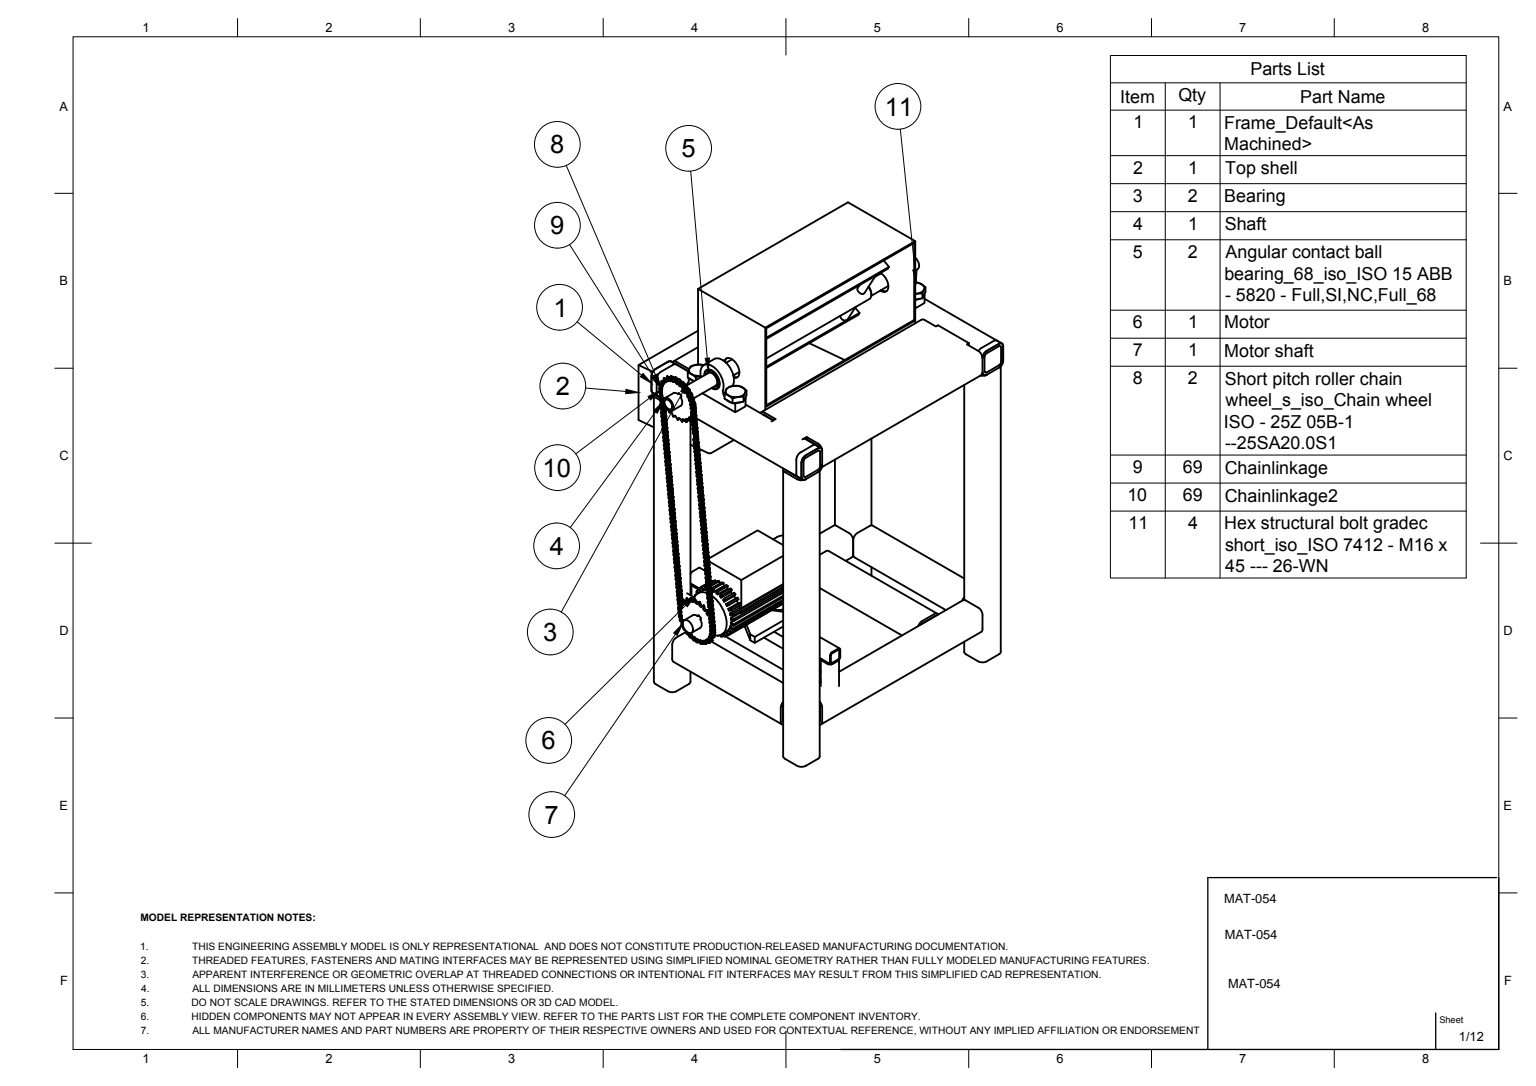
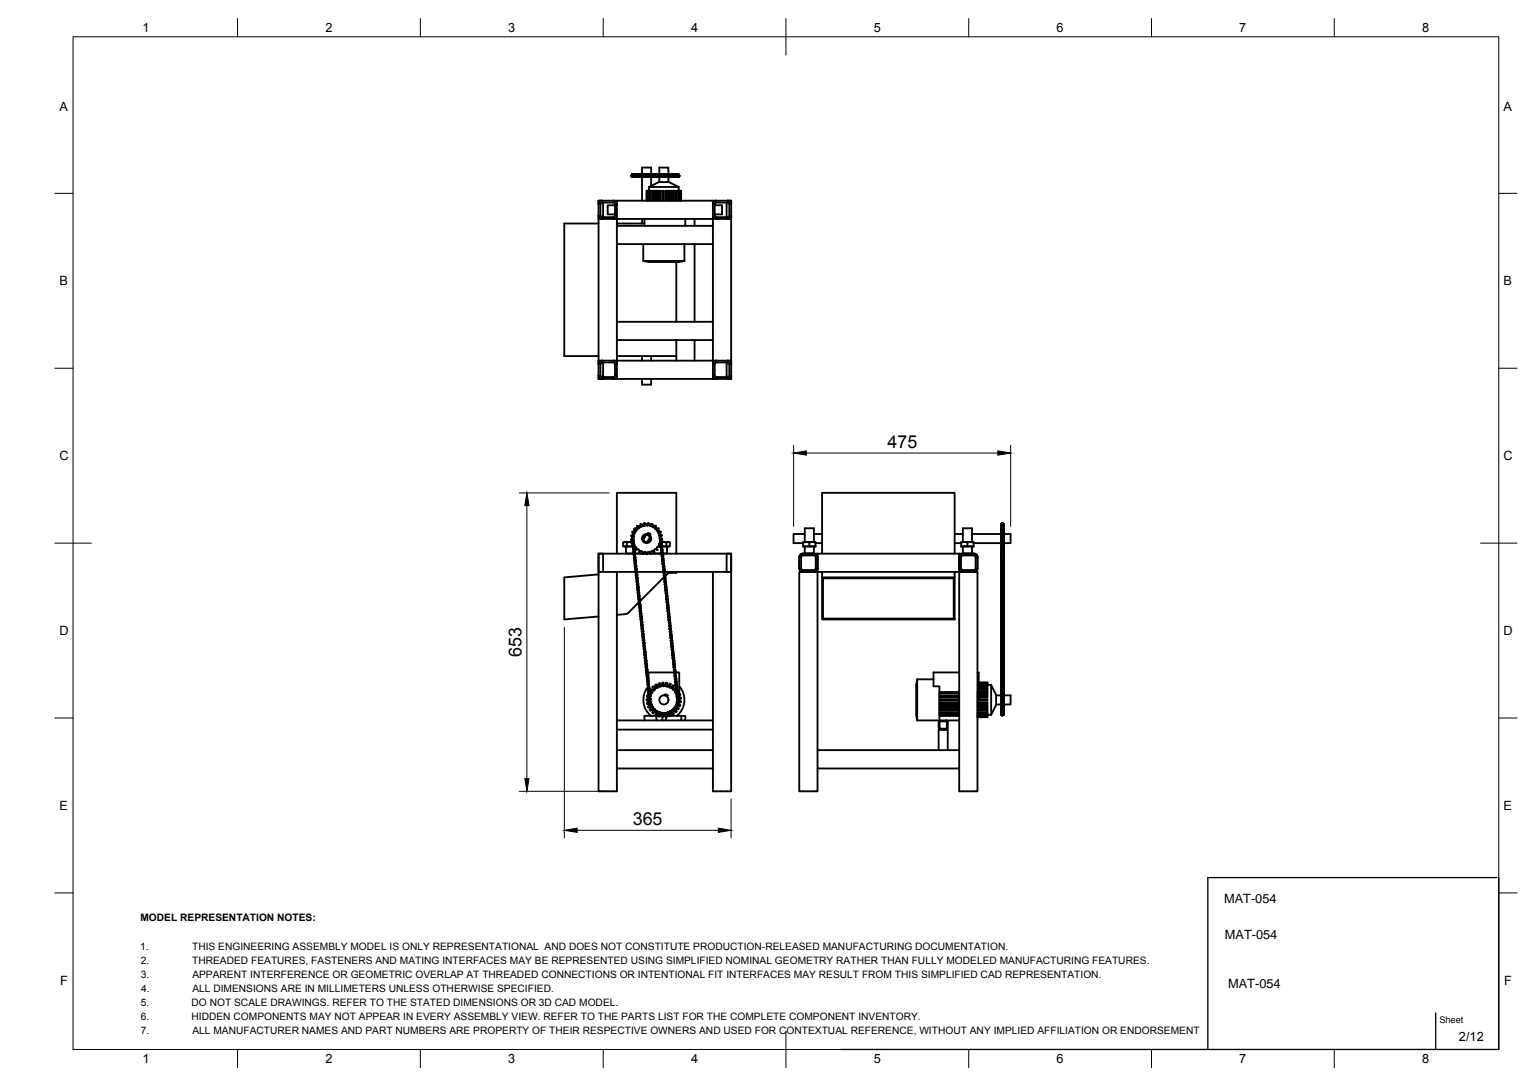
ISO-10303-21;
HEADER;
FILE_DESCRIPTION (('STEP AP214'),
    '1' );
FILE_NAME ('MAT-054',
    '2026-10-21T17:50:41',
    ( '' ),
    ( '' ),
    'SwSTEP 2.0',
    'SolidWorks 2026',
    '' );
FILE_SCHEMA (( 'AUTOMOTIVE_DESIGN' ));
ENDSEC;

DATA;
#1 = CARTESIAN_POINT ( 'NONE',  ( -499.9999999999999432, -137.0000000000000000, -155.0000000000000000 ) ) ;
#2 = ORIENTED_EDGE ( 'NONE', *, *, #27963, .F. ) ;
#3 = DIRECTION ( 'NONE',  ( 0.000000000000000000, 1.000000000000000000, 0.000000000000000000 ) ) ;
#4 = CARTESIAN_POINT ( 'NONE',  ( -19.99999999999998934, 134.9999999999999432, -162.9999999999999432 ) ) ;
#5 = CARTESIAN_POINT ( 'NONE',  ( 15.44711578872680846, -28.64595934308655956, 68.31122994652405112 ) ) ;
#6 = DIRECTION ( 'NONE',  ( -0.000000000000000000, 0.000000000000000000, -1.000000000000000000 ) ) ;
#7 = EDGE_CURVE ( 'NONE', #6804, #14714, #31558, .T. ) ;
#8 = ADVANCED_FACE ( 'NONE', ( #33361 ), #14697, .F. ) ;
#9 = CARTESIAN_POINT ( 'NONE',  ( 0.000000000000000000, -17.83604598421681331, 24.70480026434162113 ) ) ;
#10 = LINE ( 'NONE', #8370, #25873 ) ;
#11 = CARTESIAN_POINT ( 'NONE',  ( 2.789999999999999147, -7.666252171205286459, -29.49034198003814566 ) ) ;
#12 = ADVANCED_FACE ( 'NONE', ( #16842 ), #19853, .T. ) ;
#13 = ORIENTED_EDGE ( 'NONE', *, *, #11369, .F. ) ;
#14 = DIRECTION ( 'NONE',  ( 0.000000000000000000, 0.000000000000000000, -1.000000000000000000 ) ) ;
#15 = ORIENTED_EDGE ( 'NONE', *, *, #1082, .T. ) ;
#16 = VERTEX_POINT ( 'NONE', #3282 ) ;
#17 = CIRCLE ( 'NONE', #34681, 7.999999999999979572 ) ;
#18 = DIRECTION ( 'NONE',  ( -1.000000000000000000, -0.000000000000000000, -0.000000000000000000 ) ) ;
#19 = CONTEXT_DEPENDENT_SHAPE_REPRESENTATION ( #28508, #30532 ) ;
#20 = EDGE_LOOP ( 'NONE', ( #54, #27423, #18321, #7945 ) ) ;
#21 = LINE ( 'NONE', #19262, #12243 ) ;
#22 = EDGE_CURVE ( 'NONE', #26361, #15713, #881, .T. ) ;
#23 = CONTEXT_DEPENDENT_SHAPE_REPRESENTATION ( #15843, #10153 ) ;
#24 = ADVANCED_FACE ( 'NONE', ( #3974 ), #8982, .F. ) ;
#25 = LINE ( 'NONE', #27253, #34000 ) ;
#27 = EDGE_LOOP ( 'NONE', ( #3921, #9561, #6087, #4128, #28214, #30495, #16586, #17626 ) ) ;
#26 = AXIS2_PLACEMENT_3D ( 'NONE', #32504, #14502, #28009 ) ;
#28 = ORIENTED_EDGE ( 'NONE', *, *, #27270, .T. ) ;
#29 = LINE ( 'NONE', #564, #14605 ) ;
#30 = CARTESIAN_POINT ( 'NONE',  ( -23.78520691327551972, 22.21414650552148728, 68.31122994652405112 ) ) ;
#31 = EDGE_CURVE ( 'NONE', #27481, #20981, #20374, .T. ) ;
#32 = LINE ( 'NONE', #10895, #9078 ) ;
#33 = CYLINDRICAL_SURFACE ( 'NONE', #30156, 1.999999999999999556 ) ;
#34 = CARTESIAN_POINT ( 'NONE',  ( -449.9999999999999432, 137.0000000000000000, -175.0000000000000000 ) ) ;
#35 = VERTEX_POINT ( 'NONE', #17374 ) ;
#36 = DIRECTION ( 'NONE',  ( -0.4198891015602645438, 0.9075754196709571175, 0.000000000000000000 ) ) ;
#37 = DIRECTION ( 'NONE',  ( 0.000000000000000000, 1.000000000000000000, -3.421138828918010427E-49 ) ) ;
#38 = PLANE ( 'NONE',  #8347 ) ;
#39 = ADVANCED_FACE ( 'NONE', ( #31052 ), #33181, .F. ) ;
#40 = EDGE_CURVE ( 'NONE', #12730, #28037, #25521, .T. ) ;
#41 = DIRECTION ( 'NONE',  ( -1.000000000000000000, -0.000000000000000000, -0.000000000000000000 ) ) ;
#42 = DIRECTION ( 'NONE',  ( 0.000000000000000000, -1.000000000000000000, -2.465190328815662439E-32 ) ) ;
#43 = AXIS2_PLACEMENT_3D ( 'NONE', #14582, #6360, #9220 ) ;
#44 = CARTESIAN_POINT ( 'NONE',  ( -5.021133111225092982, -15.68591377522703745, -67.50000000000000000 ) ) ;
#46 = LINE ( 'NONE', #29597, #32142 ) ;
#45 = DIRECTION ( 'NONE',  ( 0.000000000000000000, -5.053935297177146739E-49, -1.000000000000000000 ) ) ;
#47 = SHAPE_REPRESENTATION ( 'frame_Default<As Machined>', ( #28566 ), #4098 ) ;
#48 = CARTESIAN_POINT ( 'NONE',  ( 8.000000000000000000, 0.000000000000000000, 0.000000000000000000 ) ) ;
#49 = EDGE_LOOP ( 'NONE', ( #24690, #13383, #3512, #29102 ) ) ;
#50 = DIRECTION ( 'NONE',  ( -1.000000000000000000, -0.000000000000000000, -0.000000000000000000 ) ) ;
#52 = DIRECTION ( 'NONE',  ( 1.000000000000000000, 0.000000000000000000, -1.848892746611746966E-32 ) ) ;
#51 = CARTESIAN_POINT ( 'NONE',  ( 11.99999999999999645, 124.9999999999999716, 194.9999999999999716 ) ) ;
#53 = B_SPLINE_CURVE_WITH_KNOTS ( 'NONE', 3,
 ( #11296, #13610, #21443, #2909 ),
 .UNSPECIFIED., .F., .F.,
 ( 4, 4 ),
 ( 1.980634265047841514E-07, 0.0006879337600918932361 ),
 .UNSPECIFIED. ) ;
#54 = ORIENTED_EDGE ( 'NONE', *, *, #21337, .T. ) ;
#55 = CIRCLE ( 'NONE', #10291, 1.154999999999999805 ) ;
#56 = CARTESIAN_POINT ( 'NONE',  ( 2.789999999999999147, -23.41952779159776199, 19.49300927180536291 ) ) ;
#57 = AXIS2_PLACEMENT_3D ( 'NONE', #27982, #32829, #17674 ) ;
#58 = ADVANCED_FACE ( 'NONE', ( #14158 ), #33712, .T. ) ;
#59 = ORIENTED_EDGE ( 'NONE', *, *, #18290, .T. ) ;
#60 = ORIENTED_EDGE ( 'NONE', *, *, #3732, .F. ) ;
#61 = DIRECTION ( 'NONE',  ( 0.000000000000000000, 6.123233995736766036E-17, 1.000000000000000000 ) ) ;
#62 = ORIENTED_EDGE ( 'NONE', *, *, #19345, .T. ) ;
#63 = ORIENTED_EDGE ( 'NONE', *, *, #23072, .F. ) ;
#64 = AXIS2_PLACEMENT_3D ( 'NONE', #13573, #18917, #21744 ) ;
#65 = PLANE ( 'NONE',  #4223 ) ;
#66 = EDGE_CURVE ( 'NONE', #35075, #4705, #9334, .T. ) ;
#67 = AXIS2_PLACEMENT_3D ( 'NONE', #32973, #22315, #1132 ) ;
#68 = EDGE_CURVE ( 'NONE', #14854, #22599, #23039, .T. ) ;
#69 = ADVANCED_FACE ( 'NONE', ( #20027 ), #30867, .F. ) ;
#70 = DIRECTION ( 'NONE',  ( -0.9766205557100867685, 0.2149704402110236834, 3.948942922735914076E-17 ) ) ;
#71 = DIRECTION ( 'NONE',  ( 0.000000000000000000, -6.870191984066554061E-16, -1.000000000000000000 ) ) ;
#72 = EDGE_LOOP ( 'NONE', ( #10606, #16036, #12165, #7623, #9118, #25813 ) ) ;
#73 = ORIENTED_EDGE ( 'NONE', *, *, #26819, .F. ) ;
#74 = DIRECTION ( 'NONE',  ( 0.000000000000000000, 0.000000000000000000, -1.000000000000000000 ) ) ;
#75 = FACE_OUTER_BOUND ( 'NONE', #24485, .T. ) ;
#76 = FACE_OUTER_BOUND ( 'NONE', #742, .T. ) ;
#77 = CARTESIAN_POINT ( 'NONE',  ( 3.235562306570555532E-30, -1.691831803474588058, -87.50000000000000000 ) ) ;
#78 = ORIENTED_EDGE ( 'NONE', *, *, #19900, .T. ) ;
#79 = DIRECTION ( 'NONE',  ( 1.000000000000000000, 0.000000000000000000, -1.848892746611746966E-32 ) ) ;
#80 = CIRCLE ( 'NONE', #11440, 7.999999999999979572 ) ;
#81 = CARTESIAN_POINT ( 'NONE',  ( -365.0000000000000000, 118.9999999999999716, 130.0000000000000000 ) ) ;
#82 = ORIENTED_EDGE ( 'NONE', *, *, #22501, .F. ) ;
#83 = AXIS2_PLACEMENT_3D ( 'NONE', #4281, #34723, #15702 ) ;
#84 = AXIS2_PLACEMENT_3D ( 'NONE', #29650, #6301, #461 ) ;
#85 = AXIS2_PLACEMENT_3D ( 'NONE', #752, #27973, #1103 ) ;
#86 = CARTESIAN_POINT ( 'NONE',  ( -20.02113311122498729, -5.758675521474015291, -67.50000000000000000 ) ) ;
#87 = DIRECTION ( 'NONE',  ( 0.000000000000000000, 1.310824597558155437E-49, 1.000000000000000000 ) ) ;
#88 = CARTESIAN_POINT ( 'NONE',  ( -1.030735741678193484, 1.713938105891546826, 0.000000000000000000 ) ) ;
#89 = FACE_OUTER_BOUND ( 'NONE', #8391, .T. ) ;
#90 = ORIENTED_EDGE ( 'NONE', *, *, #18503, .T. ) ;
#91 = FACE_OUTER_BOUND ( 'NONE', #10797, .T. ) ;
#92 = ORIENTED_EDGE ( 'NONE', *, *, #10815, .F. ) ;
#94 = CARTESIAN_POINT ( 'NONE',  ( -499.9999999999999432, 112.9999999999999574, 159.0000000000000000 ) ) ;
#93 = CARTESIAN_POINT ( 'NONE',  ( -418.0000000000000000, -112.9999999999999858, -174.9999999999999716 ) ) ;
#95 = CARTESIAN_POINT ( 'NONE',  ( 9.199999999999999289, -7.794228634059966687, -13.49999999999999822 ) ) ;
#96 = VECTOR ( 'NONE', #6013, 1000.000000000000000 ) ;
#97 = ORIENTED_EDGE ( 'NONE', *, *, #12534, .F. ) ;
#98 = CYLINDRICAL_SURFACE ( 'NONE', #29121, 7.500000000000000000 ) ;
#99 = CARTESIAN_POINT ( 'NONE',  ( -45.00000000000000000, 16.36947364650383818, 36.69637551990492597 ) ) ;
#100 = MANIFOLD_SOLID_BREP ( 'Square tube 40 X 40 X 4(1)[12]', #34815 ) ;
#101 = ORIENTED_EDGE ( 'NONE', *, *, #29088, .F. ) ;
#102 = AXIS2_PLACEMENT_3D ( 'NONE', #15826, #31812, #4404 ) ;
#103 = AXIS2_PLACEMENT_3D ( 'NONE', #2451, #30043, #5636 ) ;
#105 = ORIENTED_EDGE ( 'NONE', *, *, #3853, .F. ) ;
#104 = AXIS2_PLACEMENT_3D ( 'NONE', #26124, #29507, #9931 ) ;
#106 = CARTESIAN_POINT ( 'NONE',  ( -449.9999999999999432, -112.9999999999999858, -155.0000000000000000 ) ) ;
#107 = CARTESIAN_POINT ( 'NONE',  ( 0.000000000000000000, -29.91351748324107973, 5.799410679710550021 ) ) ;
#108 = VERTEX_POINT ( 'NONE', #26214 ) ;
#109 = VERTEX_POINT ( 'NONE', #18069 ) ;
#110 = VECTOR ( 'NONE', #12286, 1000.000000000000227 ) ;
#111 = DIRECTION ( 'NONE',  ( -1.000000000000000000, -0.000000000000000000, 0.000000000000000000 ) ) ;
#112 = ADVANCED_FACE ( 'NONE', ( #7166 ), #34411, .T. ) ;
#113 = DIRECTION ( 'NONE',  ( 0.000000000000000000, 1.717547996016640980E-15, -1.000000000000000000 ) ) ;
#114 = EDGE_CURVE ( 'NONE', #27996, #34376, #12253, .T. ) ;
#115 = CARTESIAN_POINT ( 'NONE',  ( 1.749999999999999778, -10.89151784028265624, -32.64600270996228204 ) ) ;
#116 = CARTESIAN_POINT ( 'NONE',  ( 9.199999999999999289, 7.794228634059941818, 13.49999999999999645 ) ) ;
#117 = ORIENTED_EDGE ( 'NONE', *, *, #2620, .T. ) ;
#118 = ORIENTED_EDGE ( 'NONE', *, *, #1367, .F. ) ;
#119 = LINE ( 'NONE', #24139, #24170 ) ;
#120 = CARTESIAN_POINT ( 'NONE',  ( -418.0000000000000000, -105.0000000000000142, -73.99999999999998579 ) ) ;
#121 = EDGE_CURVE ( 'NONE', #19542, #7373, #4262, .T. ) ;
#122 = CARTESIAN_POINT ( 'NONE',  ( -35.00000000000000000, -46.95407462254104303, -36.69637551990492597 ) ) ;
#123 = DIRECTION ( 'NONE',  ( -0.000000000000000000, -0.000000000000000000, -1.000000000000000000 ) ) ;
#124 = LINE ( 'NONE', #5791, #25297 ) ;
#126 = LINE ( 'NONE', #30027, #31126 ) ;
#125 =( REPRESENTATION_RELATIONSHIP ('NONE','NONE', #23037, #28231 ) REPRESENTATION_RELATIONSHIP_WITH_TRANSFORMATION ( #1643 )SHAPE_REPRESENTATION_RELATIONSHIP( ) );
#127 = CARTESIAN_POINT ( 'NONE',  ( 11.99999999999999645, 124.9999999999999716, 190.9999999999999716 ) ) ;
#128 = EDGE_LOOP ( 'NONE', ( #27295, #34610, #28913, #17445 ) ) ;
#129 = CARTESIAN_POINT ( 'NONE',  ( 9.199999999999999289, -7.794228634059966687, -13.49999999999999822 ) ) ;
#130 = EDGE_CURVE ( 'NONE', #18108, #30234, #23613, .T. ) ;
#131 = CARTESIAN_POINT ( 'NONE',  ( 1.039999999999999591, -18.21166265554809627, 29.20140402659733425 ) ) ;
#132 = CARTESIAN_POINT ( 'NONE',  ( -499.9999999999999432, 140.9999999999999716, -162.9999999999999716 ) ) ;
#133 = ORIENTED_EDGE ( 'NONE', *, *, #21122, .F. ) ;
#134 = AXIS2_PLACEMENT_3D ( 'NONE', #22862, #33708, #9328 ) ;
#135 = CARTESIAN_POINT ( 'NONE',  ( -441.9999999999999432, -104.9999999999999716, -190.9999999999999716 ) ) ;
#136 = EDGE_LOOP ( 'NONE', ( #10690, #4855, #133, #33486, #30185, #13307, #10749, #25225 ) ) ;
#137 = CARTESIAN_POINT ( 'NONE',  ( -110.0810685637187021, 0.6776097359754142957, -12.48599830169775871 ) ) ;
#138 = DIRECTION ( 'NONE',  ( 0.000000000000000000, 0.000000000000000000, -1.000000000000000000 ) ) ;
#139 = ORIENTED_EDGE ( 'NONE', *, *, #14829, .T. ) ;
#140 = CARTESIAN_POINT ( 'NONE',  ( -12.00000000000001066, -124.9999999999999432, -162.9999999999999432 ) ) ;
#141 = CARTESIAN_POINT ( 'NONE',  ( 28.11866956577618382, 16.38733641342591696, 68.31122994652405112 ) ) ;
#142 = DIRECTION ( 'NONE',  ( 0.05413890858541774848, -0.9985334138511239299, -1.834276123671687566E-16 ) ) ;
#143 = VERTEX_POINT ( 'NONE', #21234 ) ;
#144 = EDGE_LOOP ( 'NONE', ( #280, #13285, #21736, #21392, #14585, #6579, #11215, #29408, #31879, #667, #8768, #28527, #21247 ) ) ;
#145 = CARTESIAN_POINT ( 'NONE',  ( 839.5113038710145474, 1138.540472633347918, 1753.598338701303419 ) ) ;
#146 = CARTESIAN_POINT ( 'NONE',  ( -9.978866888775527855, 8.235406450278430768, -87.50000000000000000 ) ) ;
#147 = B_SPLINE_CURVE_WITH_KNOTS ( 'NONE', 3,
 ( #10015, #12703, #20870, #26557, #32247, #23363 ),
 .UNSPECIFIED., .F., .F.,
 ( 4, 2, 4 ),
 ( 2.446897702420577325E-07, 0.001873443032870420388, 0.003746641375970598611 ),
 .UNSPECIFIED. ) ;
#148 = ORIENTED_EDGE ( 'NONE', *, *, #23576, .T. ) ;
#149 = CARTESIAN_POINT ( 'NONE',  ( 3.235562306570555532E-30, 28.08988295778447508, -67.50000000000000000 ) ) ;
#150 = EDGE_CURVE ( 'NONE', #25913, #33864, #29280, .T. ) ;
#151 = AXIS2_PLACEMENT_3D ( 'NONE', #16414, #32397, #24554 ) ;
#152 = B_SPLINE_CURVE_WITH_KNOTS ( 'NONE', 3,
 ( #1584, #18327, #31299, #33977, #2108, #6909 ),
 .UNSPECIFIED., .F., .F.,
 ( 4, 2, 4 ),
 ( 4.404817104455272006E-07, 0.001874269680285309877, 0.003748098878860173927 ),
 .UNSPECIFIED. ) ;
#153 = FACE_OUTER_BOUND ( 'NONE', #33687, .T. ) ;
#154 = AXIS2_PLACEMENT_3D ( 'NONE', #33975, #1065, #20629 ) ;
#155 = DIRECTION ( 'NONE',  ( 1.000000000000000000, 0.000000000000000000, 0.000000000000000000 ) ) ;
#156 = CARTESIAN_POINT ( 'NONE',  ( -109.6397584259853915, -2.159755022470678298, 7.184107906894084294 ) ) ;
#158 = VECTOR ( 'NONE', #14520, 1000.000000000000000 ) ;
#157 = CONTEXT_DEPENDENT_SHAPE_REPRESENTATION ( #30116, #15462 ) ;
#159 = ORIENTED_EDGE ( 'NONE', *, *, #4581, .F. ) ;
#160 = ORIENTED_EDGE ( 'NONE', *, *, #17632, .T. ) ;
#161 = AXIS2_PLACEMENT_3D ( 'NONE', #27880, #20415, #25206 ) ;
#162 = ORIENTED_EDGE ( 'NONE', *, *, #7088, .T. ) ;
#163 = EDGE_CURVE ( 'NONE', #29138, #16548, #8258, .T. ) ;
#164 = DIRECTION ( 'NONE',  ( -1.000000000000000000, -0.000000000000000000, -0.000000000000000000 ) ) ;
#165 = ADVANCED_FACE ( 'NONE', ( #4848 ), #1498, .F. ) ;
#166 = DIRECTION ( 'NONE',  ( 1.000000000000000000, 0.000000000000000000, -1.232595164407831220E-32 ) ) ;
#167 = DIRECTION ( 'NONE',  ( 0.000000000000000000, 1.000000000000000000, 0.000000000000000000 ) ) ;
#168 = ORIENTED_EDGE ( 'NONE', *, *, #16056, .F. ) ;
#169 = VERTEX_POINT ( 'NONE', #10028 ) ;
#170 = ADVANCED_FACE ( 'NONE', ( #26571 ), #17893, .T. ) ;
#171 = EDGE_CURVE ( 'NONE', #17976, #25124, #32703, .T. ) ;
#172 = DIRECTION ( 'NONE',  ( 0.000000000000000000, 1.310824597558155437E-49, 1.000000000000000000 ) ) ;
#173 = VERTEX_POINT ( 'NONE', #23733 ) ;
#174 = DIRECTION ( 'NONE',  ( -0.000000000000000000, 1.000000000000000000, -0.000000000000000000 ) ) ;
#175 = EDGE_CURVE ( 'NONE', #17916, #26514, #22520, .T. ) ;
#176 = DIRECTION ( 'NONE',  ( 0.000000000000000000, 0.000000000000000000, 1.000000000000000000 ) ) ;
#177 = ORIENTED_EDGE ( 'NONE', *, *, #24168, .F. ) ;
#178 = ORIENTED_EDGE ( 'NONE', *, *, #30215, .F. ) ;
#179 = DIRECTION ( 'NONE',  ( -0.000000000000000000, -1.000000000000000000, -0.000000000000000000 ) ) ;
#180 = FACE_OUTER_BOUND ( 'NONE', #24704, .T. ) ;
#181 = VERTEX_POINT ( 'NONE', #21756 ) ;
#182 = LINE ( 'NONE', #27055, #31152 ) ;
#183 = CARTESIAN_POINT ( 'NONE',  ( 1.749999999999999778, 32.09669216789253454, -12.41728656686340138 ) ) ;
#184 = DIRECTION ( 'NONE',  ( 0.000000000000000000, 0.000000000000000000, 1.000000000000000000 ) ) ;
#186 = CARTESIAN_POINT ( 'NONE',  ( 8.000000000000000000, 0.000000000000000000, -14.19999999999999929 ) ) ;
#185 = AXIS2_PLACEMENT_3D ( 'NONE', #11007, #6874, #14922 ) ;
#187 = CIRCLE ( 'NONE', #747, 5.738084889453667792 ) ;
#188 = TOROIDAL_SURFACE ( 'NONE', #34853, 30.47050528711512030, 8.000000000000000000 ) ;
#189 = AXIS2_PLACEMENT_3D ( 'NONE', #223, #13410, #11088 ) ;
#190 = LINE ( 'NONE', #16406, #20541 ) ;
#191 = CARTESIAN_POINT ( 'NONE',  ( 2.789999999999999147, -1.291199951812987523, -30.41225463960053332 ) ) ;
#192 = VERTEX_POINT ( 'NONE', #13936 ) ;
#193 = DIRECTION ( 'NONE',  ( 0.000000000000000000, -1.000000000000000000, 0.000000000000000000 ) ) ;
#194 = DIRECTION ( 'NONE',  ( -6.982748503361914938E-15, 6.990337062275685868E-15, -1.000000000000000000 ) ) ;
#195 = ORIENTED_EDGE ( 'NONE', *, *, #25088, .F. ) ;
#196 = VERTEX_POINT ( 'NONE', #27097 ) ;
#197 = VECTOR ( 'NONE', #17016, 1000.000000000000000 ) ;
#198 = CARTESIAN_POINT ( 'NONE',  ( 105.9801405217367147, 5.657025933901884684, 4.924586583110066584 ) ) ;
#199 = VERTEX_POINT ( 'NONE', #26920 ) ;
#200 = CARTESIAN_POINT ( 'NONE',  ( -35.71762877834949990, -12.58147180936565057, -36.68877005347593467 ) ) ;
#201 = AXIS2_PLACEMENT_3D ( 'NONE', #23656, #27026, #24343 ) ;
#202 = B_SPLINE_CURVE_WITH_KNOTS ( 'NONE', 3,
 ( #7828, #4974, #32217, #8004, #26873, #2488, #32384, #18882 ),
 .UNSPECIFIED., .F., .F.,
 ( 4, 2, 2, 4 ),
 ( 0.007886720825438783139, 0.009850969036563994238, 0.01181521724768920534, 0.01574371366993962407 ),
 .UNSPECIFIED. ) ;
#204 = FACE_OUTER_BOUND ( 'NONE', #17444, .T. ) ;
#203 = CARTESIAN_POINT ( 'NONE',  ( -349.0000000000000000, 134.9999999999999716, 113.9999999999999858 ) ) ;
#205 = TOROIDAL_SURFACE ( 'NONE', #2485, 30.47050528711512030, 8.000000000000000000 ) ;
#206 = ORIENTED_EDGE ( 'NONE', *, *, #33017, .T. ) ;
#207 = ORIENTED_EDGE ( 'NONE', *, *, #14796, .T. ) ;
#208 = ADVANCED_FACE ( 'NONE', ( #18929 ), #2537, .T. ) ;
#209 = EDGE_CURVE ( 'NONE', #25754, #24825, #34950, .T. ) ;
#210 = AXIS2_PLACEMENT_3D ( 'NONE', #14613, #8714, #19766 ) ;
#211 = CARTESIAN_POINT ( 'NONE',  ( -15.99999999999998579, 124.9999999999999716, 162.9999999999999716 ) ) ;
#212 = DIRECTION ( 'NONE',  ( 0.000000000000000000, 0.000000000000000000, 1.000000000000000000 ) ) ;
#213 = CYLINDRICAL_SURFACE ( 'NONE', #21558, 7.999999999999979572 ) ;
#214 = CARTESIAN_POINT ( 'NONE',  ( -20.02113311122498729, -3.725253662474303784, -67.50000000000000000 ) ) ;
#215 = LINE ( 'NONE', #29415, #4585 ) ;
#216 = ORIENTED_EDGE ( 'NONE', *, *, #5166, .F. ) ;
#217 = CYLINDRICAL_SURFACE ( 'NONE', #9558, 3.999999999999976019 ) ;
#218 = CARTESIAN_POINT ( 'NONE',  ( 1.749999999999999778, -33.26546734453825849, 8.820166447041632551 ) ) ;
#219 = CARTESIAN_POINT ( 'NONE',  ( -500.0000000000000000, -137.0000000000000000, 190.9999999999999716 ) ) ;
#220 = CARTESIAN_POINT ( 'NONE',  ( 0.5248942730704680981, -11.05013152551600442, -31.49770363594219091 ) ) ;
#221 =( NAMED_UNIT ( * ) PLANE_ANGLE_UNIT ( ) SI_UNIT ( $, .RADIAN. ) );
#222 = EDGE_CURVE ( 'NONE', #22062, #30310, #29769, .T. ) ;
#223 = CARTESIAN_POINT ( 'NONE',  ( 0.000000000000000000, 3.524919873834583163E-15, 68.31122994652405112 ) ) ;
#225 = DIRECTION ( 'NONE',  ( 0.000000000000000000, 0.000000000000000000, 1.000000000000000000 ) ) ;
#224 = CARTESIAN_POINT ( 'NONE',  ( 143.0000000000000568, -90.29102463692673552, -73.95413108702813076 ) ) ;
#226 = CIRCLE ( 'NONE', #8162, 1.999999999999999112 ) ;
#227 = CARTESIAN_POINT ( 'NONE',  ( -8.297462993384987146E-14, 27.83741677616693266, 12.85620214406761086 ) ) ;
#228 = ORIENTED_EDGE ( 'NONE', *, *, #6017, .T. ) ;
#229 = DIRECTION ( 'NONE',  ( 1.000000000000000000, 0.000000000000000000, 0.000000000000000000 ) ) ;
#230 = LINE ( 'NONE', #27103, #6038 ) ;
#231 = EDGE_CURVE ( 'NONE', #21456, #4465, #34436, .T. ) ;
#232 = EDGE_CURVE ( 'NONE', #29036, #32413, #15921, .T. ) ;
#233 = PRODUCT_DEFINITION_FORMATION_WITH_SPECIFIED_SOURCE ( 'ANY', '', #8627, .NOT_KNOWN. ) ;
#234 = EDGE_CURVE ( 'NONE', #30170, #27211, #3153, .T. ) ;
#236 = ORIENTED_EDGE ( 'NONE', *, *, #29739, .F. ) ;
#235 = CIRCLE ( 'NONE', #12751, 3.999999999999976019 ) ;
#237 = AXIS2_PLACEMENT_3D ( 'NONE', #28026, #9683, #31396 ) ;
#238 = DIRECTION ( 'NONE',  ( 0.000000000000000000, 0.000000000000000000, 1.000000000000000000 ) ) ;
#239 = AXIS2_PLACEMENT_3D ( 'NONE', #27640, #18947, #27283 ) ;
#240 = EDGE_CURVE ( 'NONE', #16352, #20441, #2589, .T. ) ;
#241 = ORIENTED_EDGE ( 'NONE', *, *, #17416, .F. ) ;
#242 = ORIENTED_EDGE ( 'NONE', *, *, #21753, .F. ) ;
#243 = CARTESIAN_POINT ( 'NONE',  ( 22.89764159710611224, 17.63622956525712127, -77.50000000000000000 ) ) ;
#244 = ORIENTED_EDGE ( 'NONE', *, *, #13986, .T. ) ;
#245 = VERTEX_POINT ( 'NONE', #5376 ) ;
#246 = CARTESIAN_POINT ( 'NONE',  ( 8.000000000000000000, 0.000000000000000000, -15.69999999999999929 ) ) ;
#247 = CONTEXT_DEPENDENT_SHAPE_REPRESENTATION ( #8067, #13594 ) ;
#248 = AXIS2_PLACEMENT_3D ( 'NONE', #6880, #17771, #4383 ) ;
#249 = DIRECTION ( 'NONE',  ( -1.000000000000000000, 0.000000000000000000, 0.000000000000000000 ) ) ;
#250 = CARTESIAN_POINT ( 'NONE',  ( -500.0000000000000000, 112.9999999999999574, 155.0000000000000000 ) ) ;
#251 = ORIENTED_EDGE ( 'NONE', *, *, #8791, .F. ) ;
#252 = ORIENTED_EDGE ( 'NONE', *, *, #16950, .T. ) ;
#253 = EDGE_CURVE ( 'NONE', #5102, #23161, #21417, .T. ) ;
#254 = CARTESIAN_POINT ( 'NONE',  ( 32.30227131129396412, -3.970848902647437395, 68.31122994652405112 ) ) ;
#255 = DIRECTION ( 'NONE',  ( -0.3701381553399132329, -0.9289767198167918627, 0.000000000000000000 ) ) ;
#256 = VECTOR ( 'NONE', #18006, 1000.000000000000000 ) ;
#257 = CARTESIAN_POINT ( 'NONE',  ( 106.5104497542385928, -5.548707632555109015, -11.20129239819138967 ) ) ;
#258 = CARTESIAN_POINT ( 'NONE',  ( 2.789999999999999147, -25.83993731729808729, 18.77381338200959604 ) ) ;
#259 = ORIENTED_EDGE ( 'NONE', *, *, #5135, .T. ) ;
#260 = ORIENTED_EDGE ( 'NONE', *, *, #32935, .F. ) ;
#261 = LINE ( 'NONE', #33170, #9980 ) ;
#262 = VECTOR ( 'NONE', #31181, 1000.000000000000000 ) ;
#263 = AXIS2_PLACEMENT_3D ( 'NONE', #22124, #50, #11096 ) ;
#264 = DIRECTION ( 'NONE',  ( 1.000000000000000000, 0.000000000000000000, 0.000000000000000000 ) ) ;
#265 = EDGE_LOOP ( 'NONE', ( #34746, #139, #23845, #12635, #26310, #31196, #6266, #393 ) ) ;
#266 = CARTESIAN_POINT ( 'NONE',  ( 15.99999999999998579, 4.559999999999908127, 168.2400000000000091 ) ) ;
#267 = CARTESIAN_POINT ( 'NONE',  ( 0.000000000000000000, -7.666252171205264254, -29.49034198003815632 ) ) ;
#268 = CARTESIAN_POINT ( 'NONE',  ( 5.021133111224369117, -1.691831803474588058, -87.50000000000000000 ) ) ;
#269 = CARTESIAN_POINT ( 'NONE',  ( 0.000000000000000000, 6.992329373473909019E-15, 49.43553178847298568 ) ) ;
#270 = ORIENTED_EDGE ( 'NONE', *, *, #32963, .T. ) ;
#271 = FACE_OUTER_BOUND ( 'NONE', #6766, .T. ) ;
#272 = ORIENTED_EDGE ( 'NONE', *, *, #3278, .F. ) ;
#273 = EDGE_CURVE ( 'NONE', #17170, #26514, #10910, .T. ) ;
#275 = CARTESIAN_POINT ( 'NONE',  ( -130.6469666100234406, 6.000000000000000000, 57.49999999999999289 ) ) ;
#274 = DIRECTION ( 'NONE',  ( 0.000000000000000000, 0.000000000000000000, 1.000000000000000000 ) ) ;
#276 = DIRECTION ( 'NONE',  ( 0.000000000000000000, 0.000000000000000000, -1.000000000000000000 ) ) ;
#277 = EDGE_CURVE ( 'NONE', #32572, #17435, #29890, .T. ) ;
#278 = ADVANCED_FACE ( 'NONE', ( #16441 ), #5428, .T. ) ;
#279 = CIRCLE ( 'NONE', #22435, 4.682234377621698584 ) ;
#280 = ORIENTED_EDGE ( 'NONE', *, *, #30246, .T. ) ;
#281 = CARTESIAN_POINT ( 'NONE',  ( -499.9999999999999432, -137.0000000000000000, -190.9999999999999716 ) ) ;
#282 = CARTESIAN_POINT ( 'NONE',  ( -35.00000000000000000, 0.000000000000000000, 0.000000000000000000 ) ) ;
#283 = CIRCLE ( 'NONE', #32662, 4.682234377621698584 ) ;
#284 = EDGE_LOOP ( 'NONE', ( #25209, #30307, #21311, #18042 ) ) ;
#285 = VECTOR ( 'NONE', #12711, 1000.000000000000000 ) ;
#286 = ORIENTED_EDGE ( 'NONE', *, *, #4793, .F. ) ;
#287 = VECTOR ( 'NONE', #30917, 1000.000000000000000 ) ;
#288 = AXIS2_PLACEMENT_3D ( 'NONE', #34150, #4414, #26138 ) ;
#289 = ORIENTED_EDGE ( 'NONE', *, *, #26141, .T. ) ;
#290 = CARTESIAN_POINT ( 'NONE',  ( -418.0000000000000000, 113.0000000000000000, 154.9999999999999716 ) ) ;
#291 = CARTESIAN_POINT ( 'NONE',  ( -101.1657792522907329, 3.400963087932908024, 6.689628992625340942 ) ) ;
#292 = VERTEX_POINT ( 'NONE', #13238 ) ;
#293 = ORIENTED_EDGE ( 'NONE', *, *, #23924, .F. ) ;
#294 = CARTESIAN_POINT ( 'NONE',  ( -10.00000000000000000, 0.000000000000000000, 0.000000000000000000 ) ) ;
#295 = CARTESIAN_POINT ( 'NONE',  ( -445.9999999999999432, -137.0000000000000000, 154.9999999999999716 ) ) ;
#296 = DIRECTION ( 'NONE',  ( 0.000000000000000000, 1.000000000000000000, 0.000000000000000000 ) ) ;
#297 = LINE ( 'NONE', #7943, #15401 ) ;
#298 = ORIENTED_EDGE ( 'NONE', *, *, #4872, .T. ) ;
#299 = ORIENTED_EDGE ( 'NONE', *, *, #29304, .T. ) ;
#300 = DIRECTION ( 'NONE',  ( 1.000000000000000000, 3.040835319149746528E-31, 1.232595164407830946E-32 ) ) ;
#301 = CARTESIAN_POINT ( 'NONE',  ( 2.033589663487044952, 13.95893286369055097, -30.90974742850055179 ) ) ;
#302 = CARTESIAN_POINT ( 'NONE',  ( -12.00000000000001066, -109.0000000000000142, 155.0000000000000000 ) ) ;
#303 = DIRECTION ( 'NONE',  ( -0.9985334138511239299, -0.05413890858541774848, -0.000000000000000000 ) ) ;
#304 = VECTOR ( 'NONE', #8203, 1000.000000000000000 ) ;
#305 = LINE ( 'NONE', #11698, #310 ) ;
#306 = DIRECTION ( 'NONE',  ( -0.000000000000000000, -0.000000000000000000, -1.000000000000000000 ) ) ;
#307 = DIRECTION ( 'NONE',  ( 0.000000000000000000, 0.000000000000000000, 1.000000000000000000 ) ) ;
#308 = ORIENTED_EDGE ( 'NONE', *, *, #21108, .F. ) ;
#309 = VECTOR ( 'NONE', #16304, 1000.000000000000000 ) ;
#310 = VECTOR ( 'NONE', #22368, 999.9999999999998863 ) ;
#311 = DIRECTION ( 'NONE',  ( 0.000000000000000000, -0.000000000000000000, -1.000000000000000000 ) ) ;
#312 = CARTESIAN_POINT ( 'NONE',  ( 2.789999999999999147, 7.350529080603967813, -30.20932655202929595 ) ) ;
#313 = ORIENTED_EDGE ( 'NONE', *, *, #17871, .T. ) ;
#314 = CYLINDRICAL_SURFACE ( 'NONE', #12647, 1.649999999999999911 ) ;
#315 = ORIENTED_EDGE ( 'NONE', *, *, #26179, .T. ) ;
#316 = VECTOR ( 'NONE', #20254, 1000.000000000000000 ) ;
#317 = VECTOR ( 'NONE', #9866, 1000.000000000000000 ) ;
#318 = CARTESIAN_POINT ( 'NONE',  ( 32.40067729534749219, 3.066020821660472517, 68.31122994652405112 ) ) ;
#319 = VERTEX_POINT ( 'NONE', #27272 ) ;
#320 = CARTESIAN_POINT ( 'NONE',  ( 1.749999999999999778, 0.000000000000000000, 0.000000000000000000 ) ) ;
#322 = AXIS2_PLACEMENT_3D ( 'NONE', #10565, #32080, #10742 ) ;
#321 = CARTESIAN_POINT ( 'NONE',  ( 11.99999999999999645, -124.9999999999999432, -154.9999999999999716 ) ) ;
#323 = EDGE_CURVE ( 'NONE', #17531, #2097, #46, .T. ) ;
#324 = EDGE_CURVE ( 'NONE', #31410, #8890, #5192, .T. ) ;
#325 = EDGE_CURVE ( 'NONE', #23614, #34805, #30448, .T. ) ;
#326 = ORIENTED_EDGE ( 'NONE', *, *, #11265, .T. ) ;
#327 = DIRECTION ( 'NONE',  ( -0.000000000000000000, -1.000000000000000000, -0.000000000000000000 ) ) ;
#328 = CARTESIAN_POINT ( 'NONE',  ( 2.789999999999999147, 0.000000000000000000, 0.000000000000000000 ) ) ;
#330 = DIRECTION ( 'NONE',  ( 0.000000000000000000, -1.224646799147353207E-16, 1.000000000000000000 ) ) ;
#329 = PRODUCT_DEFINITION ( 'UNKNOWN', '', #233, #29569 ) ;
#331 = ORIENTED_EDGE ( 'NONE', *, *, #24983, .F. ) ;
#332 = VECTOR ( 'NONE', #22185, 999.9999999999998863 ) ;
#333 = EDGE_LOOP ( 'NONE', ( #9601, #2215, #28741, #29275, #5602, #22316, #13085, #21357 ) ) ;
#334 = CARTESIAN_POINT ( 'NONE',  ( 827.0635550463485970, 1254.876359783047747, 1753.598338701303419 ) ) ;
#335 = CARTESIAN_POINT ( 'NONE',  ( 0.000000000000000000, 0.000000000000000000, 0.000000000000000000 ) ) ;
#336 = ORIENTED_EDGE ( 'NONE', *, *, #6534, .F. ) ;
#337 = AXIS2_PLACEMENT_3D ( 'NONE', #12188, #9323, #17539 ) ;
#338 = PLANE ( 'NONE',  #21235 ) ;
#339 = SURFACE_STYLE_FILL_AREA ( #24699 ) ;
#340 = CARTESIAN_POINT ( 'NONE',  ( 3.235562306570555532E-30, -1.691831803474591833, -67.50000000000000000 ) ) ;
#341 = CARTESIAN_POINT ( 'NONE',  ( -103.3057560645484045, -4.837552664684794834, 5.733718144795171945 ) ) ;
#342 = CONTEXT_DEPENDENT_SHAPE_REPRESENTATION ( #19220, #7187 ) ;
#343 = ORIENTED_EDGE ( 'NONE', *, *, #19695, .F. ) ;
#345 = ORIENTED_EDGE ( 'NONE', *, *, #32175, .T. ) ;
#344 =( REPRESENTATION_RELATIONSHIP ('NONE','NONE', #23037, #15767 ) REPRESENTATION_RELATIONSHIP_WITH_TRANSFORMATION ( #13168 )SHAPE_REPRESENTATION_RELATIONSHIP( ) );
#346 = ORIENTED_EDGE ( 'NONE', *, *, #29604, .F. ) ;
#347 = DIRECTION ( 'NONE',  ( 0.000000000000000000, -1.000000000000000000, -2.465190328815662439E-32 ) ) ;
#348 = VECTOR ( 'NONE', #16267, 1000.000000000000000 ) ;
#349 = CARTESIAN_POINT ( 'NONE',  ( 0.000000000000000000, -30.41598411195408502, -1.821977758773957179 ) ) ;
#350 = CARTESIAN_POINT ( 'NONE',  ( 105.0000000000000000, 0.000000000000000000, 60.00000000000000000 ) ) ;
#351 = ORIENTED_EDGE ( 'NONE', *, *, #29532, .T. ) ;
#352 = ORIENTED_EDGE ( 'NONE', *, *, #24437, .F. ) ;
#353 = CARTESIAN_POINT ( 'NONE',  ( 5.021133111224679091, 26.05646109878476224, -67.50000000000000000 ) ) ;
#354 = ORIENTED_EDGE ( 'NONE', *, *, #15930, .T. ) ;
#355 = CARTESIAN_POINT ( 'NONE',  ( -20.00000000000007461, 104.9999999999999858, -162.9999999999999716 ) ) ;
#356 = CARTESIAN_POINT ( 'NONE',  ( -414.0000000000000568, -124.9999999999999858, -77.99999999999997158 ) ) ;
#357 = ORIENTED_EDGE ( 'NONE', *, *, #28689, .F. ) ;
#358 = EDGE_LOOP ( 'NONE', ( #6537, #22025, #25095, #26334 ) ) ;
#359 = CIRCLE ( 'NONE', #19122, 3.999999999999976019 ) ;
#360 = CYLINDRICAL_SURFACE ( 'NONE', #25416, 2.033421858999710619 ) ;
#361 = EDGE_CURVE ( 'NONE', #12124, #30243, #11090, .T. ) ;
#362 = DIRECTION ( 'NONE',  ( -0.000000000000000000, 1.000000000000000000, -0.000000000000000000 ) ) ;
#363 = ORIENTED_EDGE ( 'NONE', *, *, #34633, .T. ) ;
#364 = VECTOR ( 'NONE', #34672, 1000.000000000000000 ) ;
#365 = DIRECTION ( 'NONE',  ( 0.000000000000000000, 1.000000000000000000, 5.145227585319922065E-49 ) ) ;
#366 = DIRECTION ( 'NONE',  ( 0.000000000000000000, 0.000000000000000000, 1.000000000000000000 ) ) ;
#367 = EDGE_CURVE ( 'NONE', #31738, #21426, #28743, .T. ) ;
#368 = LINE ( 'NONE', #5152, #16717 ) ;
#369 = CARTESIAN_POINT ( 'NONE',  ( 22.89764159710613001, 8.346743312457581609, -87.50000000000000000 ) ) ;
#370 = CARTESIAN_POINT ( 'NONE',  ( -19.99999999999998934, 144.9999999999999147, 162.9999999999999716 ) ) ;
#371 = PLANE ( 'NONE',  #32639 ) ;
#373 = EDGE_CURVE ( 'NONE', #12936, #16352, #14295, .T. ) ;
#372 = PLANE ( 'NONE',  #748 ) ;
#374 = AXIS2_PLACEMENT_3D ( 'NONE', #31781, #29476, #5070 ) ;
#375 = ORIENTED_EDGE ( 'NONE', *, *, #8635, .T. ) ;
#376 = ADVANCED_FACE ( 'NONE', ( #22293 ), #33492, .T. ) ;
#377 = LINE ( 'NONE', #5513, #1804 ) ;
#378 = DIRECTION ( 'NONE',  ( 0.1063910735368947813, -0.9943243633099144718, -3.335902418024520312E-15 ) ) ;
#379 = ORIENTED_EDGE ( 'NONE', *, *, #10888, .T. ) ;
#380 = ORIENTED_EDGE ( 'NONE', *, *, #13916, .T. ) ;
#381 = EDGE_CURVE ( 'NONE', #23842, #27991, #33323, .T. ) ;
#382 = EDGE_CURVE ( 'NONE', #29286, #20322, #3767, .T. ) ;
#383 = VECTOR ( 'NONE', #16250, 1000.000000000000114 ) ;
#384 = CARTESIAN_POINT ( 'NONE',  ( 145.0000000000000568, -87.50000000000000000, 65.00000000000000000 ) ) ;
#385 = EDGE_LOOP ( 'NONE', ( #22303, #2960 ) ) ;
#386 = CARTESIAN_POINT ( 'NONE',  ( -349.0000000000000000, -125.0000000000000284, 168.9999999999999716 ) ) ;
#387 = AXIS2_PLACEMENT_3D ( 'NONE', #34628, #13273, #5228 ) ;
#388 = CARTESIAN_POINT ( 'NONE',  ( -499.9999999999999432, 136.9999999999999432, -159.0000000000000000 ) ) ;
#389 = ITEM_DEFINED_TRANSFORMATION ( 'NONE', 'NONE', #34327,  #28566 ) ;
#391 = CARTESIAN_POINT ( 'NONE',  ( 2.261199744108339349, -18.53787122671715082, -27.77096539590149504 ) ) ;
#390 = DIRECTION ( 'NONE',  ( 0.000000000000000000, 0.000000000000000000, -1.000000000000000000 ) ) ;
#392 = VERTEX_POINT ( 'NONE', #6605 ) ;
#393 = ORIENTED_EDGE ( 'NONE', *, *, #6508, .T. ) ;
#394 = CARTESIAN_POINT ( 'NONE',  ( -36.80830595996284416, 8.862931941313791029, -36.68877005347593467 ) ) ;
#395 = CARTESIAN_POINT ( 'NONE',  ( -355.0000000000000000, 132.9999999999999716, 113.9999999999999858 ) ) ;
#396 = AXIS2_PLACEMENT_3D ( 'NONE', #7173, #18412, #15218 ) ;
#397 = LINE ( 'NONE', #6768, #1059 ) ;
#398 = CARTESIAN_POINT ( 'NONE',  ( -499.9999999999999432, -137.0000000000000000, -159.0000000000000000 ) ) ;
#399 = DIRECTION ( 'NONE',  ( 0.000000000000000000, 1.836970198721029934E-16, -1.000000000000000000 ) ) ;
#400 = ORIENTED_EDGE ( 'NONE', *, *, #18488, .T. ) ;
#401 = DIRECTION ( 'NONE',  ( 0.000000000000000000, -4.122115190439938353E-15, -1.000000000000000000 ) ) ;
#402 = CARTESIAN_POINT ( 'NONE',  ( -363.0000000000000000, -135.0000000000000000, 114.0000000000000000 ) ) ;
#403 = DIRECTION ( 'NONE',  ( 0.000000000000000000, 0.000000000000000000, 1.000000000000000000 ) ) ;
#404 = VERTEX_POINT ( 'NONE', #32954 ) ;
#405 = CARTESIAN_POINT ( 'NONE',  ( 2.789999999999999147, -2.530647759431309929, -30.33427519320597199 ) ) ;
#406 = VECTOR ( 'NONE', #1614, 1000.000000000000000 ) ;
#407 = DIRECTION ( 'NONE',  ( 0.000000000000000000, 6.123233995736766036E-17, 1.000000000000000000 ) ) ;
#409 = CARTESIAN_POINT ( 'NONE',  ( -2.216215597024039141, -32.46987467335852529, 68.31122994652405112 ) ) ;
#408 = FACE_OUTER_BOUND ( 'NONE', #18168, .T. ) ;
#410 = AXIS2_PLACEMENT_3D ( 'NONE', #353, #702, #3357 ) ;
#411 = CARTESIAN_POINT ( 'NONE',  ( -20.00000000000004619, -124.9999999999999432, -194.9999999999999432 ) ) ;
#412 = ORIENTED_EDGE ( 'NONE', *, *, #6672, .F. ) ;
#413 = DIRECTION ( 'NONE',  ( 1.000000000000000000, -0.000000000000000000, 0.000000000000000000 ) ) ;
#414 = FACE_OUTER_BOUND ( 'NONE', #24829, .T. ) ;
#415 = EDGE_CURVE ( 'NONE', #2863, #31849, #8577, .T. ) ;
#416 = ORIENTED_EDGE ( 'NONE', *, *, #6218, .F. ) ;
#417 = EDGE_CURVE ( 'NONE', #26117, #20828, #25120, .T. ) ;
#418 = EDGE_CURVE ( 'NONE', #32157, #25965, #6244, .T. ) ;
#419 = VECTOR ( 'NONE', #14183, 1000.000000000000000 ) ;
#420 = ORIENTED_EDGE ( 'NONE', *, *, #12622, .F. ) ;
#421 = ORIENTED_EDGE ( 'NONE', *, *, #373, .F. ) ;
#422 = DIRECTION ( 'NONE',  ( -1.000000000000000000, -0.000000000000000000, -0.000000000000000000 ) ) ;
#423 = VERTEX_POINT ( 'NONE', #6428 ) ;
#424 = ORIENTED_EDGE ( 'NONE', *, *, #23285, .T. ) ;
#425 = CARTESIAN_POINT ( 'NONE',  ( -18.45373714011839539, 26.80790850550480897, 68.31122994652405112 ) ) ;
#426 = EDGE_CURVE ( 'NONE', #7666, #28875, #25652, .T. ) ;
#427 = CIRCLE ( 'NONE', #22026, 10.00000000000000000 ) ;
#428 = VECTOR ( 'NONE', #33661, 1000.000000000000000 ) ;
#429 = CARTESIAN_POINT ( 'NONE',  ( -418.0000000000000000, 124.9999999999999432, -162.9999999999999716 ) ) ;
#430 = PLANE ( 'NONE',  #10872 ) ;
#431 = ORIENTED_EDGE ( 'NONE', *, *, #25232, .F. ) ;
#432 = ORIENTED_EDGE ( 'NONE', *, *, #20397, .F. ) ;
#433 = LINE ( 'NONE', #254, #17985 ) ;
#434 = DIRECTION ( 'NONE',  ( 0.000000000000000000, 1.836970198721029441E-16, -1.000000000000000000 ) ) ;
#435 = EDGE_CURVE ( 'NONE', #18500, #31492, #4843, .T. ) ;
#436 = DIRECTION ( 'NONE',  ( -1.000000000000000000, 0.000000000000000000, 0.000000000000000000 ) ) ;
#437 = CARTESIAN_POINT ( 'NONE',  ( -4.850000000000000533, 0.000000000000000000, 3.180000000000000160 ) ) ;
#438 = ORIENTED_EDGE ( 'NONE', *, *, #25737, .T. ) ;
#439 = VECTOR ( 'NONE', #21313, 1000.000000000000000 ) ;
#440 = EDGE_CURVE ( 'NONE', #10023, #18562, #30296, .T. ) ;
#441 = DIRECTION ( 'NONE',  ( -1.000000000000000000, -0.000000000000000000, -0.000000000000000000 ) ) ;
#442 = EDGE_CURVE ( 'NONE', #2071, #22576, #14652, .T. ) ;
#443 = DIRECTION ( 'NONE',  ( -0.000000000000000000, 1.000000000000000000, -0.000000000000000000 ) ) ;
#444 = ORIENTED_EDGE ( 'NONE', *, *, #6797, .F. ) ;
#445 = DIRECTION ( 'NONE',  ( 1.000000000000000000, 0.000000000000000000, 0.000000000000000000 ) ) ;
#446 = EDGE_CURVE ( 'NONE', #17949, #8883, #28157, .T. ) ;
#447 = CARTESIAN_POINT ( 'NONE',  ( 0.006892415499590480790, 4.187058600949983500, -30.58452291340886831 ) ) ;
#448 = CARTESIAN_POINT ( 'NONE',  ( 2.719010669804482916, -30.32061017160040350, -9.230676164042293408 ) ) ;
#449 = DIRECTION ( 'NONE',  ( 0.4198891015602635446, -0.9075754196709575616, -1.667188999027280528E-16 ) ) ;
#450 = ORIENTED_EDGE ( 'NONE', *, *, #30527, .F. ) ;
#451 = AXIS2_PLACEMENT_3D ( 'NONE', #17742, #12395, #1529 ) ;
#452 = FACE_OUTER_BOUND ( 'NONE', #26260, .T. ) ;
#453 = ORIENTED_EDGE ( 'NONE', *, *, #7812, .T. ) ;
#454 = PLANE ( 'NONE',  #18923 ) ;
#455 = CIRCLE ( 'NONE', #12411, 2.524999999999999467 ) ;
#456 = AXIS2_PLACEMENT_3D ( 'NONE', #31514, #16040, #10517 ) ;
#457 = ORIENTED_EDGE ( 'NONE', *, *, #17828, .T. ) ;
#458 = EDGE_CURVE ( 'NONE', #20784, #34333, #22819, .T. ) ;
#459 = ADVANCED_FACE ( 'NONE', ( #16977 ), #27625, .T. ) ;
#460 = DIRECTION ( 'NONE',  ( -1.000000000000000000, 0.000000000000000000, -1.300283923313630633E-47 ) ) ;
#461 = DIRECTION ( 'NONE',  ( -1.000000000000000000, 0.000000000000000000, 0.000000000000000000 ) ) ;
#462 = EDGE_LOOP ( 'NONE', ( #2821, #4541, #31445, #15602, #5501, #28046 ) ) ;
#463 = ORIENTED_EDGE ( 'NONE', *, *, #15359, .T. ) ;
#464 = AXIS2_PLACEMENT_3D ( 'NONE', #20405, #28583, #17576 ) ;
#465 = ORIENTED_EDGE ( 'NONE', *, *, #4049, .T. ) ;
#466 = CARTESIAN_POINT ( 'NONE',  ( -0.2989565185775304723, 0.000000000000000000, 0.000000000000000000 ) ) ;
#467 = CARTESIAN_POINT ( 'NONE',  ( -145.0000000000000568, -87.50000000000000000, 65.00000000000000000 ) ) ;
#468 = ORIENTED_EDGE ( 'NONE', *, *, #12591, .T. ) ;
#469 = VERTEX_POINT ( 'NONE', #17506 ) ;
#470 = CARTESIAN_POINT ( 'NONE',  ( -445.9999999999999432, 105.0000000000000000, -77.99999999999997158 ) ) ;
#471 = CARTESIAN_POINT ( 'NONE',  ( 2.783107615394383672, -17.88431215799149143, 25.16139613958896604 ) ) ;
#472 = CARTESIAN_POINT ( 'NONE',  ( -5.781867695661277118, -1.866624223957557893, -0.7500000000000000000 ) ) ;
#473 = CARTESIAN_POINT ( 'NONE',  ( -499.9999999999999432, 112.9999999999999574, -159.0000000000000000 ) ) ;
#474 = VERTEX_POINT ( 'NONE', #30482 ) ;
#475 = ORIENTED_EDGE ( 'NONE', *, *, #20470, .F. ) ;
#476 = CYLINDRICAL_SURFACE ( 'NONE', #3727, 7.999999999999979572 ) ;
#477 = DIRECTION ( 'NONE',  ( 0.000000000000000000, 0.000000000000000000, 1.000000000000000000 ) ) ;
#478 = CARTESIAN_POINT ( 'NONE',  ( 145.0000000000000568, -90.29102463692674974, -73.95413108702814498 ) ) ;
#479 = PLANE ( 'NONE',  #16043 ) ;
#480 = EDGE_CURVE ( 'NONE', #32964, #14283, #33981, .T. ) ;
#481 = VECTOR ( 'NONE', #14446, 1000.000000000000000 ) ;
#482 = EDGE_CURVE ( 'NONE', #12038, #33286, #10560, .T. ) ;
#483 = CARTESIAN_POINT ( 'NONE',  ( 0.7564103440795023614, 14.91861104533797899, -30.45815716957487496 ) ) ;
#484 = DIRECTION ( 'NONE',  ( -1.000000000000000000, 0.000000000000000000, 0.000000000000000000 ) ) ;
#486 = AXIS2_PLACEMENT_3D ( 'NONE', #4593, #26151, #10139 ) ;
#485 = DIRECTION ( 'NONE',  ( -1.000000000000000000, 0.000000000000000000, -0.000000000000000000 ) ) ;
#487 = ORIENTED_EDGE ( 'NONE', *, *, #9637, .F. ) ;
#488 = CARTESIAN_POINT ( 'NONE',  ( -32.54223829851967764, 0.4550817492056100644, 68.31122994652405112 ) ) ;
#489 = ADVANCED_FACE ( 'NONE', ( #1969 ), #7124, .F. ) ;
#490 = CARTESIAN_POINT ( 'NONE',  ( -414.0000000000000568, 105.0000000000000000, 132.0000000000000000 ) ) ;
#491 = CIRCLE ( 'NONE', #22653, 2.524999999999999467 ) ;
#492 = DIRECTION ( 'NONE',  ( -1.000000000000000000, -0.000000000000000000, -0.000000000000000000 ) ) ;
#493 = VERTEX_POINT ( 'NONE', #26528 ) ;
#494 = EDGE_CURVE ( 'NONE', #32940, #29402, #33851, .T. ) ;
#495 = DIRECTION ( 'NONE',  ( 0.000000000000000000, 2.309213040847544338E-50, 1.000000000000000000 ) ) ;
#496 = EDGE_LOOP ( 'NONE', ( #8671, #8496, #20597, #12284 ) ) ;
#497 = DIRECTION ( 'NONE',  ( -5.546364386991661285E-52, 0.000000000000000000, -1.000000000000000000 ) ) ;
#498 = CARTESIAN_POINT ( 'NONE',  ( -100.0512976970618269, 1.336696757081942799, 12.43272095415539624 ) ) ;
#499 = VECTOR ( 'NONE', #8880, 1000.000000000000000 ) ;
#500 = TOROIDAL_SURFACE ( 'NONE', #9599, 30.47050528711512030, 8.000000000000000000 ) ;
#501 = VERTEX_POINT ( 'NONE', #14993 ) ;
#502 = DIRECTION ( 'NONE',  ( 1.000000000000000000, 0.000000000000000000, -1.232595164407831220E-32 ) ) ;
#503 = PLANE ( 'NONE',  #5402 ) ;
#504 = PLANE ( 'NONE',  #30798 ) ;
#505 = ORIENTED_EDGE ( 'NONE', *, *, #3408, .T. ) ;
#506 = CARTESIAN_POINT ( 'NONE',  ( 825.6804718436084158, 1267.802569466347677, 1753.598338701304101 ) ) ;
#507 = CARTESIAN_POINT ( 'NONE',  ( 0.5248942543850775300, -33.37077467988373769, 0.7759739055973007282 ) ) ;
#508 = EDGE_CURVE ( 'NONE', #6161, #17092, #29208, .T. ) ;
#509 = VERTEX_POINT ( 'NONE', #1793 ) ;
#510 = FACE_OUTER_BOUND ( 'NONE', #7829, .T. ) ;
#511 = AXIS2_PLACEMENT_3D ( 'NONE', #21319, #32167, #30028 ) ;
#512 = LINE ( 'NONE', #33420, #24339 ) ;
#513 = CARTESIAN_POINT ( 'NONE',  ( 2.719010673315533477, 14.74869129583236216, -28.05389252521634802 ) ) ;
#514 = CARTESIAN_POINT ( 'NONE',  ( 110.5348319305551996, -1.563330414527343892, 7.345474502415979323 ) ) ;
#515 = ITEM_DEFINED_TRANSFORMATION ( 'NONE', 'NONE', #29751,  #28566 ) ;
#516 = ORIENTED_EDGE ( 'NONE', *, *, #603, .F. ) ;
#517 = ORIENTED_EDGE ( 'NONE', *, *, #32290, .F. ) ;
#518 = ORIENTED_EDGE ( 'NONE', *, *, #18226, .F. ) ;
#519 = DIRECTION ( 'NONE',  ( 0.000000000000000000, 1.131431318426415506E-52, 1.000000000000000000 ) ) ;
#520 = ADVANCED_FACE ( 'NONE', ( #26170 ), #21018, .T. ) ;
#521 = CARTESIAN_POINT ( 'NONE',  ( -20.00000000000007461, 112.9999999999999574, 162.9999999999999716 ) ) ;
#522 = EDGE_CURVE ( 'NONE', #24257, #22309, #20328, .T. ) ;
#523 = ADVANCED_FACE ( 'NONE', ( #31345 ), #4279, .F. ) ;
#524 = DIRECTION ( 'NONE',  ( -1.000000000000000000, 0.000000000000000000, 0.000000000000000000 ) ) ;
#525 = CIRCLE ( 'NONE', #16796, 7.999999999999979572 ) ;
#526 = ORIENTED_EDGE ( 'NONE', *, *, #22218, .F. ) ;
#527 = VERTEX_POINT ( 'NONE', #12669 ) ;
#528 = LINE ( 'NONE', #11379, #25963 ) ;
#529 = ORIENTED_EDGE ( 'NONE', *, *, #33922, .T. ) ;
#530 = CYLINDRICAL_SURFACE ( 'NONE', #3882, 4.000000000000003553 ) ;
#531 = CYLINDRICAL_SURFACE ( 'NONE', #29653, 7.999999999999979572 ) ;
#532 = ORIENTED_EDGE ( 'NONE', *, *, #11905, .T. ) ;
#533 = VECTOR ( 'NONE', #26637, 1000.000000000000000 ) ;
#534 = ORIENTED_EDGE ( 'NONE', *, *, #6126, .F. ) ;
#535 = DIRECTION ( 'NONE',  ( -1.000000000000000000, 0.000000000000000000, 0.000000000000000000 ) ) ;
#536 = DIRECTION ( 'NONE',  ( 1.000000000000000000, -0.000000000000000000, -0.000000000000000000 ) ) ;
#537 = ORIENTED_EDGE ( 'NONE', *, *, #19901, .F. ) ;
#538 = CARTESIAN_POINT ( 'NONE',  ( -10.84269519964070305, -36.27449394610876965, -36.68877005347593467 ) ) ;
#539 = CARTESIAN_POINT ( 'NONE',  ( 14.14940496480368104, 33.69708579775584667, -36.68877005347592757 ) ) ;
#540 = PLANE ( 'NONE',  #20688 ) ;
#541 = AXIS2_PLACEMENT_3D ( 'NONE', #20921, #31768, #29104 ) ;
#542 = CARTESIAN_POINT ( 'NONE',  ( -499.9999999999999432, -113.0000000000000000, -162.9999999999999716 ) ) ;
#543 = LINE ( 'NONE', #35085, #19991 ) ;
#544 = CARTESIAN_POINT ( 'NONE',  ( -9.144464960067640646, -31.23432620483743705, -36.68877005347593467 ) ) ;
#545 = ORIENTED_EDGE ( 'NONE', *, *, #1677, .T. ) ;
#546 = DIRECTION ( 'NONE',  ( 2.631201909438060269E-14, -5.396010391056495992E-16, 0.9999999999999998890 ) ) ;
#547 = APPLICATION_CONTEXT ( 'automotive_design' ) ;
#548 = ORIENTED_EDGE ( 'NONE', *, *, #30977, .T. ) ;
#549 = VERTEX_POINT ( 'NONE', #28849 ) ;
#550 = DIRECTION ( 'NONE',  ( -1.000000000000000000, 0.000000000000000000, 0.000000000000000000 ) ) ;
#551 = CARTESIAN_POINT ( 'NONE',  ( 103.6426013227723928, 5.578557642680240569, 5.013303406467239931 ) ) ;
#552 = PRODUCT_CONTEXT ( 'NONE', #11461, 'mechanical' ) ;
#553 = EDGE_CURVE ( 'NONE', #7666, #18883, #20841, .T. ) ;
#554 = ORIENTED_EDGE ( 'NONE', *, *, #3009, .T. ) ;
#555 = DIRECTION ( 'NONE',  ( 0.000000000000000000, 1.000000000000000000, 5.145227585319922065E-49 ) ) ;
#556 = CARTESIAN_POINT ( 'NONE',  ( -104.3188479752188869, -5.080615126163384510, -11.42114788619746868 ) ) ;
#557 = EDGE_CURVE ( 'NONE', #31368, #17595, #13969, .T. ) ;
#558 = AXIS2_PLACEMENT_3D ( 'NONE', #28352, #26018, #20687 ) ;
#559 = EDGE_CURVE ( 'NONE', #10218, #5077, #21246, .T. ) ;
#561 = CARTESIAN_POINT ( 'NONE',  ( -410.0000000000000568, 104.9999999999999858, -175.0000000000000000 ) ) ;
#560 = FACE_OUTER_BOUND ( 'NONE', #15965, .T. ) ;
#562 = EDGE_LOOP ( 'NONE', ( #7226, #23075, #30348, #6330 ) ) ;
#563 = ORIENTED_EDGE ( 'NONE', *, *, #30172, .T. ) ;
#564 = CARTESIAN_POINT ( 'NONE',  ( -499.9999999999999432, 136.9999999999999432, -155.0000000000000000 ) ) ;
#565 = EDGE_CURVE ( 'NONE', #34117, #30722, #12848, .T. ) ;
#566 = LINE ( 'NONE', #21926, #17059 ) ;
#567 = DIRECTION ( 'NONE',  ( 1.000000000000000000, 0.000000000000000000, 0.000000000000000000 ) ) ;
#568 = DIRECTION ( 'NONE',  ( 0.000000000000000000, -1.000000000000000000, 0.000000000000000000 ) ) ;
#569 = ORIENTED_EDGE ( 'NONE', *, *, #971, .T. ) ;
#570 = CARTESIAN_POINT ( 'NONE',  ( 0.000000000000000000, -20.35927063852824048, 24.61013060777164796 ) ) ;
#571 = DIRECTION ( 'NONE',  ( 1.000000000000000000, 0.000000000000000000, -1.848892746611746966E-32 ) ) ;
#572 = PLANE ( 'NONE',  #2099 ) ;
#573 = ORIENTED_EDGE ( 'NONE', *, *, #23821, .T. ) ;
#574 = LINE ( 'NONE', #16262, #35090 ) ;
#575 = CARTESIAN_POINT ( 'NONE',  ( -418.0000000000000000, -145.0000000000000000, -175.0000000000000000 ) ) ;
#576 = EDGE_CURVE ( 'NONE', #19034, #23318, #12495, .T. ) ;
#577 = CARTESIAN_POINT ( 'NONE',  ( -499.9999999999999432, 136.9999999999999432, -190.9999999999999716 ) ) ;
#579 = DIRECTION ( 'NONE',  ( -1.000000000000000000, -0.000000000000000000, -0.000000000000000000 ) ) ;
#578 = DIRECTION ( 'NONE',  ( 0.000000000000000000, 0.000000000000000000, 1.000000000000000000 ) ) ;
#580 = DIRECTION ( 'NONE',  ( 0.000000000000000000, 1.000000000000000000, 5.145227585319922065E-49 ) ) ;
#581 = ORIENTED_EDGE ( 'NONE', *, *, #14404, .F. ) ;
#582 = DIRECTION ( 'NONE',  ( 0.000000000000000000, 1.310824597558155437E-49, 1.000000000000000000 ) ) ;
#583 = DIRECTION ( 'NONE',  ( -1.000000000000000000, -0.000000000000000000, -0.000000000000000000 ) ) ;
#584 = VECTOR ( 'NONE', #33294, 1000.000000000000000 ) ;
#585 = ORIENTED_EDGE ( 'NONE', *, *, #9500, .F. ) ;
#586 = ORIENTED_EDGE ( 'NONE', *, *, #10577, .T. ) ;
#587 =( REPRESENTATION_RELATIONSHIP ('NONE','NONE', #23037, #28231 ) REPRESENTATION_RELATIONSHIP_WITH_TRANSFORMATION ( #22450 )SHAPE_REPRESENTATION_RELATIONSHIP( ) );
#588 = ORIENTED_EDGE ( 'NONE', *, *, #13917, .F. ) ;
#589 = CARTESIAN_POINT ( 'NONE',  ( 2.789999999999999591, -3.625355760179855835, 30.44651458975030067 ) ) ;
#590 = EDGE_LOOP ( 'NONE', ( #5300, #9615, #21290, #22102 ) ) ;
#591 = VERTEX_POINT ( 'NONE', #18194 ) ;
#592 = LINE ( 'NONE', #30312, #24116 ) ;
#593 = EDGE_CURVE ( 'NONE', #33757, #32360, #20496, .T. ) ;
#594 = VERTEX_POINT ( 'NONE', #20673 ) ;
#595 = CARTESIAN_POINT ( 'NONE',  ( 0.000000000000000000, -25.77598557799239742, -16.24962337825829195 ) ) ;
#596 = LINE ( 'NONE', #19835, #27348 ) ;
#597 = ORIENTED_EDGE ( 'NONE', *, *, #21069, .F. ) ;
#598 = ORIENTED_EDGE ( 'NONE', *, *, #14200, .F. ) ;
#599 = FACE_OUTER_BOUND ( 'NONE', #6843, .T. ) ;
#601 = LINE ( 'NONE', #17003, #7250 ) ;
#600 = AXIS2_PLACEMENT_3D ( 'NONE', #10978, #16688, #29670 ) ;
#602 = ADVANCED_FACE ( 'NONE', ( #4451 ), #23172, .T. ) ;
#603 = EDGE_CURVE ( 'NONE', #26714, #17291, #15511, .T. ) ;
#604 = CARTESIAN_POINT ( 'NONE',  ( 100.0399502288726268, -2.891119662789794820, -12.16223328578254481 ) ) ;
#605 = CARTESIAN_POINT ( 'NONE',  ( 2.261199747851626807, 5.497007441955480189, -32.93420861807575051 ) ) ;
#606 = DIRECTION ( 'NONE',  ( -0.000000000000000000, 1.000000000000000000, -0.000000000000000000 ) ) ;
#607 = ORIENTED_EDGE ( 'NONE', *, *, #23373, .T. ) ;
#608 = AXIS2_PLACEMENT_3D ( 'NONE', #24658, #22008, #32850 ) ;
#609 = DIRECTION ( 'NONE',  ( -0.000000000000000000, 1.836970198721029934E-16, -1.000000000000000000 ) ) ;
#610 = EDGE_CURVE ( 'NONE', #19346, #10620, #34542, .T. ) ;
#611 = ADVANCED_FACE ( 'NONE', ( #2493 ), #8368, .F. ) ;
#612 = CARTESIAN_POINT ( 'NONE',  ( 1.040000000000003810, -2.430610048905784915, -34.32897884578301984 ) ) ;
#613 = EDGE_LOOP ( 'NONE', ( #32797, #28941 ) ) ;
#614 = PLANE ( 'NONE',  #25375 ) ;
#615 = CARTESIAN_POINT ( 'NONE',  ( 1.040000000000000258, 28.00026196654270905, 20.00929742917132614 ) ) ;
#616 = LINE ( 'NONE', #2922, #2449 ) ;
#617 = CARTESIAN_POINT ( 'NONE',  ( 0.02407890056655825201, -23.70329957282570632, -20.11932597908854703 ) ) ;
#618 = CARTESIAN_POINT ( 'NONE',  ( 15.99999999999998579, 4.559999999999908127, -172.9900000000000091 ) ) ;
#619 = AXIS2_PLACEMENT_3D ( 'NONE', #1312, #12183, #23029 ) ;
#620 = CIRCLE ( 'NONE', #9710, 13.49999999999999822 ) ;
#621 = LINE ( 'NONE', #27139, #28055 ) ;
#623 = ORIENTED_EDGE ( 'NONE', *, *, #12621, .T. ) ;
#622 =( GEOMETRIC_REPRESENTATION_CONTEXT ( 3 ) GLOBAL_UNCERTAINTY_ASSIGNED_CONTEXT ( ( #6076 ) ) GLOBAL_UNIT_ASSIGNED_CONTEXT ( ( #14562, #33576, #1191 ) ) REPRESENTATION_CONTEXT ( 'NONE', 'WORKASPACE' ) );
#625 = DIRECTION ( 'NONE',  ( -1.000000000000000000, -0.000000000000000000, -0.000000000000000000 ) ) ;
#624 = LINE ( 'NONE', #9159, #6292 ) ;
#626 = EDGE_CURVE ( 'NONE', #20682, #8601, #10335, .T. ) ;
#627 = ORIENTED_EDGE ( 'NONE', *, *, #29512, .F. ) ;
#628 = CYLINDRICAL_SURFACE ( 'NONE', #33668, 34.41491905851385269 ) ;
#629 = CARTESIAN_POINT ( 'NONE',  ( 12.00000000000001066, -134.9999999999999716, 194.9999999999999716 ) ) ;
#630 = AXIS2_PLACEMENT_3D ( 'NONE', #7025, #15243, #23764 ) ;
#631 = EDGE_LOOP ( 'NONE', ( #17739, #3820, #7539, #1701 ) ) ;
#632 = AXIS2_PLACEMENT_3D ( 'NONE', #14720, #8823, #19878 ) ;
#633 = EDGE_LOOP ( 'NONE', ( #9077, #27367, #24881, #22906, #2998 ) ) ;
#634 = EDGE_CURVE ( 'NONE', #13940, #4555, #21191, .T. ) ;
#635 = EDGE_CURVE ( 'NONE', #21072, #3784, #32561, .T. ) ;
#636 = ORIENTED_EDGE ( 'NONE', *, *, #31314, .F. ) ;
#637 = DIRECTION ( 'NONE',  ( -1.000000000000000000, -0.000000000000000000, -0.000000000000000000 ) ) ;
#638 = CARTESIAN_POINT ( 'NONE',  ( 2.789999999999999147, -21.75986515490462736, -21.28569233123117144 ) ) ;
#639 = VERTEX_POINT ( 'NONE', #21379 ) ;
#640 = VERTEX_POINT ( 'NONE', #13541 ) ;
#641 = DIRECTION ( 'NONE',  ( -0.000000000000000000, 1.836970198721029934E-16, -1.000000000000000000 ) ) ;
#642 = FACE_OUTER_BOUND ( 'NONE', #3782, .T. ) ;
#643 = CARTESIAN_POINT ( 'NONE',  ( 11.99999999999995559, -145.0000000000000000, 194.9999999999999716 ) ) ;
#644 = AXIS2_PLACEMENT_3D ( 'NONE', #32551, #30604, #176 ) ;
#645 = CARTESIAN_POINT ( 'NONE',  ( -4.087654984470516816E-16, 27.73515059361837842, -12.87176213890998433 ) ) ;
#646 = ORIENTED_EDGE ( 'NONE', *, *, #2039, .T. ) ;
#647 = ORIENTED_EDGE ( 'NONE', *, *, #9770, .F. ) ;
#648 = CARTESIAN_POINT ( 'NONE',  ( 99.26191511054632599, 0.000000000000000000, 60.00000000000000000 ) ) ;
#649 = FACE_OUTER_BOUND ( 'NONE', #15663, .T. ) ;
#650 = VECTOR ( 'NONE', #5944, 1000.000000000000000 ) ;
#651=STYLED_ITEM('',(#35254),#22717);
#652 = LINE ( 'NONE', #11513, #1580 ) ;
#653 = LINE ( 'NONE', #18869, #7882 ) ;
#654 = CARTESIAN_POINT ( 'NONE',  ( -70.00000000000000000, 75.55999999999990280, -172.9900000000000091 ) ) ;
#655 = LINE ( 'NONE', #13651, #10552 ) ;
#656 = ADVANCED_FACE ( 'NONE', ( #2312 ), #27058, .F. ) ;
#657 = EDGE_CURVE ( 'NONE', #30105, #32001, #24381, .T. ) ;
#658 = CARTESIAN_POINT ( 'NONE',  ( 12.00000000000001066, 134.9999999999999432, -154.9999999999999716 ) ) ;
#659 = ORIENTED_EDGE ( 'NONE', *, *, #951, .T. ) ;
#660 = VECTOR ( 'NONE', #33698, 1000.000000000000000 ) ;
#661 = LINE ( 'NONE', #835, #20287 ) ;
#662 = DIRECTION ( 'NONE',  ( 0.000000000000000000, 1.000000000000000000, 0.000000000000000000 ) ) ;
#663 = AXIS2_PLACEMENT_3D ( 'NONE', #15533, #26376, #17867 ) ;
#664 = LINE ( 'NONE', #5982, #1831 ) ;
#665 = ORIENTED_EDGE ( 'NONE', *, *, #8099, .F. ) ;
#666 = FACE_OUTER_BOUND ( 'NONE', #16803, .T. ) ;
#667 = ORIENTED_EDGE ( 'NONE', *, *, #12403, .T. ) ;
#668 = DIRECTION ( 'NONE',  ( 0.000000000000000000, 0.000000000000000000, -1.000000000000000000 ) ) ;
#669 = DIRECTION ( 'NONE',  ( -1.000000000000000000, 0.000000000000000000, 0.000000000000000000 ) ) ;
#670 = EDGE_CURVE ( 'NONE', #3150, #31908, #29334, .T. ) ;
#672 = ORIENTED_EDGE ( 'NONE', *, *, #22907, .F. ) ;
#671 = AXIS2_PLACEMENT_3D ( 'NONE', #19191, #13656, #30199 ) ;
#673 = AXIS2_PLACEMENT_3D ( 'NONE', #16710, #32352, #5290 ) ;
#674 = CARTESIAN_POINT ( 'NONE',  ( 1.749999999999999778, 14.89726405156217126, 31.02351007835983054 ) ) ;
#675 = VECTOR ( 'NONE', #22343, 1000.000000000000114 ) ;
#676 = CARTESIAN_POINT ( 'NONE',  ( 55.00000000000000711, 9.122700168548420677E-16, -6.898500000000000298 ) ) ;
#677 = LINE ( 'NONE', #11000, #15466 ) ;
#678 = CIRCLE ( 'NONE', #20570, 3.999999999999976019 ) ;
#679 = EDGE_CURVE ( 'NONE', #33018, #4776, #8184, .T. ) ;
#680 = ORIENTED_EDGE ( 'NONE', *, *, #6279, .T. ) ;
#681 = EDGE_CURVE ( 'NONE', #1567, #23446, #30476, .T. ) ;
#682 = EDGE_CURVE ( 'NONE', #30822, #12038, #929, .T. ) ;
#683 = DIRECTION ( 'NONE',  ( 2.631201909438060585E-14, -5.396010391056496978E-16, 1.000000000000000000 ) ) ;
#684 = DIRECTION ( 'NONE',  ( -1.000000000000000000, -0.000000000000000000, -0.000000000000000000 ) ) ;
#685 = ORIENTED_EDGE ( 'NONE', *, *, #27268, .F. ) ;
#686 = CARTESIAN_POINT ( 'NONE',  ( 0.02407890056655695096, -23.70329957282599764, 20.11932597908820242 ) ) ;
#687 = EDGE_CURVE ( 'NONE', #28835, #181, #8010, .T. ) ;
#688 = VECTOR ( 'NONE', #24666, 1000.000000000000000 ) ;
#689 = LINE ( 'NONE', #22397, #22097 ) ;
#690 = DIRECTION ( 'NONE',  ( -1.000000000000000000, 8.433758354584418579E-81, -1.232595164407830946E-32 ) ) ;
#691 = DIRECTION ( 'NONE',  ( -1.000000000000000000, -0.000000000000000000, -0.000000000000000000 ) ) ;
#692 = ORIENTED_EDGE ( 'NONE', *, *, #2681, .F. ) ;
#693 = VERTEX_POINT ( 'NONE', #5676 ) ;
#694 = ORIENTED_EDGE ( 'NONE', *, *, #22904, .F. ) ;
#695 = PRODUCT ( 'frame_Default<As Machined>', 'frame_Default<As Machined>', '', ( #11065 ) ) ;
#696 = FACE_OUTER_BOUND ( 'NONE', #25279, .T. ) ;
#697 = CIRCLE ( 'NONE', #1800, 4.750000000000004441 ) ;
#698 = CARTESIAN_POINT ( 'NONE',  ( 2.765921099433441999, -23.70329957282570632, -20.11932597908854703 ) ) ;
#700 = ORIENTED_EDGE ( 'NONE', *, *, #24646, .F. ) ;
#699 = AXIS2_PLACEMENT_3D ( 'NONE', #32555, #29554, #17888 ) ;
#701 = VERTEX_POINT ( 'NONE', #5505 ) ;
#702 = DIRECTION ( 'NONE',  ( -0.000000000000000000, 1.836970198721029934E-16, -1.000000000000000000 ) ) ;
#703 = AXIS2_PLACEMENT_3D ( 'NONE', #2442, #2103, #14812 ) ;
#704 = ORIENTED_EDGE ( 'NONE', *, *, #7401, .F. ) ;
#705 = DIRECTION ( 'NONE',  ( 0.000000000000000000, 0.000000000000000000, 1.000000000000000000 ) ) ;
#706 = CARTESIAN_POINT ( 'NONE',  ( 0.02407890056655868569, 24.20451283648829133, 19.51346322004938827 ) ) ;
#707 = VERTEX_POINT ( 'NONE', #16225 ) ;
#708 = EDGE_LOOP ( 'NONE', ( #10396, #12384, #6662, #7529 ) ) ;
#709 =( NAMED_UNIT ( * ) PLANE_ANGLE_UNIT ( ) SI_UNIT ( $, .RADIAN. ) );
#710 = LINE ( 'NONE', #3191, #33103 ) ;
#711 = ORIENTED_EDGE ( 'NONE', *, *, #4540, .T. ) ;
#712 = DIRECTION ( 'NONE',  ( -0.000000000000000000, 1.836970198721029688E-16, -1.000000000000000000 ) ) ;
#713 = FACE_OUTER_BOUND ( 'NONE', #31703, .T. ) ;
#714 = CARTESIAN_POINT ( 'NONE',  ( -500.0000000000000000, -113.0000000000000000, 194.9999999999999716 ) ) ;
#715 = CARTESIAN_POINT ( 'NONE',  ( -105.3381247832323027, -5.114954807106461665, 11.40557921924218832 ) ) ;
#716 = LINE ( 'NONE', #33098, #30982 ) ;
#717 = SURFACE_STYLE_USAGE ( .BOTH. , #27762 ) ;
#718 = ORIENTED_EDGE ( 'NONE', *, *, #26278, .T. ) ;
#719 = EDGE_CURVE ( 'NONE', #25735, #29292, #10014, .T. ) ;
#720 = CIRCLE ( 'NONE', #7507, 7.500000000000000000 ) ;
#721 = EDGE_CURVE ( 'NONE', #11831, #17160, #30086, .T. ) ;
#722 = ORIENTED_EDGE ( 'NONE', *, *, #5518, .F. ) ;
#723 = VECTOR ( 'NONE', #4056, 1000.000000000000000 ) ;
#724 = DIRECTION ( 'NONE',  ( 0.1063910735368947813, -0.9943243633099144718, -3.335902418024520312E-15 ) ) ;
#725 = AXIS2_PLACEMENT_3D ( 'NONE', #32125, #31776, #7740 ) ;
#726 = VERTEX_POINT ( 'NONE', #16403 ) ;
#727 = ORIENTED_EDGE ( 'NONE', *, *, #801, .T. ) ;
#728 = DIRECTION ( 'NONE',  ( 0.000000000000000000, 1.000000000000000000, 0.000000000000000000 ) ) ;
#729 = CARTESIAN_POINT ( 'NONE',  ( 104.6074685613258168, 5.728031835420551943, 4.841551550731546527 ) ) ;
#730 = SHAPE_DEFINITION_REPRESENTATION ( #21995, #18474 ) ;
#731 = VERTEX_POINT ( 'NONE', #27233 ) ;
#732 = CARTESIAN_POINT ( 'NONE',  ( 3.985664461616345376E-15, 32.54542015209057837, -87.50000000000000000 ) ) ;
#733 = CARTESIAN_POINT ( 'NONE',  ( -108.7324602969096645, -3.501388609494501036, -12.00022069954820836 ) ) ;
#735 = CARTESIAN_POINT ( 'NONE',  ( -500.0000000000000000, -137.0000000000000000, 159.0000000000000000 ) ) ;
#734 = CARTESIAN_POINT ( 'NONE',  ( -500.0000000000000000, -137.0000000000000000, 187.0000000000000000 ) ) ;
#736 = VERTEX_POINT ( 'NONE', #13710 ) ;
#737 = ORIENTED_EDGE ( 'NONE', *, *, #1707, .T. ) ;
#738 = DIRECTION ( 'NONE',  ( -0.8568571761675883858, 0.5155538571770231782, 9.470570714698694973E-17 ) ) ;
#739 = DIRECTION ( 'NONE',  ( 1.000000000000000000, 0.000000000000000000, 0.000000000000000000 ) ) ;
#740 = CARTESIAN_POINT ( 'NONE',  ( -8.499999999999998224, 0.000000000000000000, 5.429999999999999716 ) ) ;
#741 = FACE_OUTER_BOUND ( 'NONE', #26082, .T. ) ;
#742 = EDGE_LOOP ( 'NONE', ( #25177, #23804, #31066, #16632 ) ) ;
#743 = AXIS2_PLACEMENT_3D ( 'NONE', #19776, #22084, #19423 ) ;
#744 = DIRECTION ( 'NONE',  ( 1.000000000000000000, 0.000000000000000000, 0.000000000000000000 ) ) ;
#745 = CYLINDRICAL_SURFACE ( 'NONE', #8305, 7.999999999999979572 ) ;
#746 = DIRECTION ( 'NONE',  ( -1.000000000000000000, 0.000000000000000000, -1.300283923313630633E-47 ) ) ;
#747 = AXIS2_PLACEMENT_3D ( 'NONE', #33040, #30386, #5986 ) ;
#748 = AXIS2_PLACEMENT_3D ( 'NONE', #8542, #14074, #33456 ) ;
#749 = VECTOR ( 'NONE', #31002, 1000.000000000000000 ) ;
#750 = VERTEX_POINT ( 'NONE', #16577 ) ;
#751 = CARTESIAN_POINT ( 'NONE',  ( 143.0000000000000568, -167.8552739801376390, -46.75049602362128809 ) ) ;
#752 = CARTESIAN_POINT ( 'NONE',  ( 10.96230482721425403, -14.55883922869198344, -77.50000000000000000 ) ) ;
#753 = PLANE ( 'NONE',  #13835 ) ;
#755 = CARTESIAN_POINT ( 'NONE',  ( -1.025333382651330166E-15, 0.6596962799366378194, 13.49999999999999645 ) ) ;
#754 = DIRECTION ( 'NONE',  ( 0.000000000000000000, 0.000000000000000000, 1.000000000000000000 ) ) ;
#756 = UNCERTAINTY_MEASURE_WITH_UNIT (LENGTH_MEASURE( 1.000000000000000082E-05 ), #23264, 'distance_accuracy_value', 'NONE');
#757 = DIRECTION ( 'NONE',  ( -1.000000000000000000, -0.000000000000000000, -0.000000000000000000 ) ) ;
#758 = ORIENTED_EDGE ( 'NONE', *, *, #30163, .F. ) ;
#759 = CARTESIAN_POINT ( 'NONE',  ( -363.0000000000000000, -135.0000000000000000, 114.0000000000000000 ) ) ;
#760 = DIRECTION ( 'NONE',  ( -0.000000000000000000, -5.145227585319922065E-49, -1.000000000000000000 ) ) ;
#761 = EDGE_CURVE ( 'NONE', #19084, #9157, #24545, .T. ) ;
#762 = EDGE_CURVE ( 'NONE', #30403, #3499, #15137, .T. ) ;
#763 = VERTEX_POINT ( 'NONE', #5153 ) ;
#764 = PRODUCT_DEFINITION ( 'UNKNOWN', '', #21844, #32398 ) ;
#765 = ORIENTED_EDGE ( 'NONE', *, *, #6752, .T. ) ;
#766 = AXIS2_PLACEMENT_3D ( 'NONE', #19908, #30749, #8331 ) ;
#767 = AXIS2_PLACEMENT_3D ( 'NONE', #17195, #9516, #17375 ) ;
#768 = VECTOR ( 'NONE', #8009, 1000.000000000000000 ) ;
#769 = VERTEX_POINT ( 'NONE', #186 ) ;
#770 = CARTESIAN_POINT ( 'NONE',  ( -442.0000000000000000, -125.0000000000000000, -105.9999999999999574 ) ) ;
#771 = ORIENTED_EDGE ( 'NONE', *, *, #682, .T. ) ;
#772 = ORIENTED_EDGE ( 'NONE', *, *, #29347, .F. ) ;
#773 = CARTESIAN_POINT ( 'NONE',  ( -499.9999999999999432, -113.0000000000000000, -162.9999999999999716 ) ) ;
#774 = ORIENTED_EDGE ( 'NONE', *, *, #8706, .F. ) ;
#775 = LINE ( 'NONE', #34040, #30580 ) ;
#776 = DIRECTION ( 'NONE',  ( 0.000000000000000000, -1.000000000000000000, 0.000000000000000000 ) ) ;
#777 = ORIENTED_EDGE ( 'NONE', *, *, #34334, .F. ) ;
#778 = ORIENTED_EDGE ( 'NONE', *, *, #32742, .T. ) ;
#779 = FACE_OUTER_BOUND ( 'NONE', #30050, .T. ) ;
#780 = DIRECTION ( 'NONE',  ( 0.000000000000000000, 1.000000000000000000, 5.145227585319922065E-49 ) ) ;
#781 = CARTESIAN_POINT ( 'NONE',  ( 109.5465872284862741, -3.505526250977489156, -11.99932421786962067 ) ) ;
#782 = DIRECTION ( 'NONE',  ( 0.000000000000000000, 1.000000000000000000, 2.465190328815662439E-32 ) ) ;
#783 = PLANE ( 'NONE',  #1217 ) ;
#784 = ORIENTED_EDGE ( 'NONE', *, *, #22789, .T. ) ;
#785 = CARTESIAN_POINT ( 'NONE',  ( -20.00000000000007461, 136.9999999999999432, 190.9999999999999716 ) ) ;
#786 = CIRCLE ( 'NONE', #28069, 2.033421858999711507 ) ;
#787 = DIRECTION ( 'NONE',  ( 0.000000000000000000, 1.836970198721029441E-16, -1.000000000000000000 ) ) ;
#788 = ORIENTED_EDGE ( 'NONE', *, *, #21266, .F. ) ;
#789 = CARTESIAN_POINT ( 'NONE',  ( -499.9999999999999432, 112.9999999999999574, 190.9999999999999716 ) ) ;
#790 = FACE_OUTER_BOUND ( 'NONE', #10832, .T. ) ;
#791 = LINE ( 'NONE', #11664, #19521 ) ;
#792 = AXIS2_PLACEMENT_3D ( 'NONE', #33774, #1203, #17249 ) ;
#793 = LINE ( 'NONE', #15037, #16102 ) ;
#794 = AXIS2_PLACEMENT_3D ( 'NONE', #34240, #4849, #18070 ) ;
#795 = AXIS2_PLACEMENT_3D ( 'NONE', #25885, #23221, #30872 ) ;
#796 = CARTESIAN_POINT ( 'NONE',  ( 12.46788440507149964, 30.06253867087536946, 68.31122994652405112 ) ) ;
#797 = VERTEX_POINT ( 'NONE', #7654 ) ;
#798 = DIRECTION ( 'NONE',  ( 0.000000000000000000, 0.000000000000000000, 1.000000000000000000 ) ) ;
#800 = FACE_OUTER_BOUND ( 'NONE', #12597, .T. ) ;
#799 = FACE_OUTER_BOUND ( 'NONE', #15356, .T. ) ;
#801 = EDGE_CURVE ( 'NONE', #5991, #17491, #18552, .T. ) ;
#802 = VERTEX_POINT ( 'NONE', #25076 ) ;
#803 =( REPRESENTATION_RELATIONSHIP ('NONE','NONE', #23037, #15767 ) REPRESENTATION_RELATIONSHIP_WITH_TRANSFORMATION ( #4733 )SHAPE_REPRESENTATION_RELATIONSHIP( ) );
#804 = DIRECTION ( 'NONE',  ( 0.000000000000000000, 1.000000000000000000, 0.000000000000000000 ) ) ;
#805 = DIRECTION ( 'NONE',  ( 0.000000000000000000, 0.000000000000000000, 1.000000000000000000 ) ) ;
#806 = EDGE_CURVE ( 'NONE', #26021, #12216, #16751, .T. ) ;
#807 = ORIENTED_EDGE ( 'NONE', *, *, #3982, .T. ) ;
#808 = AXIS2_PLACEMENT_3D ( 'NONE', #12779, #23621, #34477 ) ;
#809 = EDGE_CURVE ( 'NONE', #1130, #16248, #20815, .T. ) ;
#810 = ORIENTED_EDGE ( 'NONE', *, *, #19374, .T. ) ;
#811 = CARTESIAN_POINT ( 'NONE',  ( 104.6049621835381487, -5.727834534852265236, -4.841784820303065118 ) ) ;
#812 = ORIENTED_EDGE ( 'NONE', *, *, #27179, .F. ) ;
#813 = ORIENTED_EDGE ( 'NONE', *, *, #20854, .T. ) ;
#814 = B_SPLINE_CURVE_WITH_KNOTS ( 'NONE', 3,
 ( #14475, #31011, #28163, #940, #14997, #1459 ),
 .UNSPECIFIED., .F., .F.,
 ( 4, 2, 4 ),
 ( 2.343813143889068798E-07, 0.001873432713173589807, 0.003746631045032783325 ),
 .UNSPECIFIED. ) ;
#815 = CARTESIAN_POINT ( 'NONE',  ( -35.00000000000000000, -4.831299144296466785, 15.81122994652406355 ) ) ;
#816 = CIRCLE ( 'NONE', #30389, 30.47050528711512030 ) ;
#817 = EDGE_CURVE ( 'NONE', #591, #27019, #22610, .T. ) ;
#818 = CARTESIAN_POINT ( 'NONE',  ( 0.000000000000000000, 0.000000000000000000, 0.000000000000000000 ) ) ;
#819 = LINE ( 'NONE', #5782, #3363 ) ;
#820 = AXIS2_PLACEMENT_3D ( 'NONE', #3238, #14113, #27797 ) ;
#821 = CYLINDRICAL_SURFACE ( 'NONE', #2018, 1.155000000000000027 ) ;
#822 = CARTESIAN_POINT ( 'NONE',  ( 0.07098932849787087385, 31.23843357299762857, -5.357709411917221054 ) ) ;
#823 = ORIENTED_EDGE ( 'NONE', *, *, #1952, .F. ) ;
#824 = ORIENTED_EDGE ( 'NONE', *, *, #23128, .F. ) ;
#825 = AXIS2_PLACEMENT_3D ( 'NONE', #30486, #20162, #31187 ) ;
#827 = MANIFOLD_SOLID_BREP ( 'Cut-Extrude2', #21909 ) ;
#826 = CARTESIAN_POINT ( 'NONE',  ( 212.5000000000000000, 9.184850993605147944E-16, -7.500000000000000000 ) ) ;
#828 = LINE ( 'NONE', #27867, #26026 ) ;
#829 = DIRECTION ( 'NONE',  ( 0.000000000000000000, 0.000000000000000000, -1.000000000000000000 ) ) ;
#830 = DIRECTION ( 'NONE',  ( 0.000000000000000000, 0.000000000000000000, 1.000000000000000000 ) ) ;
#831 = CARTESIAN_POINT ( 'NONE',  ( 0.000000000000000000, -5.984944020946091570, 31.37417528048439763 ) ) ;
#832 = LINE ( 'NONE', #5974, #7684 ) ;
#833 = CARTESIAN_POINT ( 'NONE',  ( 1.394999999999999574, 6.714005886385425725, -33.75364837705166110 ) ) ;
#834 = ORIENTED_EDGE ( 'NONE', *, *, #5373, .F. ) ;
#835 = CARTESIAN_POINT ( 'NONE',  ( -36.04853892210773836, 11.59936550071286376, 68.31122994652405112 ) ) ;
#836 = CARTESIAN_POINT ( 'NONE',  ( -15.99999999999998579, 136.9999999999999716, -175.0000000000000284 ) ) ;
#837 = DIRECTION ( 'NONE',  ( 0.000000000000000000, 1.000000000000000000, 1.224646799147353207E-16 ) ) ;
#838 = ORIENTED_EDGE ( 'NONE', *, *, #33279, .T. ) ;
#839 = AXIS2_PLACEMENT_3D ( 'NONE', #13257, #7899, #20906 ) ;
#840 = B_SPLINE_CURVE_WITH_KNOTS ( 'NONE', 3,
 ( #9936, #25292, #8926, #10109, #6597, #26129 ),
 .UNSPECIFIED., .F., .F.,
 ( 4, 2, 4 ),
 ( 4.404817133574835894E-07, 0.001874269703891905288, 0.003748098926070445643 ),
 .UNSPECIFIED. ) ;
#841 = DIRECTION ( 'NONE',  ( 0.000000000000000000, -1.000000000000000000, 6.123233995736766036E-17 ) ) ;
#842 = VERTEX_POINT ( 'NONE', #31436 ) ;
#843 = B_SPLINE_CURVE_WITH_KNOTS ( 'NONE', 3,
 ( #21300, #7758, #27153, #24466, #15972, #22001, #29835, #11154, #291, #21814, #5777, #7935, #18814, #32316, #10626, #26809, #19169, #2595, #18644, #2419, #21476, #13297, #10795, #24129, #13464, #16203, #32670, #8111, #18989, #24650, #8291, #5433, #16326, #27325, #32840, #2942 ),
 .UNSPECIFIED., .F., .F.,
 ( 4, 2, 2, 2, 2, 2, 2, 2, 2, 2, 2, 2, 2, 2, 2, 2, 2, 4 ),
 ( 4.603728119458012508E-18, 0.001035696236907480625, 0.002071392473814956912, 0.003107088710722432333, 0.004142784947629908621, 0.005178481184537384041, 0.006214177421444859462, 0.007249873658352335749, 0.007767721776806054378, 0.008285569895259772139, 0.009321266132167249294, 0.01035696236907472818, 0.01087481048752844855, 0.01139265860598217064, 0.01242835484288958188, 0.01449974731670443211, 0.01553544355361186069, 0.01657113979051928407 ),
 .UNSPECIFIED. ) ;
#844 = CARTESIAN_POINT ( 'NONE',  ( -365.0000000000000000, 130.9999999999999716, 111.9999999999999858 ) ) ;
#845 = AXIS2_PLACEMENT_3D ( 'NONE', #22762, #9054, #27387 ) ;
#846 = CARTESIAN_POINT ( 'NONE',  ( -100.4098818337750885, 2.281765576240580629, 12.29396198687797259 ) ) ;
#847 = CARTESIAN_POINT ( 'NONE',  ( -349.0000000000000000, 134.9999999999999716, 126.0000000000000000 ) ) ;
#848 = VECTOR ( 'NONE', #31003, 1000.000000000000000 ) ;
#849 = ORIENTED_EDGE ( 'NONE', *, *, #21052, .T. ) ;
#850 = AXIS2_PLACEMENT_3D ( 'NONE', #14253, #6390, #19596 ) ;
#851 = FACE_OUTER_BOUND ( 'NONE', #26589, .T. ) ;
#852 = LINE ( 'NONE', #22571, #25306 ) ;
#853 = LINE ( 'NONE', #6703, #25713 ) ;
#854 = VECTOR ( 'NONE', #2989, 1000.000000000000000 ) ;
#855 = EDGE_CURVE ( 'NONE', #32236, #2476, #6011, .T. ) ;
#856 = ORIENTED_EDGE ( 'NONE', *, *, #12997, .T. ) ;
#857 = ADVANCED_FACE ( 'NONE', ( #30253 ), #22251, .F. ) ;
#858 = EDGE_CURVE ( 'NONE', #7203, #16288, #5854, .T. ) ;
#859 = CARTESIAN_POINT ( 'NONE',  ( 831.2128046545705047, 1216.097730733147273, 1753.598338701303419 ) ) ;
#860 = FACE_OUTER_BOUND ( 'NONE', #11273, .T. ) ;
#861 = ORIENTED_EDGE ( 'NONE', *, *, #7933, .F. ) ;
#862 = CARTESIAN_POINT ( 'NONE',  ( -430.0000000000000000, -119.0000000000000000, 111.9999999999999858 ) ) ;
#863 = CARTESIAN_POINT ( 'NONE',  ( -28.00450684652667022, 16.58167570419056247, -36.68877005347593467 ) ) ;
#864 = CIRCLE ( 'NONE', #19071, 4.000000000000003553 ) ;
#865 = DIRECTION ( 'NONE',  ( 0.000000000000000000, -1.000000000000000000, -1.836970198721029934E-16 ) ) ;
#866 = FACE_OUTER_BOUND ( 'NONE', #16501, .T. ) ;
#867 = ORIENTED_EDGE ( 'NONE', *, *, #33939, .F. ) ;
#868 = ORIENTED_EDGE ( 'NONE', *, *, #240, .F. ) ;
#869 = ORIENTED_EDGE ( 'NONE', *, *, #27770, .T. ) ;
#870 = CARTESIAN_POINT ( 'NONE',  ( 10.62930655775863364, -36.34639295086972766, 68.31122994652405112 ) ) ;
#871 = VECTOR ( 'NONE', #29284, 1000.000000000000000 ) ;
#872 = EDGE_CURVE ( 'NONE', #17833, #17981, #14432, .T. ) ;
#873 = DIRECTION ( 'NONE',  ( 1.000000000000000000, 0.000000000000000000, 0.000000000000000000 ) ) ;
#874 = DIRECTION ( 'NONE',  ( 0.000000000000000000, 0.000000000000000000, 1.000000000000000000 ) ) ;
#875 = FACE_OUTER_BOUND ( 'NONE', #18381, .T. ) ;
#876 = ORIENTED_EDGE ( 'NONE', *, *, #5437, .T. ) ;
#877 = ORIENTED_EDGE ( 'NONE', *, *, #2719, .T. ) ;
#878 = AXIS2_PLACEMENT_3D ( 'NONE', #15837, #32184, #18849 ) ;
#879 = DIRECTION ( 'NONE',  ( 0.000000000000000000, 0.000000000000000000, -1.000000000000000000 ) ) ;
#880 = ORIENTED_EDGE ( 'NONE', *, *, #150, .F. ) ;
#881 = CIRCLE ( 'NONE', #13382, 4.750000000000004441 ) ;
#882 = EDGE_CURVE ( 'NONE', #28417, #9255, #19687, .T. ) ;
#883 = CARTESIAN_POINT ( 'NONE',  ( -442.0000000000000000, -124.9999999999999858, -77.99999999999997158 ) ) ;
#884 = DIRECTION ( 'NONE',  ( 0.000000000000000000, 0.000000000000000000, -1.000000000000000000 ) ) ;
#885 = ORIENTED_EDGE ( 'NONE', *, *, #10951, .F. ) ;
#887 = EDGE_CURVE ( 'NONE', #24475, #21957, #33276, .T. ) ;
#886 = ORIENTED_EDGE ( 'NONE', *, *, #32162, .T. ) ;
#888 = FACE_OUTER_BOUND ( 'NONE', #22918, .T. ) ;
#889 = CYLINDRICAL_SURFACE ( 'NONE', #9256, 3.999999999999976019 ) ;
#890 = VERTEX_POINT ( 'NONE', #25929 ) ;
#891 = CARTESIAN_POINT ( 'NONE',  ( 22.89764159710615132, -1.579009122040562207, -77.50000000000000000 ) ) ;
#892 = CARTESIAN_POINT ( 'NONE',  ( 15.99999999999998579, -137.0000000000000000, -155.0000000000000284 ) ) ;
#893 = EDGE_CURVE ( 'NONE', #25849, #6490, #16930, .T. ) ;
#894 = LINE ( 'NONE', #11935, #25790 ) ;
#895 = VECTOR ( 'NONE', #17120, 1000.000000000000000 ) ;
#896 = CARTESIAN_POINT ( 'NONE',  ( -110.0477662801539935, -0.8438318447813555334, 12.47259309357265522 ) ) ;
#897 = DIRECTION ( 'NONE',  ( 0.000000000000000000, 0.000000000000000000, 1.000000000000000000 ) ) ;
#898 = AXIS2_PLACEMENT_3D ( 'NONE', #26736, #2349, #13228 ) ;
#899 = ORIENTED_EDGE ( 'NONE', *, *, #20430, .F. ) ;
#900 = ORIENTED_EDGE ( 'NONE', *, *, #18867, .T. ) ;
#901 = EDGE_CURVE ( 'NONE', #33356, #2161, #3374, .T. ) ;
#902 = EDGE_CURVE ( 'NONE', #26131, #14276, #11579, .T. ) ;
#903 = DIRECTION ( 'NONE',  ( 2.631201909438060269E-14, -5.396010391056495992E-16, 0.9999999999999998890 ) ) ;
#904 = VERTEX_POINT ( 'NONE', #6207 ) ;
#905 = AXIS2_PLACEMENT_3D ( 'NONE', #32431, #24589, #8050 ) ;
#906 = ORIENTED_EDGE ( 'NONE', *, *, #16042, .T. ) ;
#907 = CARTESIAN_POINT ( 'NONE',  ( 212.5000000000000000, 0.000000000000000000, 0.000000000000000000 ) ) ;
#908 = CARTESIAN_POINT ( 'NONE',  ( 8.000000000000000000, 0.000000000000000000, 0.000000000000000000 ) ) ;
#909 = ITEM_DEFINED_TRANSFORMATION ( 'NONE', 'NONE', #20638,  #28566 ) ;
#910 = ORIENTED_EDGE ( 'NONE', *, *, #5324, .F. ) ;
#911 = CARTESIAN_POINT ( 'NONE',  ( -365.0000000000000000, -117.0000000000000000, 113.9999999999999858 ) ) ;
#912 = CARTESIAN_POINT ( 'NONE',  ( -100.9389840009208825, -3.127506413740531510, -12.10571963949988650 ) ) ;
#913 = VECTOR ( 'NONE', #9835, 1000.000000000000000 ) ;
#915 = DIRECTION ( 'NONE',  ( -1.000000000000000000, -0.000000000000000000, -0.000000000000000000 ) ) ;
#914 = CARTESIAN_POINT ( 'NONE',  ( -363.0000000000000000, -135.0000000000000000, 126.0000000000000000 ) ) ;
#916 = VERTEX_POINT ( 'NONE', #17758 ) ;
#917 = ORIENTED_EDGE ( 'NONE', *, *, #6958, .T. ) ;
#918 = CARTESIAN_POINT ( 'NONE',  ( -449.9999999999999432, -124.9999999999999716, 132.0000000000000000 ) ) ;
#919 = AXIS2_PLACEMENT_3D ( 'NONE', #30994, #17497, #28147 ) ;
#920 = DIRECTION ( 'NONE',  ( 0.000000000000000000, 0.000000000000000000, -1.000000000000000000 ) ) ;
#921 = CARTESIAN_POINT ( 'NONE',  ( -449.9999999999999432, -125.0000000000000000, 187.0000000000000000 ) ) ;
#922 = DIRECTION ( 'NONE',  ( 1.000000000000000000, -0.000000000000000000, 0.000000000000000000 ) ) ;
#923 = ORIENTED_EDGE ( 'NONE', *, *, #10157, .T. ) ;
#924 = EDGE_CURVE ( 'NONE', #20300, #23023, #4196, .T. ) ;
#925 = CARTESIAN_POINT ( 'NONE',  ( 0.07094833174329351344, -22.12275578582332258, -22.69570394412150094 ) ) ;
#926 = EDGE_CURVE ( 'NONE', #18645, #8559, #4534, .T. ) ;
#927 = CARTESIAN_POINT ( 'NONE',  ( -19.99999999999998934, 124.9999999999999716, 155.0000000000000000 ) ) ;
#928 = ORIENTED_EDGE ( 'NONE', *, *, #4882, .F. ) ;
#929 = CIRCLE ( 'NONE', #2617, 1.999999999999999112 ) ;
#930 = DIRECTION ( 'NONE',  ( -1.000000000000000000, -0.000000000000000000, 0.000000000000000000 ) ) ;
#931 = CARTESIAN_POINT ( 'NONE',  ( -499.9999999999999432, 136.9999999999999432, -159.0000000000000000 ) ) ;
#932 = DIRECTION ( 'NONE',  ( 0.000000000000000000, 0.000000000000000000, -1.000000000000000000 ) ) ;
#934 = CARTESIAN_POINT ( 'NONE',  ( 1.205771365940041528, 7.794228634059941818, 13.49999999999999645 ) ) ;
#933 = CARTESIAN_POINT ( 'NONE',  ( 0.000000000000000000, 0.000000000000000000, 0.000000000000000000 ) ) ;
#935 = AXIS2_PLACEMENT_3D ( 'NONE', #4865, #34789, #15576 ) ;
#937 = EDGE_CURVE ( 'NONE', #22497, #8202, #34818, .T. ) ;
#936 = CARTESIAN_POINT ( 'NONE',  ( 53.89849999999999852, 9.797174393178825657E-16, -8.000000000000000000 ) ) ;
#938 = CARTESIAN_POINT ( 'NONE',  ( 0.07098930208213954929, -22.12324074713423983, 22.69596835361121379 ) ) ;
#939 = VERTEX_POINT ( 'NONE', #24113 ) ;
#940 = CARTESIAN_POINT ( 'NONE',  ( 2.265105836449367249, -9.574141296992072725, -31.97728166840280295 ) ) ;
#941 = DIRECTION ( 'NONE',  ( -1.000000000000000000, 0.000000000000000000, 0.000000000000000000 ) ) ;
#942 = PRODUCT_DEFINITION_SHAPE ( 'NONE', 'NONE',  #35174 ) ;
#943 = VECTOR ( 'NONE', #26555, 1000.000000000000000 ) ;
#944 = ORIENTED_EDGE ( 'NONE', *, *, #27551, .T. ) ;
#945 = CIRCLE ( 'NONE', #12819, 4.000000000000003553 ) ;
#946 = ORIENTED_EDGE ( 'NONE', *, *, #3678, .T. ) ;
#947 = EDGE_LOOP ( 'NONE', ( #30573, #9309, #21201, #23371 ) ) ;
#948 = CARTESIAN_POINT ( 'NONE',  ( -12.00000000000001066, 104.9999999999999858, -155.0000000000000000 ) ) ;
#949 = VERTEX_POINT ( 'NONE', #26096 ) ;
#950 = ORIENTED_EDGE ( 'NONE', *, *, #18415, .F. ) ;
#951 = EDGE_CURVE ( 'NONE', #29695, #26014, #34640, .T. ) ;
#952 = FACE_OUTER_BOUND ( 'NONE', #1655, .T. ) ;
#953 = VECTOR ( 'NONE', #12900, 1000.000000000000000 ) ;
#954 = ITEM_DEFINED_TRANSFORMATION ( 'NONE', 'NONE', #20088,  #28566 ) ;
#955 = ORIENTED_EDGE ( 'NONE', *, *, #9993, .T. ) ;
#956 = CARTESIAN_POINT ( 'NONE',  ( 1.749999999999999778, 0.000000000000000000, 0.000000000000000000 ) ) ;
#957 = DIRECTION ( 'NONE',  ( 0.000000000000000000, 0.000000000000000000, -1.000000000000000000 ) ) ;
#958 = EDGE_LOOP ( 'NONE', ( #8878, #27960, #18209, #24992 ) ) ;
#959 = ORIENTED_EDGE ( 'NONE', *, *, #2723, .T. ) ;
#960 = CARTESIAN_POINT ( 'NONE',  ( 15.44711578872682267, -28.64595934308655600, 68.31122994652405112 ) ) ;
#961 = DIRECTION ( 'NONE',  ( -1.000000000000000000, 0.000000000000000000, 0.000000000000000000 ) ) ;
#962 = AXIS2_PLACEMENT_3D ( 'NONE', #16567, #5499, #19235 ) ;
#963 = EDGE_CURVE ( 'NONE', #18812, #2924, #2407, .T. ) ;
#964 = CARTESIAN_POINT ( 'NONE',  ( -3.250000000000000000, 5.404196845913421754, 3.180000000000000160 ) ) ;
#965 = DIRECTION ( 'NONE',  ( -1.000000000000000000, -0.000000000000000000, 0.000000000000000000 ) ) ;
#966 = CARTESIAN_POINT ( 'NONE',  ( -12.00000000000003908, -134.9999999999999716, -154.9999999999999716 ) ) ;
#967 = ORIENTED_EDGE ( 'NONE', *, *, #21553, .T. ) ;
#968 = EDGE_CURVE ( 'NONE', #34921, #949, #21287, .T. ) ;
#969 = AXIS2_PLACEMENT_3D ( 'NONE', #27218, #29899, #2828 ) ;
#970 = DIRECTION ( 'NONE',  ( 1.000000000000000000, 0.000000000000000000, -1.232595164407831220E-32 ) ) ;
#971 = EDGE_CURVE ( 'NONE', #5416, #26553, #2066, .T. ) ;
#972 = CARTESIAN_POINT ( 'NONE',  ( -105.0000000000000000, 0.000000000000000000, 60.00000000000000000 ) ) ;
#973 = ORIENTED_EDGE ( 'NONE', *, *, #9241, .T. ) ;
#974 = DIRECTION ( 'NONE',  ( -0.000000000000000000, 1.000000000000000000, 0.000000000000000000 ) ) ;
#975 = LINE ( 'NONE', #1321, #16054 ) ;
#976 = DIRECTION ( 'NONE',  ( 0.000000000000000000, -1.000000000000000000, -1.836970198721029934E-16 ) ) ;
#977 = PLANE ( 'NONE',  #12699 ) ;
#978 = DIRECTION ( 'NONE',  ( 1.000000000000000000, 0.000000000000000000, 0.000000000000000000 ) ) ;
#979 = DIRECTION ( 'NONE',  ( -0.000000000000000000, -0.000000000000000000, -1.000000000000000000 ) ) ;
#980 = VERTEX_POINT ( 'NONE', #12938 ) ;
#981 = CARTESIAN_POINT ( 'NONE',  ( -0.9727285265192158192, -1.747512292859697114, 5.429999999999999716 ) ) ;
#983 = PLANE ( 'NONE',  #23120 ) ;
#982 = DIRECTION ( 'NONE',  ( -1.000000000000000000, -0.000000000000000000, 0.000000000000000000 ) ) ;
#984 = VERTEX_POINT ( 'NONE', #15788 ) ;
#985 = PRODUCT ( 'chainlinkage', 'chainlinkage', '', ( #30098 ) ) ;
#986 = FACE_OUTER_BOUND ( 'NONE', #14814, .T. ) ;
#987 = AXIS2_PLACEMENT_3D ( 'NONE', #7647, #179, #11034 ) ;
#988 = ORIENTED_EDGE ( 'NONE', *, *, #13058, .F. ) ;
#989 = ORIENTED_EDGE ( 'NONE', *, *, #16056, .T. ) ;
#990 = AXIS2_PLACEMENT_3D ( 'NONE', #24668, #10640, #10812 ) ;
#991 = AXIS2_PLACEMENT_3D ( 'NONE', #11970, #9804, #22814 ) ;
#992 = ORIENTED_EDGE ( 'NONE', *, *, #23128, .T. ) ;
#993 = CARTESIAN_POINT ( 'NONE',  ( -445.9999999999999432, 104.9999999999999858, -162.9999999999999716 ) ) ;
#994 = ORIENTED_EDGE ( 'NONE', *, *, #20204, .T. ) ;
#995 = VERTEX_POINT ( 'NONE', #18457 ) ;
#996 = CARTESIAN_POINT ( 'NONE',  ( -9.978866888775426602, 14.09580098603202458, -67.50000000000000000 ) ) ;
#998 = FACE_OUTER_BOUND ( 'NONE', #9441, .T. ) ;
#997 = AXIS2_PLACEMENT_3D ( 'NONE', #20960, #9749, #4739 ) ;
#999 = CARTESIAN_POINT ( 'NONE',  ( 0.000000000000000000, -33.69708579775584667, 49.43553178847298568 ) ) ;
#1000 = LINE ( 'NONE', #22721, #30171 ) ;
#1001 = VERTEX_POINT ( 'NONE', #4369 ) ;
#1002 = ORIENTED_EDGE ( 'NONE', *, *, #10125, .T. ) ;
#1003 = EDGE_CURVE ( 'NONE', #17724, #17949, #11737, .T. ) ;
#1004 = CARTESIAN_POINT ( 'NONE',  ( 8.986540508143580297, 33.69708579775584667, 68.31122994652405112 ) ) ;
#1005 = DIRECTION ( 'NONE',  ( 1.000000000000000000, -0.000000000000000000, -0.000000000000000000 ) ) ;
#1006 = LINE ( 'NONE', #478, #28288 ) ;
#1007 = EDGE_CURVE ( 'NONE', #10470, #34124, #5457, .T. ) ;
#1008 = CARTESIAN_POINT ( 'NONE',  ( 1.040000000000000924, -18.66807150955393624, -28.91175816027522316 ) ) ;
#1009 = CARTESIAN_POINT ( 'NONE',  ( -8.000000000000000000, 0.000000000000000000, -15.69999999999999929 ) ) ;
#1010 = CARTESIAN_POINT ( 'NONE',  ( 145.0000000000000568, -99.56883598056833762, -180.0000000000000000 ) ) ;
#1011 = EDGE_CURVE ( 'NONE', #29748, #30400, #2067, .T. ) ;
#1012 = AXIS2_PLACEMENT_3D ( 'NONE', #21639, #26986, #3122 ) ;
#1013 = DIRECTION ( 'NONE',  ( -1.000000000000000000, 0.000000000000000000, 0.000000000000000000 ) ) ;
#1014 = ORIENTED_EDGE ( 'NONE', *, *, #28076, .T. ) ;
#1015 = EDGE_CURVE ( 'NONE', #2086, #14870, #28769, .T. ) ;
#1016 = LINE ( 'NONE', #17232, #19707 ) ;
#1017 = DIRECTION ( 'NONE',  ( 0.000000000000000000, 1.310824597558155437E-49, 1.000000000000000000 ) ) ;
#1018 = CARTESIAN_POINT ( 'NONE',  ( 0.000000000000000000, 0.000000000000000000, -13.49999999999999822 ) ) ;
#1019 = EDGE_LOOP ( 'NONE', ( #8379, #30017, #22732, #21816 ) ) ;
#1020 = AXIS2_PLACEMENT_3D ( 'NONE', #3481, #19182, #27167 ) ;
#1021 =( REPRESENTATION_RELATIONSHIP ('NONE','NONE', #23037, #15767 ) REPRESENTATION_RELATIONSHIP_WITH_TRANSFORMATION ( #19737 )SHAPE_REPRESENTATION_RELATIONSHIP( ) );
#1022 = CARTESIAN_POINT ( 'NONE',  ( 22.89764159710611224, 17.63622956525712482, -87.50000000000000000 ) ) ;
#1023 = ORIENTED_EDGE ( 'NONE', *, *, #17027, .T. ) ;
#1024 = DIRECTION ( 'NONE',  ( 0.000000000000000000, 1.836970198721029441E-16, -1.000000000000000000 ) ) ;
#1025 = EDGE_CURVE ( 'NONE', #26862, #18446, #31608, .T. ) ;
#1026 = CIRCLE ( 'NONE', #29448, 2.525000000000000799 ) ;
#1027 = ORIENTED_EDGE ( 'NONE', *, *, #16202, .T. ) ;
#1028 = DIRECTION ( 'NONE',  ( -3.040835319149746090E-31, -1.000000000000000000, 3.748118910144520367E-63 ) ) ;
#1029 = DIRECTION ( 'NONE',  ( -0.000000000000000000, -0.000000000000000000, -1.000000000000000000 ) ) ;
#1030 = DIRECTION ( 'NONE',  ( -0.000000000000000000, -0.000000000000000000, -1.000000000000000000 ) ) ;
#1031 = VERTEX_POINT ( 'NONE', #26619 ) ;
#1032 = DIRECTION ( 'NONE',  ( -7.893605728314051750E-14, 1.618803117314786530E-15, 1.000000000000000000 ) ) ;
#1033 = CYLINDRICAL_SURFACE ( 'NONE', #4520, 16.19999999999999929 ) ;
#1034 = ORIENTED_EDGE ( 'NONE', *, *, #29447, .F. ) ;
#1035 = FACE_BOUND ( 'NONE', #9089, .T. ) ;
#1036 = FACE_OUTER_BOUND ( 'NONE', #26947, .T. ) ;
#1037 = AXIS2_PLACEMENT_3D ( 'NONE', #21545, #32381, #7826 ) ;
#1038 = VECTOR ( 'NONE', #10976, 1000.000000000000000 ) ;
#1039 = CARTESIAN_POINT ( 'NONE',  ( 187.4264068711928530, -12.50000000000001066, 15.00000000000001243 ) ) ;
#1040 = DIRECTION ( 'NONE',  ( 0.8835120444460231592, -0.4684084406997896521, -0.000000000000000000 ) ) ;
#1041 = VERTEX_POINT ( 'NONE', #2236 ) ;
#1042 = ORIENTED_EDGE ( 'NONE', *, *, #9870, .T. ) ;
#1043 = AXIS2_PLACEMENT_3D ( 'NONE', #2995, #22054, #19392 ) ;
#1044 = ORIENTED_EDGE ( 'NONE', *, *, #6337, .F. ) ;
#1045 = DIRECTION ( 'NONE',  ( 0.000000000000000000, 1.000000000000000000, 0.000000000000000000 ) ) ;
#1046 = PLANE ( 'NONE',  #15456 ) ;
#1047 = AXIS2_PLACEMENT_3D ( 'NONE', #8394, #6728, #13919 ) ;
#1048 = B_SPLINE_CURVE_WITH_KNOTS ( 'NONE', 3,
 ( #12793, #34310, #605, #32333, #16164, #22322 ),
 .UNSPECIFIED., .F., .F.,
 ( 4, 2, 4 ),
 ( 4.404817060652725496E-07, 0.001874269649560036423, 0.003748098817414007630 ),
 .UNSPECIFIED. ) ;
#1049 = CARTESIAN_POINT ( 'NONE',  ( 1.040000000000001146, 21.72796464722008025, 26.68861566460903134 ) ) ;
#1050 = CARTESIAN_POINT ( 'NONE',  ( -11.83261234297099662, -30.31820670846268229, 68.31122994652405112 ) ) ;
#1051 = ORIENTED_EDGE ( 'NONE', *, *, #3243, .F. ) ;
#1052 = CARTESIAN_POINT ( 'NONE',  ( 2.606461907020827251, -31.53621309121735194, 6.848028948309839770 ) ) ;
#1053 = CARTESIAN_POINT ( 'NONE',  ( 32.81769769215652133, 18.87860345536237006, 49.43553178847298568 ) ) ;
#1054 = VERTEX_POINT ( 'NONE', #18119 ) ;
#1055 = EDGE_CURVE ( 'NONE', #26315, #29922, #21463, .T. ) ;
#1056 = CARTESIAN_POINT ( 'NONE',  ( 0.000000000000000000, 0.000000000000000000, 0.000000000000000000 ) ) ;
#1057 = ADVANCED_FACE ( 'NONE', ( #28943 ), #34459, .F. ) ;
#1058 = DIRECTION ( 'NONE',  ( -1.000000000000000000, -3.469446951953834515E-18, 0.000000000000000000 ) ) ;
#1059 = VECTOR ( 'NONE', #20484, 1000.000000000000000 ) ;
#1060 = ORIENTED_EDGE ( 'NONE', *, *, #27470, .F. ) ;
#1061 = ORIENTED_EDGE ( 'NONE', *, *, #9092, .F. ) ;
#1062 = AXIS2_PLACEMENT_3D ( 'NONE', #28487, #22452, #19618 ) ;
#1063 = ADVANCED_FACE ( 'NONE', ( #13287 ), #10427, .F. ) ;
#1064 = EDGE_CURVE ( 'NONE', #21836, #5569, #31063, .T. ) ;
#1065 = DIRECTION ( 'NONE',  ( -1.000000000000000000, -0.000000000000000000, -0.000000000000000000 ) ) ;
#1066 = ORIENTED_EDGE ( 'NONE', *, *, #40, .F. ) ;
#1067 = LINE ( 'NONE', #27933, #15226 ) ;
#1068 = LINE ( 'NONE', #892, #6351 ) ;
#1069 = CARTESIAN_POINT ( 'NONE',  ( 19.99999999999998224, 134.9999999999998863, 187.0000000000000000 ) ) ;
#1070 = CIRCLE ( 'NONE', #29493, 4.750000000000004441 ) ;
#1071 = CARTESIAN_POINT ( 'NONE',  ( -7.218132304338721994, -1.866624223957557893, -0.7500000000000000000 ) ) ;
#1072 = DIRECTION ( 'NONE',  ( -1.000000000000000000, 0.000000000000000000, -1.300283923313630633E-47 ) ) ;
#1073 = CARTESIAN_POINT ( 'NONE',  ( 19.99999999999998224, 134.9999999999999432, -186.9999999999999716 ) ) ;
#1075 = ADVANCED_FACE ( 'NONE', ( #32306 ), #1883, .T. ) ;
#1074 = ORIENTED_EDGE ( 'NONE', *, *, #12659, .T. ) ;
#1076 = ORIENTED_EDGE ( 'NONE', *, *, #23191, .F. ) ;
#1077 = CARTESIAN_POINT ( 'NONE',  ( 834.6705126614218671, 1183.782206524897447, 1753.598338701303192 ) ) ;
#1078 = EDGE_LOOP ( 'NONE', ( #8545, #2209, #34917, #26406 ) ) ;
#1079 = DIRECTION ( 'NONE',  ( 0.000000000000000000, 1.836970198721029441E-16, -1.000000000000000000 ) ) ;
#1080 = EDGE_CURVE ( 'NONE', #5077, #15056, #15786, .T. ) ;
#1081 = VECTOR ( 'NONE', #9547, 1000.000000000000000 ) ;
#1082 = EDGE_CURVE ( 'NONE', #13600, #23413, #21990, .T. ) ;
#1083 = CARTESIAN_POINT ( 'NONE',  ( -31.48191842954600617, 28.04684603917314334, 55.43429723762557870 ) ) ;
#1084 = ITEM_DEFINED_TRANSFORMATION ( 'NONE', 'NONE', #2986,  #28566 ) ;
#1085 = ORIENTED_EDGE ( 'NONE', *, *, #12660, .T. ) ;
#1086 = DIRECTION ( 'NONE',  ( -1.000000000000000000, 0.000000000000000000, 0.000000000000000000 ) ) ;
#1087 = COLOUR_RGB ( '',0.7921568627450980005, 0.8196078431372548767, 0.9333333333333333481 ) ;
#1088 = CARTESIAN_POINT ( 'NONE',  ( 2.719010679974587230, -18.14847849655048506, 25.98417794693611782 ) ) ;
#1089 = ORIENTED_EDGE ( 'NONE', *, *, #19291, .F. ) ;
#1090 = ORIENTED_EDGE ( 'NONE', *, *, #16252, .F. ) ;
#1091 = CARTESIAN_POINT ( 'NONE',  ( 18.63894936814906700, 26.67946662374790279, 68.31122994652405112 ) ) ;
#1092 = DIRECTION ( 'NONE',  ( -1.000000000000000000, 0.000000000000000000, 0.000000000000000000 ) ) ;
#1093 = CARTESIAN_POINT ( 'NONE',  ( 1.749999999999999778, 34.10861917999622506, -4.581348211831717698 ) ) ;
#1094 = DIRECTION ( 'NONE',  ( 0.000000000000000000, 1.131431318426415506E-52, 1.000000000000000000 ) ) ;
#1095 = VERTEX_POINT ( 'NONE', #3288 ) ;
#1096 = AXIS2_PLACEMENT_3D ( 'NONE', #14859, #9508, #17884 ) ;
#1097 = CARTESIAN_POINT ( 'NONE',  ( 105.0000000000000000, 0.000000000000000000, -57.49999999999999289 ) ) ;
#1098 = DIRECTION ( 'NONE',  ( 0.000000000000000000, 1.000000000000000000, 0.000000000000000000 ) ) ;
#1099 = EDGE_CURVE ( 'NONE', #12821, #24367, #15334, .T. ) ;
#1100 = EDGE_CURVE ( 'NONE', #17221, #31475, #28500, .T. ) ;
#1101 = VERTEX_POINT ( 'NONE', #8456 ) ;
#1102 = CARTESIAN_POINT ( 'NONE',  ( 9.199999999999999289, 7.794228634059941818, 13.49999999999999645 ) ) ;
#1103 = DIRECTION ( 'NONE',  ( 0.000000000000000000, 1.000000000000000000, 0.000000000000000000 ) ) ;
#1104 = EDGE_CURVE ( 'NONE', #20048, #7819, #2582, .T. ) ;
#1105 = CARTESIAN_POINT ( 'NONE',  ( -8.000000000000000000, 0.000000000000000000, 0.000000000000000000 ) ) ;
#1107 = CARTESIAN_POINT ( 'NONE',  ( -418.0000000000000000, 105.0000000000000000, -69.99999999999998579 ) ) ;
#1106 = CARTESIAN_POINT ( 'NONE',  ( 2.265105730852140287, 33.01038087096667084, 4.952322205615443451 ) ) ;
#1108 = AXIS2_PLACEMENT_3D ( 'NONE', #964, #6635, #11836 ) ;
#1109 = CARTESIAN_POINT ( 'NONE',  ( 19.99999999999998224, 134.9999999999998863, 187.0000000000000000 ) ) ;
#1110 = DIRECTION ( 'NONE',  ( -1.000000000000000000, 6.792721752314501023E-48, -3.697785493223492838E-32 ) ) ;
#1111 = ORIENTED_EDGE ( 'NONE', *, *, #27207, .F. ) ;
#1112 = FACE_OUTER_BOUND ( 'NONE', #12815, .T. ) ;
#1113 = FILL_AREA_STYLE_COLOUR ( '', #11550 ) ;
#1114 = MECHANICAL_DESIGN_GEOMETRIC_PRESENTATION_REPRESENTATION (  '', ( #28951 ), #30096 ) ;
#1115 = ORIENTED_EDGE ( 'NONE', *, *, #13293, .F. ) ;
#1116 = SHAPE_REPRESENTATION_RELATIONSHIP ( 'NONE' , 'NONE' ,  #34141, #15654 ) ;
#1117 = MANIFOLD_SOLID_BREP ( 'Trim/Extend7[2]', #17953 ) ;
#1118 = ORIENTED_EDGE ( 'NONE', *, *, #5241, .F. ) ;
#1119 = VECTOR ( 'NONE', #9651, 1000.000000000000000 ) ;
#1120 = EDGE_CURVE ( 'NONE', #3592, #3718, #32998, .T. ) ;
#1121 = EDGE_CURVE ( 'NONE', #18879, #2754, #13627, .T. ) ;
#1122 = ORIENTED_EDGE ( 'NONE', *, *, #12067, .F. ) ;
#1123 = DIRECTION ( 'NONE',  ( 0.000000000000000000, -1.000000000000000000, -1.541976423090495633E-16 ) ) ;
#1124 = ORIENTED_EDGE ( 'NONE', *, *, #19366, .T. ) ;
#1125 = VERTEX_POINT ( 'NONE', #275 ) ;
#1126 = CARTESIAN_POINT ( 'NONE',  ( 22.89764159710613001, 8.346743312457579833, -77.50000000000000000 ) ) ;
#1127 = EDGE_CURVE ( 'NONE', #13812, #701, #14617, .T. ) ;
#1128 = EDGE_CURVE ( 'NONE', #20858, #2088, #19713, .T. ) ;
#1129 = VECTOR ( 'NONE', #24012, 1000.000000000000000 ) ;
#1130 = VERTEX_POINT ( 'NONE', #8097 ) ;
#1131 = FACE_OUTER_BOUND ( 'NONE', #17761, .T. ) ;
#1132 = DIRECTION ( 'NONE',  ( 0.000000000000000000, 1.000000000000000000, 0.000000000000000000 ) ) ;
#1133 = EDGE_LOOP ( 'NONE', ( #18626, #22635, #27907, #4390 ) ) ;
#1134 = VERTEX_POINT ( 'NONE', #8277 ) ;
#1135 = DIRECTION ( 'NONE',  ( -1.000000000000000000, -0.000000000000000000, -0.000000000000000000 ) ) ;
#1136 = EDGE_CURVE ( 'NONE', #1031, #6516, #13984, .T. ) ;
#1137 = DIRECTION ( 'NONE',  ( 0.000000000000000000, 0.000000000000000000, 1.000000000000000000 ) ) ;
#1138 = CARTESIAN_POINT ( 'NONE',  ( 19.99999999999998934, 75.55999999999990280, 168.2400000000000091 ) ) ;
#1139 = FACE_OUTER_BOUND ( 'NONE', #18911, .T. ) ;
#1140 = FACE_OUTER_BOUND ( 'NONE', #5912, .T. ) ;
#1141 = ORIENTED_EDGE ( 'NONE', *, *, #31612, .T. ) ;
#1142 = DIRECTION ( 'NONE',  ( 1.000000000000000000, 0.000000000000000000, 0.000000000000000000 ) ) ;
#1143 = DIRECTION ( 'NONE',  ( -0.000000000000000000, 1.836970198721029934E-16, -1.000000000000000000 ) ) ;
#1144 = ADVANCED_FACE ( 'NONE', ( #8622 ), #16847, .T. ) ;
#1145 = DIRECTION ( 'NONE',  ( 0.000000000000000000, -1.000000000000000000, 6.123233995736766036E-17 ) ) ;
#1146 = ORIENTED_EDGE ( 'NONE', *, *, #20627, .F. ) ;
#1147 = CARTESIAN_POINT ( 'NONE',  ( -363.0000000000000000, -125.0000000000000284, 168.9999999999999716 ) ) ;
#1148 = DIRECTION ( 'NONE',  ( 1.000000000000000000, 0.000000000000000000, 0.000000000000000000 ) ) ;
#1149 = CARTESIAN_POINT ( 'NONE',  ( -130.6469666100234406, 6.000000000000000000, 62.49999999999999289 ) ) ;
#1150 = AXIS2_PLACEMENT_3D ( 'NONE', #6582, #33640, #25277 ) ;
#1151 = CARTESIAN_POINT ( 'NONE',  ( 104.2139989449238442, 5.687433884741868617, -4.889179432777876144 ) ) ;
#1153 = CARTESIAN_POINT ( 'NONE',  ( -45.00000000000000000, 16.36947364650383818, -36.69637551990492597 ) ) ;
#1152 = DIRECTION ( 'NONE',  ( -0.5155538571770220679, -0.8568571761675890519, 0.000000000000000000 ) ) ;
#1154 = VERTEX_POINT ( 'NONE', #20032 ) ;
#1155 = DIRECTION ( 'NONE',  ( 0.000000000000000000, 1.131431318426415506E-52, 1.000000000000000000 ) ) ;
#1157 = LINE ( 'NONE', #19859, #27644 ) ;
#1156 = CARTESIAN_POINT ( 'NONE',  ( -9.978866888775426602, 16.12922284503173742, -67.50000000000000000 ) ) ;
#1158 = ORIENTED_EDGE ( 'NONE', *, *, #23185, .T. ) ;
#1159 = CARTESIAN_POINT ( 'NONE',  ( 2.765921099433444219, 31.00221527374952046, 2.344426712874309260 ) ) ;
#1160 = ORIENTED_EDGE ( 'NONE', *, *, #15687, .T. ) ;
#1161 = EDGE_CURVE ( 'NONE', #29789, #12936, #20296, .T. ) ;
#1162 = ADVANCED_FACE ( 'NONE', ( #33539, #17379 ), #31058, .F. ) ;
#1163 = ORIENTED_EDGE ( 'NONE', *, *, #33703, .T. ) ;
#1164 = CARTESIAN_POINT ( 'NONE',  ( 99.46516806944471512, -1.563330414527343892, -7.345474502415979323 ) ) ;
#1165 = VERTEX_POINT ( 'NONE', #28559 ) ;
#1166 = ORIENTED_EDGE ( 'NONE', *, *, #4549, .T. ) ;
#1167 = CYLINDRICAL_SURFACE ( 'NONE', #24085, 2.000000000000001776 ) ;
#1168 = VECTOR ( 'NONE', #26116, 1000.000000000000000 ) ;
#1169 = CARTESIAN_POINT ( 'NONE',  ( -0.7181323043387224381, -1.866624223957557893, 5.429999999999999716 ) ) ;
#1170 = DIRECTION ( 'NONE',  ( 0.000000000000000000, 1.000000000000000000, -3.374343856708137958E-53 ) ) ;
#1171 = CYLINDRICAL_SURFACE ( 'NONE', #632, 7.999999999999979572 ) ;
#1172 = VERTEX_POINT ( 'NONE', #8805 ) ;
#1173 = ORIENTED_EDGE ( 'NONE', *, *, #31545, .T. ) ;
#1174 = CARTESIAN_POINT ( 'NONE',  ( -365.0000000000000000, -125.0000000000000000, 130.0000000000000000 ) ) ;
#1175 = CARTESIAN_POINT ( 'NONE',  ( -365.0000000000000000, 124.9999999999999432, 168.9999999999999716 ) ) ;
#1176 = DIRECTION ( 'NONE',  ( 1.000000000000000000, -0.000000000000000000, -0.000000000000000000 ) ) ;
#1177 = LINE ( 'NONE', #20748, #30629 ) ;
#1178 = FACE_OUTER_BOUND ( 'NONE', #24175, .T. ) ;
#1179 = FACE_BOUND ( 'NONE', #11958, .T. ) ;
#1180 = CIRCLE ( 'NONE', #15390, 4.750000000000004441 ) ;
#1181 = DIRECTION ( 'NONE',  ( 0.000000000000000000, 0.000000000000000000, 1.000000000000000000 ) ) ;
#1182 = ORIENTED_EDGE ( 'NONE', *, *, #5883, .F. ) ;
#1183 = AXIS2_PLACEMENT_3D ( 'NONE', #16487, #14473, #30162 ) ;
#1184 = DIRECTION ( 'NONE',  ( 0.000000000000000000, 0.000000000000000000, 1.000000000000000000 ) ) ;
#1185 = CARTESIAN_POINT ( 'NONE',  ( 1.040000000000000036, 31.89769921723006263, -12.91988538846923973 ) ) ;
#1186 = FACE_OUTER_BOUND ( 'NONE', #18294, .T. ) ;
#1187 = ORIENTED_EDGE ( 'NONE', *, *, #14083, .F. ) ;
#1188 = CYLINDRICAL_SURFACE ( 'NONE', #33151, 7.999999999999979572 ) ;
#1189 = EDGE_LOOP ( 'NONE', ( #29261, #25620, #10327, #29887 ) ) ;
#1190 = CIRCLE ( 'NONE', #33002, 3.999999999999976019 ) ;
#1191 =( NAMED_UNIT ( * ) SI_UNIT ( $, .STERADIAN. ) SOLID_ANGLE_UNIT ( ) );
#1192 = DIRECTION ( 'NONE',  ( 0.000000000000000000, 0.000000000000000000, 1.000000000000000000 ) ) ;
#1193 = VECTOR ( 'NONE', #14137, 1000.000000000000000 ) ;
#1194 = VERTEX_POINT ( 'NONE', #6123 ) ;
#1195 = SHAPE_REPRESENTATION ( 'short pitch roller chain wheel_s_iso_Chain wheel ISO - 25Z 05B-1 --25SA20.0S1', ( #28566 ), #10954 ) ;
#1196 = DIRECTION ( 'NONE',  ( 0.000000000000000000, -1.000000000000000000, 0.000000000000000000 ) ) ;
#1197 = DIRECTION ( 'NONE',  ( 0.000000000000000000, 1.836970198721029934E-16, -1.000000000000000000 ) ) ;
#1198 = CARTESIAN_POINT ( 'NONE',  ( 0.000000000000000000, 0.000000000000000000, -0.7500000000000000000 ) ) ;
#1199 = EDGE_CURVE ( 'NONE', #9586, #15011, #14704, .T. ) ;
#1200 = ORIENTED_EDGE ( 'NONE', *, *, #8308, .T. ) ;
#1201 = ADVANCED_FACE ( 'NONE', ( #800 ), #983, .T. ) ;
#1202 = AXIS2_PLACEMENT_3D ( 'NONE', #18750, #32418, #8038 ) ;
#1203 = DIRECTION ( 'NONE',  ( -7.894331716720217856E-14, 1.172479848580911511E-15, 1.000000000000000000 ) ) ;
#1204 = AXIS2_PLACEMENT_3D ( 'NONE', #9772, #34683, #18511 ) ;
#1205 = AXIS2_PLACEMENT_3D ( 'NONE', #9898, #1882, #15429 ) ;
#1206 = CARTESIAN_POINT ( 'NONE',  ( 2.789999999999999147, -29.91351748324099091, -5.799410679710938155 ) ) ;
#1207 = ADVANCED_FACE ( 'NONE', ( #28028 ), #11195, .T. ) ;
#1208 = ORIENTED_EDGE ( 'NONE', *, *, #8140, .F. ) ;
#1209 = DIRECTION ( 'NONE',  ( -0.000000000000000000, -0.000000000000000000, 1.000000000000000000 ) ) ;
#1210 = DIRECTION ( 'NONE',  ( 0.000000000000000000, 0.000000000000000000, 1.000000000000000000 ) ) ;
#1211 = CARTESIAN_POINT ( 'NONE',  ( -12.00000000000001066, -124.9999999999999432, -154.9999999999999716 ) ) ;
#1212 = DIRECTION ( 'NONE',  ( 0.000000000000000000, 0.000000000000000000, 1.000000000000000000 ) ) ;
#1213 = ITEM_DEFINED_TRANSFORMATION ( 'NONE', 'NONE', #24044,  #28566 ) ;
#1214 = VERTEX_POINT ( 'NONE', #1505 ) ;
#1215 = ORIENTED_EDGE ( 'NONE', *, *, #12710, .T. ) ;
#1216 = ORIENTED_EDGE ( 'NONE', *, *, #1754, .T. ) ;
#1217 = AXIS2_PLACEMENT_3D ( 'NONE', #8786, #19668, #24975 ) ;
#1218 = PRESENTATION_STYLE_ASSIGNMENT (( #22228 ) ) ;
#1220 = CARTESIAN_POINT ( 'NONE',  ( 0.2989565185775198697, 0.000000000000000000, 11.22499999999999787 ) ) ;
#1219 = AXIS2_PLACEMENT_3D ( 'NONE', #14763, #14936, #23289 ) ;
#1221 = CARTESIAN_POINT ( 'NONE',  ( 212.5000000000000000, 0.000000000000000000, 10.00000000000000000 ) ) ;
#1222 = CARTESIAN_POINT ( 'NONE',  ( 2.789999999999999147, 11.49079834592189897, 28.42701364291173149 ) ) ;
#1224 = CARTESIAN_POINT ( 'NONE',  ( 0.000000000000000000, 1.224646799147353256E-15, -10.00000000000000000 ) ) ;
#1223 =( REPRESENTATION_RELATIONSHIP ('NONE','NONE', #23037, #15767 ) REPRESENTATION_RELATIONSHIP_WITH_TRANSFORMATION ( #20994 )SHAPE_REPRESENTATION_RELATIONSHIP( ) );
#1225 = CYLINDRICAL_SURFACE ( 'NONE', #27765, 4.306175033202026547 ) ;
#1226 = VERTEX_POINT ( 'NONE', #12375 ) ;
#1227 = PRODUCT_DEFINITION_SHAPE ( 'NONE', 'NONE',  #35185 ) ;
#1228 = CYLINDRICAL_SURFACE ( 'NONE', #34024, 3.999999999999976019 ) ;
#1229 = CARTESIAN_POINT ( 'NONE',  ( 109.1843660233815996, 3.930740943550895761, 11.86668706373619386 ) ) ;
#1230 = ORIENTED_EDGE ( 'NONE', *, *, #16119, .T. ) ;
#1231 = CARTESIAN_POINT ( 'NONE',  ( 1.749999999999999778, -18.21166265554766994, -29.20140402659760070 ) ) ;
#1232 = VECTOR ( 'NONE', #14059, 1000.000000000000000 ) ;
#1233 = AXIS2_PLACEMENT_3D ( 'NONE', #17065, #502, #30744 ) ;
#1234 = CARTESIAN_POINT ( 'NONE',  ( -500.0000000000000000, -113.0000000000000000, 162.9999999999999716 ) ) ;
#1235 = VERTEX_POINT ( 'NONE', #11854 ) ;
#1236 = AXIS2_PLACEMENT_3D ( 'NONE', #2308, #29726, #32744 ) ;
#1237 = DIRECTION ( 'NONE',  ( -1.000000000000000000, -0.000000000000000000, -0.000000000000000000 ) ) ;
#1238 = CARTESIAN_POINT ( 'NONE',  ( 20.73027531293552528, -10.15143121711728469, 0.000000000000000000 ) ) ;
#1239 = CARTESIAN_POINT ( 'NONE',  ( -130.6469666100234406, -6.000000000000000000, 57.49999999999999289 ) ) ;
#1240 = CARTESIAN_POINT ( 'NONE',  ( -365.0000000000000000, -125.0000000000000284, 181.0000000000000000 ) ) ;
#1241 = DIRECTION ( 'NONE',  ( 1.000000000000000000, 0.000000000000000000, -0.000000000000000000 ) ) ;
#1242 = PLANE ( 'NONE',  #3525 ) ;
#1243 = EDGE_CURVE ( 'NONE', #14225, #17403, #32769, .T. ) ;
#1244 = ORIENTED_EDGE ( 'NONE', *, *, #5386, .F. ) ;
#1245 = CIRCLE ( 'NONE', #12552, 3.999999999999976019 ) ;
#1246 = VERTEX_POINT ( 'NONE', #33189 ) ;
#1247 = CARTESIAN_POINT ( 'NONE',  ( 776.7474300520071893, 1152.325823706140454, 1753.598338701303646 ) ) ;
#1248 = EDGE_CURVE ( 'NONE', #32323, #27667, #1157, .T. ) ;
#1249 = ORIENTED_EDGE ( 'NONE', *, *, #11405, .T. ) ;
#1250 = EDGE_CURVE ( 'NONE', #2295, #22708, #31023, .T. ) ;
#1251 = CARTESIAN_POINT ( 'NONE',  ( 2.033800793502754445, 13.95859842408627038, 30.90949138205576219 ) ) ;
#1252 = AXIS2_PLACEMENT_3D ( 'NONE', #26130, #7779, #13322 ) ;
#1253 = EDGE_CURVE ( 'NONE', #22184, #6749, #4918, .T. ) ;
#1254 = DIRECTION ( 'NONE',  ( -1.000000000000000000, -0.000000000000000000, -0.000000000000000000 ) ) ;
#1255 = ADVANCED_FACE ( 'NONE', ( #27847 ), #16878, .T. ) ;
#1256 = CONTEXT_DEPENDENT_SHAPE_REPRESENTATION ( #27824, #4092 ) ;
#1257 = CIRCLE ( 'NONE', #25693, 2.000000000000001776 ) ;
#1258 = ORIENTED_EDGE ( 'NONE', *, *, #33383, .F. ) ;
#1259 = VECTOR ( 'NONE', #25566, 1000.000000000000000 ) ;
#1260 = CARTESIAN_POINT ( 'NONE',  ( -442.0000000000000000, 104.9999999999999858, -194.9999999999999716 ) ) ;
#1261 = CARTESIAN_POINT ( 'NONE',  ( -101.8768327269408189, -4.064293880962482675, -11.82242856119474439 ) ) ;
#1262 = EDGE_CURVE ( 'NONE', #12124, #6786, #12904, .T. ) ;
#1264 = CARTESIAN_POINT ( 'NONE',  ( -499.9999999999999432, 136.9999999999999432, 159.0000000000000000 ) ) ;
#1263 = DIRECTION ( 'NONE',  ( 1.000000000000000000, 0.000000000000000000, 0.000000000000000000 ) ) ;
#1265 = ORIENTED_EDGE ( 'NONE', *, *, #24062, .T. ) ;
#1266 = ORIENTED_EDGE ( 'NONE', *, *, #34069, .F. ) ;
#1267 = DIRECTION ( 'NONE',  ( 0.000000000000000000, 1.836970198721029441E-16, -1.000000000000000000 ) ) ;
#1268 = DIRECTION ( 'NONE',  ( 0.000000000000000000, 1.000000000000000000, 1.836970198721029688E-16 ) ) ;
#1269 = DIRECTION ( 'NONE',  ( -0.000000000000000000, 1.836970198721029688E-16, -1.000000000000000000 ) ) ;
#1270 = ORIENTED_EDGE ( 'NONE', *, *, #9403, .T. ) ;
#1271 = DIRECTION ( 'NONE',  ( 0.000000000000000000, -1.000000000000000000, 0.000000000000000000 ) ) ;
#1272 = DIRECTION ( 'NONE',  ( 1.000000000000000000, 0.000000000000000000, 0.000000000000000000 ) ) ;
#1273 =( REPRESENTATION_RELATIONSHIP ('NONE','NONE', #23037, #28231 ) REPRESENTATION_RELATIONSHIP_WITH_TRANSFORMATION ( #8732 )SHAPE_REPRESENTATION_RELATIONSHIP( ) );
#1274 = ORIENTED_EDGE ( 'NONE', *, *, #32043, .F. ) ;
#1275 = DIRECTION ( 'NONE',  ( 0.000000000000000000, 1.836970198721029688E-16, -1.000000000000000000 ) ) ;
#1276 = CARTESIAN_POINT ( 'NONE',  ( -32.32899628990713126, -3.747048406849335045, -36.68877005347593467 ) ) ;
#1277 = CARTESIAN_POINT ( 'NONE',  ( 0.5248942285756895698, 33.20489141755878393, 3.412611943275336124 ) ) ;
#1280 = DIRECTION ( 'NONE',  ( 0.000000000000000000, 1.000000000000000000, 0.000000000000000000 ) ) ;
#1279 = DIRECTION ( 'NONE',  ( 0.000000000000000000, 0.000000000000000000, -1.000000000000000000 ) ) ;
#1278 = VECTOR ( 'NONE', #1030, 1000.000000000000000 ) ;
#1281 = AXIS2_PLACEMENT_3D ( 'NONE', #20582, #12757, #15597 ) ;
#1282 = AXIS2_PLACEMENT_3D ( 'NONE', #25350, #982, #13983 ) ;
#1283 = LINE ( 'NONE', #12153, #22975 ) ;
#1284 = CYLINDRICAL_SURFACE ( 'NONE', #1183, 2.524999999999999467 ) ;
#1285 = EDGE_LOOP ( 'NONE', ( #25859, #17008, #10345, #31825 ) ) ;
#1286 = B_SPLINE_CURVE_WITH_KNOTS ( 'NONE', 3,
 ( #7807, #32013, #34519, #18000 ),
 .UNSPECIFIED., .F., .F.,
 ( 4, 4 ),
 ( 0.005298345749243330016, 0.005985214453301815341 ),
 .UNSPECIFIED. ) ;
#1287 = FACE_OUTER_BOUND ( 'NONE', #34679, .T. ) ;
#1288 = CARTESIAN_POINT ( 'NONE',  ( 0.8377008405913606293, -14.95094041744786928, 1.104211576045298404 ) ) ;
#1289 = ORIENTED_EDGE ( 'NONE', *, *, #2239, .T. ) ;
#1290 = VERTEX_POINT ( 'NONE', #12025 ) ;
#1291 = ORIENTED_EDGE ( 'NONE', *, *, #6612, .T. ) ;
#1292 = EDGE_CURVE ( 'NONE', #7906, #11190, #17556, .T. ) ;
#1293 = FACE_OUTER_BOUND ( 'NONE', #25940, .T. ) ;
#1294 = EDGE_CURVE ( 'NONE', #23520, #30318, #7681, .T. ) ;
#1295 = ORIENTED_EDGE ( 'NONE', *, *, #18930, .T. ) ;
#1296 = VERTEX_POINT ( 'NONE', #3457 ) ;
#1297 = ORIENTED_EDGE ( 'NONE', *, *, #33193, .F. ) ;
#1298 = CARTESIAN_POINT ( 'NONE',  ( -349.0000000000000000, -125.0000000000000284, 183.0000000000000000 ) ) ;
#1300 = AXIS2_PLACEMENT_3D ( 'NONE', #30263, #5863, #6215 ) ;
#1299 = ITEM_DEFINED_TRANSFORMATION ( 'NONE', 'NONE', #13852,  #28566 ) ;
#1301 = ORIENTED_EDGE ( 'NONE', *, *, #28459, .F. ) ;
#1302 = CARTESIAN_POINT ( 'NONE',  ( 2.789999999999999147, -23.41952779159776199, 19.49300927180536291 ) ) ;
#1303 = AXIS2_PLACEMENT_3D ( 'NONE', #31389, #29379, #10696 ) ;
#1304 = DIRECTION ( 'NONE',  ( -1.000000000000000000, 0.000000000000000000, -0.000000000000000000 ) ) ;
#1305 = VERTEX_POINT ( 'NONE', #14347 ) ;
#1306 = AXIS2_PLACEMENT_3D ( 'NONE', #10338, #21198, #18723 ) ;
#1307 = EDGE_LOOP ( 'NONE', ( #15407, #21157, #27983, #5723, #28927, #18871 ) ) ;
#1308 = AXIS2_PLACEMENT_3D ( 'NONE', #23598, #4889, #7035 ) ;
#1309 = DIRECTION ( 'NONE',  ( -0.000000000000000000, -0.000000000000000000, -1.000000000000000000 ) ) ;
#1310 = DIRECTION ( 'NONE',  ( 1.000000000000000000, 0.000000000000000000, -0.000000000000000000 ) ) ;
#1311 = CARTESIAN_POINT ( 'NONE',  ( 11.99999999999999645, 124.9999999999999716, 159.0000000000000000 ) ) ;
#1313 = EDGE_CURVE ( 'NONE', #292, #9463, #11107, .T. ) ;
#1312 = CARTESIAN_POINT ( 'NONE',  ( 5.021133111224162171, -21.54630831098063837, -67.50000000000000000 ) ) ;
#1314 = DIRECTION ( 'NONE',  ( 1.000000000000000000, 0.000000000000000000, 0.000000000000000000 ) ) ;
#1315 = VERTEX_POINT ( 'NONE', #22523 ) ;
#1316 = CARTESIAN_POINT ( 'NONE',  ( 0.000000000000000000, 6.992329373473909019E-15, 49.43553178847298568 ) ) ;
#1317 = CARTESIAN_POINT ( 'NONE',  ( -430.0000000000000000, 134.9999999999999716, 113.9999999999999858 ) ) ;
#1318 = CARTESIAN_POINT ( 'NONE',  ( -355.0000000000000000, -133.0000000000000000, 126.0000000000000000 ) ) ;
#1319 = ORIENTED_EDGE ( 'NONE', *, *, #1542, .F. ) ;
#1320 = CARTESIAN_POINT ( 'NONE',  ( -449.9999999999999432, 137.0000000000000000, 154.9999999999999716 ) ) ;
#1322 = ADVANCED_FACE ( 'NONE', ( #2195 ), #1844, .T. ) ;
#1321 = CARTESIAN_POINT ( 'NONE',  ( 145.0000000000000568, -97.56119630548165844, -180.0000000000000000 ) ) ;
#1323 = DIRECTION ( 'NONE',  ( 0.000000000000000000, 1.000000000000000000, 0.000000000000000000 ) ) ;
#1324 = ADVANCED_FACE ( 'NONE', ( #2364 ), #23223, .T. ) ;
#1325 = CYLINDRICAL_SURFACE ( 'NONE', #28033, 4.682234377621698584 ) ;
#1326 = CARTESIAN_POINT ( 'NONE',  ( -6.500000000000000000, 0.000000000000000000, 4.679999999999999716 ) ) ;
#1327 = ADVANCED_FACE ( 'NONE', ( #34422 ), #4667, .F. ) ;
#1328 = AXIS2_PLACEMENT_3D ( 'NONE', #32076, #7695, #24061 ) ;
#1329 = DIRECTION ( 'NONE',  ( -1.000000000000000000, 0.000000000000000000, 0.000000000000000000 ) ) ;
#1330 = ORIENTED_EDGE ( 'NONE', *, *, #22566, .F. ) ;
#1331 = DIRECTION ( 'NONE',  ( 0.000000000000000000, 3.374343856708137958E-53, -1.000000000000000000 ) ) ;
#1333 = CARTESIAN_POINT ( 'NONE',  ( 0.000000000000000000, -20.35927063852789232, -24.61013060777193218 ) ) ;
#1332 = DIRECTION ( 'NONE',  ( 1.000000000000000000, 0.000000000000000000, 0.000000000000000000 ) ) ;
#1334 = EDGE_CURVE ( 'NONE', #13964, #33838, #28902, .T. ) ;
#1335 = AXIS2_PLACEMENT_3D ( 'NONE', #31486, #28644, #1423 ) ;
#1337 = VERTEX_POINT ( 'NONE', #20892 ) ;
#1336 = AXIS2_PLACEMENT_3D ( 'NONE', #1879, #2063, #34282 ) ;
#1338 = AXIS2_PLACEMENT_3D ( 'NONE', #14468, #8753, #12149 ) ;
#1339 = DIRECTION ( 'NONE',  ( 0.000000000000000000, 0.000000000000000000, 1.000000000000000000 ) ) ;
#1340 = VERTEX_POINT ( 'NONE', #32088 ) ;
#1341 = B_SPLINE_CURVE_WITH_KNOTS ( 'NONE', 3,
 ( #18800, #8455, #21987, #19157 ),
 .UNSPECIFIED., .F., .F.,
 ( 4, 4 ),
 ( 0.005298347253562356134, 0.005985215922708608631 ),
 .UNSPECIFIED. ) ;
#1342 = EDGE_CURVE ( 'NONE', #7970, #11639, #23738, .T. ) ;
#1343 = ORIENTED_EDGE ( 'NONE', *, *, #33236, .F. ) ;
#1344 = CARTESIAN_POINT ( 'NONE',  ( 99.58236139071918558, -1.928835813323004800, -7.257044673176061167 ) ) ;
#1345 = ORIENTED_EDGE ( 'NONE', *, *, #882, .F. ) ;
#1346 = ORIENTED_EDGE ( 'NONE', *, *, #16683, .F. ) ;
#1347 = CARTESIAN_POINT ( 'NONE',  ( 0.000000000000000000, 0.000000000000000000, 0.000000000000000000 ) ) ;
#1348 = CARTESIAN_POINT ( 'NONE',  ( 0.02407890056655738464, -11.07880054387241664, 29.04985141099759360 ) ) ;
#1349 = CIRCLE ( 'NONE', #21810, 3.999999999999948042 ) ;
#1350 = CARTESIAN_POINT ( 'NONE',  ( -418.0000000000000000, -105.0000000000000142, 187.0000000000000000 ) ) ;
#1351 = CARTESIAN_POINT ( 'NONE',  ( 0.000000000000000000, 0.000000000000000000, 0.000000000000000000 ) ) ;
#1352 = ORIENTED_EDGE ( 'NONE', *, *, #31784, .F. ) ;
#1353 = EDGE_LOOP ( 'NONE', ( #34446, #22061, #26302, #9004 ) ) ;
#1354 = CARTESIAN_POINT ( 'NONE',  ( -445.9999999999999432, -105.0000000000000142, 162.9999999999999716 ) ) ;
#1355 = CARTESIAN_POINT ( 'NONE',  ( -20.00000000000007461, 136.9999999999999432, -190.9999999999999716 ) ) ;
#1356 = CARTESIAN_POINT ( 'NONE',  ( 13.32059394339353986, -35.43959265050634144, 68.31122994652405112 ) ) ;
#1357 = CARTESIAN_POINT ( 'NONE',  ( -35.00000000000000000, -12.29554237047778997, 68.31122994652405112 ) ) ;
#1358 = DIRECTION ( 'NONE',  ( 0.000000000000000000, 0.000000000000000000, 1.000000000000000000 ) ) ;
#1359 = AXIS2_PLACEMENT_3D ( 'NONE', #15799, #29485, #34829 ) ;
#1360 = CARTESIAN_POINT ( 'NONE',  ( -418.0000000000000000, 105.0000000000000142, 100.0000000000000000 ) ) ;
#1361 = AXIS2_PLACEMENT_3D ( 'NONE', #8984, #1501, #28384 ) ;
#1362 = VECTOR ( 'NONE', #25435, 1000.000000000000000 ) ;
#1363 = DIRECTION ( 'NONE',  ( -0.7960930657056428661, 0.6051742151937663516, -0.000000000000000000 ) ) ;
#1364 = VERTEX_POINT ( 'NONE', #34776 ) ;
#1365 = FACE_OUTER_BOUND ( 'NONE', #7788, .T. ) ;
#1366 = CARTESIAN_POINT ( 'NONE',  ( 2.783107601403548959, -11.06505884892056102, 28.81855237217592958 ) ) ;
#1367 = EDGE_CURVE ( 'NONE', #30447, #11932, #26058, .T. ) ;
#1368 = CARTESIAN_POINT ( 'NONE',  ( 26.04754872656010889, -19.51229300245305964, 68.31122994652405112 ) ) ;
#1369 = ORIENTED_EDGE ( 'NONE', *, *, #2507, .F. ) ;
#1370 = EDGE_CURVE ( 'NONE', #20728, #13531, #12820, .T. ) ;
#1371 = CARTESIAN_POINT ( 'NONE',  ( 2.789999999999999147, 0.000000000000000000, 0.000000000000000000 ) ) ;
#1372 = ORIENTED_EDGE ( 'NONE', *, *, #9870, .F. ) ;
#1373 = DIRECTION ( 'NONE',  ( 0.000000000000000000, 0.000000000000000000, -1.000000000000000000 ) ) ;
#1374 = CARTESIAN_POINT ( 'NONE',  ( -109.4269239543884851, 2.567831768330360642, 12.23432884111322316 ) ) ;
#1375 = VECTOR ( 'NONE', #18478, 1000.000000000000000 ) ;
#1376 = VERTEX_POINT ( 'NONE', #2023 ) ;
#1377 = DIRECTION ( 'NONE',  ( -1.000000000000000000, 0.000000000000000000, 0.000000000000000000 ) ) ;
#1378 = DIRECTION ( 'NONE',  ( 1.000000000000000000, 0.000000000000000000, -1.232595164407831220E-32 ) ) ;
#1379 = ORIENTED_EDGE ( 'NONE', *, *, #10516, .F. ) ;
#1380 = ORIENTED_EDGE ( 'NONE', *, *, #5701, .T. ) ;
#1381 = VECTOR ( 'NONE', #8053, 1000.000000000000000 ) ;
#1382 = CARTESIAN_POINT ( 'NONE',  ( 854.7149863358548600, 983.4033156899278083, 1753.598338701302964 ) ) ;
#1383 = CARTESIAN_POINT ( 'NONE',  ( 5.021133111224369117, -3.725253662474303784, -67.50000000000000000 ) ) ;
#1384 = ORIENTED_EDGE ( 'NONE', *, *, #16115, .T. ) ;
#1385 = CARTESIAN_POINT ( 'NONE',  ( 15.99999999999998579, 124.9999999999999716, 162.9999999999999716 ) ) ;
#1386 = VECTOR ( 'NONE', #1768, 1000.000000000000000 ) ;
#1387 = FACE_OUTER_BOUND ( 'NONE', #26140, .T. ) ;
#1388 = LINE ( 'NONE', #25763, #25846 ) ;
#1389 = CARTESIAN_POINT ( 'NONE',  ( 2.789999999999999147, 30.11551674275779433, 4.430359003076457469 ) ) ;
#1390 = ITEM_DEFINED_TRANSFORMATION ( 'NONE', 'NONE', #7004,  #28566 ) ;
#1391 = ORIENTED_EDGE ( 'NONE', *, *, #25706, .F. ) ;
#1392 = ORIENTED_EDGE ( 'NONE', *, *, #20061, .F. ) ;
#1393 = ORIENTED_EDGE ( 'NONE', *, *, #33177, .F. ) ;
#1394 = EDGE_CURVE ( 'NONE', #10216, #12264, #31736, .T. ) ;
#1395 = CARTESIAN_POINT ( 'NONE',  ( 2.783128933731652488, 23.98851302352063897, -19.42881381898143545 ) ) ;
#1396 = PLANE ( 'NONE',  #30792 ) ;
#1397 = DIRECTION ( 'NONE',  ( 3.469446951953832974E-18, 1.000000000000000000, 7.888609052210116302E-31 ) ) ;
#1398 = FACE_OUTER_BOUND ( 'NONE', #17490, .T. ) ;
#1399 = DIRECTION ( 'NONE',  ( 0.000000000000000000, 0.000000000000000000, 1.000000000000000000 ) ) ;
#1400 = FACE_OUTER_BOUND ( 'NONE', #34513, .T. ) ;
#1401 = ORIENTED_EDGE ( 'NONE', *, *, #25136, .T. ) ;
#1402 = VECTOR ( 'NONE', #25282, 1000.000000000000000 ) ;
#1403 = ADVANCED_FACE ( 'NONE', ( #7003 ), #23561, .T. ) ;
#1404 = CARTESIAN_POINT ( 'NONE',  ( 0.5288002438369178160, 20.68324032934645018, 26.21226347405753998 ) ) ;
#1405 = EDGE_CURVE ( 'NONE', #18566, #13343, #4853, .T. ) ;
#1406 = ORIENTED_EDGE ( 'NONE', *, *, #28646, .F. ) ;
#1407 = DIRECTION ( 'NONE',  ( 0.000000000000000000, 0.000000000000000000, 1.000000000000000000 ) ) ;
#1408 = EDGE_CURVE ( 'NONE', #14065, #34278, #9467, .T. ) ;
#1409 = AXIS2_PLACEMENT_3D ( 'NONE', #21590, #27624, #30295 ) ;
#1410 = CIRCLE ( 'NONE', #825, 2.000000000000001776 ) ;
#1411 = CARTESIAN_POINT ( 'NONE',  ( 212.5000000000000000, 0.000000000000000000, 0.000000000000000000 ) ) ;
#1412 = ORIENTED_EDGE ( 'NONE', *, *, #19543, .F. ) ;
#1413 = EDGE_CURVE ( 'NONE', #19123, #17691, #15746, .T. ) ;
#1414 = DIRECTION ( 'NONE',  ( -1.000000000000000000, 0.000000000000000000, -5.546364386991661285E-52 ) ) ;
#1415 = CARTESIAN_POINT ( 'NONE',  ( 99.26191511054632599, 0.000000000000000000, 57.49999999999999289 ) ) ;
#1416 = CARTESIAN_POINT ( 'NONE',  ( -442.0000000000000000, -104.9999999999999858, -162.9999999999999716 ) ) ;
#1417 = CARTESIAN_POINT ( 'NONE',  ( -35.55956070192387841, -32.65143121711728469, 14.30932821646982411 ) ) ;
#1418 = UNCERTAINTY_MEASURE_WITH_UNIT (LENGTH_MEASURE( 1.000000000000000082E-05 ), #3776, 'distance_accuracy_value', 'NONE');
#1419 = CARTESIAN_POINT ( 'NONE',  ( -349.0000000000000000, -125.0000000000000284, 185.0000000000000000 ) ) ;
#1420 = ORIENTED_EDGE ( 'NONE', *, *, #11174, .F. ) ;
#1421 = VECTOR ( 'NONE', #19434, 1000.000000000000000 ) ;
#1422 = ORIENTED_EDGE ( 'NONE', *, *, #4993, .T. ) ;
#1423 = DIRECTION ( 'NONE',  ( -0.1063910735369017202, 0.9943243633099136947, -1.000770725407181676E-14 ) ) ;
#1424 = ORIENTED_EDGE ( 'NONE', *, *, #6964, .T. ) ;
#1425 = DIRECTION ( 'NONE',  ( -1.000000000000000000, 6.792721752314501023E-48, -3.697785493223492838E-32 ) ) ;
#1426 = VECTOR ( 'NONE', #28156, 1000.000000000000000 ) ;
#1427 = DIRECTION ( 'NONE',  ( 1.000000000000000000, 0.000000000000000000, 0.000000000000000000 ) ) ;
#1428 = CONTEXT_DEPENDENT_SHAPE_REPRESENTATION ( #20554, #17499 ) ;
#1429 = AXIS2_PLACEMENT_3D ( 'NONE', #14786, #26313, #23469 ) ;
#1430 = ORIENTED_EDGE ( 'NONE', *, *, #9780, .F. ) ;
#1431 = CARTESIAN_POINT ( 'NONE',  ( 24.11848021413632992, 29.19488569250028220, 68.31122994652405112 ) ) ;
#1432 = DIRECTION ( 'NONE',  ( -1.000000000000000000, 0.000000000000000000, -1.300283923313630633E-47 ) ) ;
#1434 = CARTESIAN_POINT ( 'NONE',  ( -35.00000000000000000, 3.353962854566122864, -15.81122994652406355 ) ) ;
#1433 = CARTESIAN_POINT ( 'NONE',  ( -6.500000000000000000, 0.000000000000000000, -0.7500000000000000000 ) ) ;
#1435 = ORIENTED_EDGE ( 'NONE', *, *, #66, .T. ) ;
#1436 = ORIENTED_EDGE ( 'NONE', *, *, #15716, .T. ) ;
#1437 = DIRECTION ( 'NONE',  ( -1.000000000000000000, -3.469446951953834515E-18, 0.000000000000000000 ) ) ;
#1438 = EDGE_CURVE ( 'NONE', #17376, #31755, #29433, .T. ) ;
#1439 = EDGE_CURVE ( 'NONE', #23165, #2399, #29356, .T. ) ;
#1440 = CARTESIAN_POINT ( 'NONE',  ( 5.713835024271039842, 32.03991982186465748, 68.31122994652405112 ) ) ;
#1441 = DIRECTION ( 'NONE',  ( 0.000000000000000000, 1.000000000000000000, 0.000000000000000000 ) ) ;
#1442 = ORIENTED_EDGE ( 'NONE', *, *, #2873, .F. ) ;
#1443 = VECTOR ( 'NONE', #16868, 1000.000000000000000 ) ;
#1444 = DIRECTION ( 'NONE',  ( -0.1081190184239417262, -0.9941379571543595972, 0.000000000000000000 ) ) ;
#1445 = VECTOR ( 'NONE', #24810, 1000.000000000000227 ) ;
#1446 = ORIENTED_EDGE ( 'NONE', *, *, #32975, .T. ) ;
#1447 = EDGE_CURVE ( 'NONE', #11922, #29621, #20724, .T. ) ;
#1448 = CIRCLE ( 'NONE', #28152, 3.999999999999976019 ) ;
#1449 = FACE_OUTER_BOUND ( 'NONE', #28871, .T. ) ;
#1450 = DIRECTION ( 'NONE',  ( -1.000000000000000000, 0.000000000000000000, 0.000000000000000000 ) ) ;
#1451 = DIRECTION ( 'NONE',  ( 0.000000000000000000, 0.000000000000000000, -1.000000000000000000 ) ) ;
#1453 = DIRECTION ( 'NONE',  ( 1.000000000000000000, -0.000000000000000000, -0.000000000000000000 ) ) ;
#1452 = CARTESIAN_POINT ( 'NONE',  ( 29.44023756548696369, 13.87360028845404969, 68.31122994652405112 ) ) ;
#1454 = ADVANCED_FACE ( 'NONE', ( #13767, #18767, #5385 ), #5722, .F. ) ;
#1455 = AXIS2_PLACEMENT_3D ( 'NONE', #33240, #1029, #22384 ) ;
#1456 = DIRECTION ( 'NONE',  ( -3.040835319149746528E-31, -1.000000000000000000, 0.000000000000000000 ) ) ;
#1457 = DIRECTION ( 'NONE',  ( 1.000000000000000000, 0.000000000000000000, 0.000000000000000000 ) ) ;
#1458 = ORIENTED_EDGE ( 'NONE', *, *, #6369, .F. ) ;
#1459 = CARTESIAN_POINT ( 'NONE',  ( 1.749999999999999778, -10.37741591188871482, -32.81304455236878681 ) ) ;
#1460 = PRESENTATION_STYLE_ASSIGNMENT (( #25834 ) ) ;
#1461 = AXIS2_PLACEMENT_3D ( 'NONE', #27978, #24945, #19458 ) ;
#1462 = EDGE_CURVE ( 'NONE', #30062, #4232, #230, .T. ) ;
#1463 = EDGE_CURVE ( 'NONE', #1478, #31329, #13244, .T. ) ;
#1464 = ORIENTED_EDGE ( 'NONE', *, *, #2512, .T. ) ;
#1465 = ORIENTED_EDGE ( 'NONE', *, *, #5762, .F. ) ;
#1466 = CIRCLE ( 'NONE', #5996, 34.41491905851385269 ) ;
#1467 = CARTESIAN_POINT ( 'NONE',  ( 0.006871098824289784829, 18.40312061469623472, 24.78412275958840283 ) ) ;
#1468 = ORIENTED_EDGE ( 'NONE', *, *, #27241, .T. ) ;
#1469 = VERTEX_POINT ( 'NONE', #11098 ) ;
#1470 = ORIENTED_EDGE ( 'NONE', *, *, #32484, .T. ) ;
#1471 = DIRECTION ( 'NONE',  ( -1.000000000000000000, 0.000000000000000000, 0.000000000000000000 ) ) ;
#1472 = VECTOR ( 'NONE', #15375, 1000.000000000000000 ) ;
#1473 = ITEM_DEFINED_TRANSFORMATION ( 'NONE', 'NONE', #22956,  #28566 ) ;
#1474 = ORIENTED_EDGE ( 'NONE', *, *, #5517, .F. ) ;
#1475 = DIRECTION ( 'NONE',  ( 1.000000000000000000, 0.000000000000000000, 0.000000000000000000 ) ) ;
#1476 = DIRECTION ( 'NONE',  ( -1.000000000000000000, -0.000000000000000000, -0.000000000000000000 ) ) ;
#1477 = ORIENTED_EDGE ( 'NONE', *, *, #32189, .F. ) ;
#1478 = VERTEX_POINT ( 'NONE', #19120 ) ;
#1479 =( REPRESENTATION_RELATIONSHIP ('NONE','NONE', #23037, #15767 ) REPRESENTATION_RELATIONSHIP_WITH_TRANSFORMATION ( #34301 )SHAPE_REPRESENTATION_RELATIONSHIP( ) );
#1480 = CARTESIAN_POINT ( 'NONE',  ( 10.00000000000000000, 1.653273178848927064E-15, -13.50000000000000178 ) ) ;
#1481 = LINE ( 'NONE', #23362, #3323 ) ;
#1482 = VECTOR ( 'NONE', #26705, 1000.000000000000000 ) ;
#1483 = CARTESIAN_POINT ( 'NONE',  ( -19.99999999999998934, 4.559999999999908127, 168.2400000000000091 ) ) ;
#1484 = DIRECTION ( 'NONE',  ( -0.000000000000000000, -0.000000000000000000, -1.000000000000000000 ) ) ;
#1485 = CARTESIAN_POINT ( 'NONE',  ( 22.89764159710611224, 13.56412600238610366, -77.50000000000000000 ) ) ;
#1486 = VERTEX_POINT ( 'NONE', #16272 ) ;
#1487 = CARTESIAN_POINT ( 'NONE',  ( -12.00000000000001066, 124.9999999999999716, 155.0000000000000000 ) ) ;
#1489 = CIRCLE ( 'NONE', #19689, 3.999999999999976019 ) ;
#1488 = PLANE ( 'NONE',  #19097 ) ;
#1490 = CARTESIAN_POINT ( 'NONE',  ( 1.749999999999999778, 14.89726405156260469, -31.02351007835961383 ) ) ;
#1491 = ORIENTED_EDGE ( 'NONE', *, *, #27268, .T. ) ;
#1492 = DIRECTION ( 'NONE',  ( 0.000000000000000000, 0.000000000000000000, -1.000000000000000000 ) ) ;
#1493 = DIRECTION ( 'NONE',  ( 0.000000000000000000, 0.000000000000000000, 1.000000000000000000 ) ) ;
#1494 = DIRECTION ( 'NONE',  ( -1.000000000000000000, 0.000000000000000000, 0.000000000000000000 ) ) ;
#1495 = EDGE_CURVE ( 'NONE', #13296, #6161, #27458, .T. ) ;
#1496 = CARTESIAN_POINT ( 'NONE',  ( -20.00000000000007461, -113.0000000000000000, -162.9999999999999716 ) ) ;
#1498 = PLANE ( 'NONE',  #16806 ) ;
#1497 = FACE_OUTER_BOUND ( 'NONE', #34932, .T. ) ;
#1499 = ADVANCED_FACE ( 'NONE', ( #10571 ), #13591, .F. ) ;
#1500 = ADVANCED_FACE ( 'NONE', ( #24072 ), #21425, .T. ) ;
#1501 = DIRECTION ( 'NONE',  ( 0.000000000000000000, 0.000000000000000000, 1.000000000000000000 ) ) ;
#1502 = ORIENTED_EDGE ( 'NONE', *, *, #9274, .F. ) ;
#1503 = CARTESIAN_POINT ( 'NONE',  ( 1.649999999999999911, 2.020667218593132262E-16, 3.180000000000000160 ) ) ;
#1505 = CARTESIAN_POINT ( 'NONE',  ( -19.99999999999998934, -112.9999999999999858, 155.0000000000000000 ) ) ;
#1504 = DIRECTION ( 'NONE',  ( 0.7960930657056439763, -0.6051742151937649083, -1.111686998345333706E-16 ) ) ;
#1506 = ORIENTED_EDGE ( 'NONE', *, *, #19153, .T. ) ;
#1507 = CARTESIAN_POINT ( 'NONE',  ( -20.00000000000001776, -137.0000000000000000, -154.9999999999999716 ) ) ;
#1508 = AXIS2_PLACEMENT_3D ( 'NONE', #34955, #16626, #13943 ) ;
#1509 = ORIENTED_EDGE ( 'NONE', *, *, #24538, .T. ) ;
#1510 = EDGE_CURVE ( 'NONE', #24976, #16592, #18747, .T. ) ;
#1511 = B_SPLINE_CURVE_WITH_KNOTS ( 'NONE', 3,
 ( #13514, #35058, #32364, #29704 ),
 .UNSPECIFIED., .F., .F.,
 ( 4, 4 ),
 ( 0.0006242955995025980349, 0.0006879396046782833979 ),
 .UNSPECIFIED. ) ;
#1512 = ORIENTED_EDGE ( 'NONE', *, *, #16791, .T. ) ;
#1513 = CARTESIAN_POINT ( 'NONE',  ( 99.26191511054628336, -0.3983872338823410408, -7.499999999999998224 ) ) ;
#1514 = ORIENTED_EDGE ( 'NONE', *, *, #9603, .F. ) ;
#1515 = ORIENTED_EDGE ( 'NONE', *, *, #30287, .F. ) ;
#1516 = CARTESIAN_POINT ( 'NONE',  ( 19.99999999999998224, -115.0000000000000000, -158.9999999999999716 ) ) ;
#1517 = PRODUCT_DEFINITION_SHAPE ( 'NONE', 'NONE',  #35158 ) ;
#1518 = EDGE_CURVE ( 'NONE', #32367, #19566, #21944, .T. ) ;
#1519 = CARTESIAN_POINT ( 'NONE',  ( 0.5288002590931849545, -11.04911166161968161, 31.50867056184614867 ) ) ;
#1520 = ADVANCED_FACE ( 'NONE', ( #29958, #16092 ), #2544, .T. ) ;
#1521 = AXIS2_PLACEMENT_3D ( 'NONE', #13047, #32065, #5357 ) ;
#1522 = B_SPLINE_CURVE_WITH_KNOTS ( 'NONE', 3,
 ( #218, #30393, #18920, #10736, #5365, #5537 ),
 .UNSPECIFIED., .F., .F.,
 ( 4, 2, 4 ),
 ( 4.404817001457452636E-07, 0.001874269605587669443, 0.003748098729475193413 ),
 .UNSPECIFIED. ) ;
#1524 = EDGE_CURVE ( 'NONE', #14561, #13528, #33154, .T. ) ;
#1523 = CARTESIAN_POINT ( 'NONE',  ( -45.00000000000000000, -46.95407462254104303, -36.69637551990492597 ) ) ;
#1525 = CARTESIAN_POINT ( 'NONE',  ( -5.021133111224782120, 18.16264470403145381, -87.50000000000000000 ) ) ;
#1526 = EDGE_LOOP ( 'NONE', ( #14624, #22210, #8293, #29863 ) ) ;
#1527 = ORIENTED_EDGE ( 'NONE', *, *, #26835, .F. ) ;
#1528 = LINE ( 'NONE', #26245, #13393 ) ;
#1529 = DIRECTION ( 'NONE',  ( -1.292961597001347186E-16, 0.000000000000000000, 1.000000000000000000 ) ) ;
#1530 = DIRECTION ( 'NONE',  ( 0.1081190184239421009, -0.9941379571543595972, 0.000000000000000000 ) ) ;
#1531 = DIRECTION ( 'NONE',  ( 0.000000000000000000, -7.888609052210118054E-31, -1.000000000000000000 ) ) ;
#1532 = CARTESIAN_POINT ( 'NONE',  ( 0.000000000000000000, 0.000000000000000000, 0.000000000000000000 ) ) ;
#1533 = VERTEX_POINT ( 'NONE', #6134 ) ;
#1534 = DIRECTION ( 'NONE',  ( -0.000000000000000000, -0.000000000000000000, -1.000000000000000000 ) ) ;
#1535 = DIRECTION ( 'NONE',  ( 0.000000000000000000, -1.000000000000000000, -2.465190328815662439E-32 ) ) ;
#1536 = ORIENTED_EDGE ( 'NONE', *, *, #13345, .F. ) ;
#1537 = CARTESIAN_POINT ( 'NONE',  ( 8.768203845046324740E-16, -14.96303950468941402, 26.76267923429985629 ) ) ;
#1538 = LINE ( 'NONE', #836, #12071 ) ;
#1539 = DIRECTION ( 'NONE',  ( 3.469446951953832974E-18, 1.000000000000000000, -7.888609052210118054E-31 ) ) ;
#1540 = ORIENTED_EDGE ( 'NONE', *, *, #30668, .F. ) ;
#1541 = ADVANCED_FACE ( 'NONE', ( #9351 ), #11683, .T. ) ;
#1542 = EDGE_CURVE ( 'NONE', #423, #15936, #25719, .T. ) ;
#1543 = CARTESIAN_POINT ( 'NONE',  ( -349.0000000000000000, 124.9999999999999432, 181.0000000000000000 ) ) ;
#1544 = ORIENTED_EDGE ( 'NONE', *, *, #30501, .F. ) ;
#1545 = PLANE ( 'NONE',  #20508 ) ;
#1546 = EDGE_CURVE ( 'NONE', #29191, #1290, #25361, .T. ) ;
#1547 = VECTOR ( 'NONE', #10685, 1000.000000000000000 ) ;
#1548 = AXIS2_PLACEMENT_3D ( 'NONE', #5309, #19047, #32723 ) ;
#1549 = ORIENTED_EDGE ( 'NONE', *, *, #30645, .F. ) ;
#1550 = CYLINDRICAL_SURFACE ( 'NONE', #16030, 3.999999999999976019 ) ;
#1551 = CYLINDRICAL_SURFACE ( 'NONE', #7101, 3.999999999999976019 ) ;
#1552 = ORIENTED_EDGE ( 'NONE', *, *, #6009, .F. ) ;
#1553 = DIRECTION ( 'NONE',  ( -0.1063910735369225230, 0.9943243633099118073, -1.000770725407345128E-14 ) ) ;
#1554 = CIRCLE ( 'NONE', #28261, 4.309328216469825001 ) ;
#1555 = ORIENTED_EDGE ( 'NONE', *, *, #18031, .F. ) ;
#1556 = CARTESIAN_POINT ( 'NONE',  ( 105.7529209506896422, -5.691643476845047012, 11.12904465084466565 ) ) ;
#1557 = EDGE_LOOP ( 'NONE', ( #29453, #13377 ) ) ;
#1558 = CYLINDRICAL_SURFACE ( 'NONE', #28650, 3.999999999999976019 ) ;
#1559 = ADVANCED_FACE ( 'NONE', ( #27856 ), #3466, .F. ) ;
#1560 = DIRECTION ( 'NONE',  ( -1.000000000000000000, 0.000000000000000000, 0.000000000000000000 ) ) ;
#1561 = ADVANCED_FACE ( 'NONE', ( #6668 ), #17563, .T. ) ;
#1562 = CIRCLE ( 'NONE', #2694, 7.999999999999979572 ) ;
#1563 = DIRECTION ( 'NONE',  ( 0.000000000000000000, 0.000000000000000000, -1.000000000000000000 ) ) ;
#1564 = DIRECTION ( 'NONE',  ( 0.000000000000000000, 0.000000000000000000, 1.000000000000000000 ) ) ;
#1565 = VERTEX_POINT ( 'NONE', #25179 ) ;
#1566 = ORIENTED_EDGE ( 'NONE', *, *, #325, .T. ) ;
#1567 = VERTEX_POINT ( 'NONE', #17212 ) ;
#1568 = PRODUCT_DEFINITION_SHAPE ( 'NONE', 'NONE',  #35113 ) ;
#1569 = CARTESIAN_POINT ( 'NONE',  ( -499.9999999999999432, -145.0000000000000000, -162.9999999999999716 ) ) ;
#1570 = EDGE_CURVE ( 'NONE', #2181, #9401, #22532, .T. ) ;
#1571 = CARTESIAN_POINT ( 'NONE',  ( -345.0000000000000000, -125.0000000000000284, 126.0000000000000000 ) ) ;
#1572 = CIRCLE ( 'NONE', #10080, 10.00000000000000000 ) ;
#1573 = TOROIDAL_SURFACE ( 'NONE', #14654, 30.47050528711512030, 8.000000000000000000 ) ;
#1574 = LINE ( 'NONE', #28795, #6521 ) ;
#1575 = DIRECTION ( 'NONE',  ( 0.000000000000000000, 0.000000000000000000, -1.000000000000000000 ) ) ;
#1576 = CARTESIAN_POINT ( 'NONE',  ( -19.99999999999998934, 134.9999999999998863, 187.0000000000000000 ) ) ;
#1577 = ORIENTED_EDGE ( 'NONE', *, *, #13570, .F. ) ;
#1578 = EDGE_CURVE ( 'NONE', #28711, #30135, #4167, .T. ) ;
#1579 = DIRECTION ( 'NONE',  ( 0.000000000000000000, 0.000000000000000000, 1.000000000000000000 ) ) ;
#1580 = VECTOR ( 'NONE', #9186, 1000.000000000000000 ) ;
#1581 = EDGE_LOOP ( 'NONE', ( #13449, #1380, #34172, #23284 ) ) ;
#1582 = CARTESIAN_POINT ( 'NONE',  ( 1.394999999999999574, -18.66807150955433769, 28.91175816027496381 ) ) ;
#1583 = ORIENTED_EDGE ( 'NONE', *, *, #32329, .F. ) ;
#1584 = CARTESIAN_POINT ( 'NONE',  ( 1.749999999999999778, -25.27164158951550732, -23.36088151536945645 ) ) ;
#1585 = DIRECTION ( 'NONE',  ( 0.9766205557100867685, 0.2149704402110236834, 3.948942922735914076E-17 ) ) ;
#1586 = CIRCLE ( 'NONE', #11849, 7.999999999999979572 ) ;
#1587 = DIRECTION ( 'NONE',  ( 0.000000000000000000, 1.000000000000000000, 0.000000000000000000 ) ) ;
#1588 = CARTESIAN_POINT ( 'NONE',  ( -500.0000000000000000, -137.0000000000000000, 155.0000000000000000 ) ) ;
#1589 = EDGE_CURVE ( 'NONE', #5237, #5316, #28038, .T. ) ;
#1590 = CARTESIAN_POINT ( 'NONE',  ( 42.44043929807611448, -17.65143121711728469, 0.000000000000000000 ) ) ;
#1591 = ORIENTED_EDGE ( 'NONE', *, *, #33237, .T. ) ;
#1592 = CIRCLE ( 'NONE', #13512, 7.999999999999979572 ) ;
#1593 = VECTOR ( 'NONE', #14428, 1000.000000000000000 ) ;
#1594 = VERTEX_POINT ( 'NONE', #9691 ) ;
#1595 = DIRECTION ( 'NONE',  ( -1.148577860975596558E-14, -4.996422718717765158E-14, 0.9999999999999998890 ) ) ;
#1596 = ORIENTED_EDGE ( 'NONE', *, *, #34606, .T. ) ;
#1597 = ADVANCED_FACE ( 'NONE', ( #34432 ), #28911, .F. ) ;
#1598 = CIRCLE ( 'NONE', #5542, 32.54542015209055705 ) ;
#1599 = EDGE_CURVE ( 'NONE', #27420, #3383, #29381, .T. ) ;
#1600 = LINE ( 'NONE', #23659, #4417 ) ;
#1601 = EDGE_CURVE ( 'NONE', #14586, #5645, #7354, .T. ) ;
#1602 = CARTESIAN_POINT ( 'NONE',  ( -45.05956070192387841, -32.65143121711728469, 20.00000000000000000 ) ) ;
#1603 = ORIENTED_EDGE ( 'NONE', *, *, #13178, .F. ) ;
#1604 = DIRECTION ( 'NONE',  ( -1.000000000000000000, -0.000000000000000000, -0.000000000000000000 ) ) ;
#1606 = DIRECTION ( 'NONE',  ( -0.4198891015602640997, -0.9075754196709572286, 0.000000000000000000 ) ) ;
#1605 = DIRECTION ( 'NONE',  ( -0.000000000000000000, 1.000000000000000000, -0.000000000000000000 ) ) ;
#1607 = CIRCLE ( 'NONE', #3885, 32.54542015209054995 ) ;
#1608 = ORIENTED_EDGE ( 'NONE', *, *, #29083, .F. ) ;
#1609 = ORIENTED_EDGE ( 'NONE', *, *, #17986, .F. ) ;
#1610 = LINE ( 'NONE', #4267, #18005 ) ;
#1611 = DIRECTION ( 'NONE',  ( -1.300283923313630633E-47, 0.000000000000000000, 1.000000000000000000 ) ) ;
#1612 = FACE_OUTER_BOUND ( 'NONE', #15707, .T. ) ;
#1613 = VERTEX_POINT ( 'NONE', #10394 ) ;
#1614 = DIRECTION ( 'NONE',  ( -0.000000000000000000, -1.000000000000000000, -0.000000000000000000 ) ) ;
#1615 = AXIS2_PLACEMENT_3D ( 'NONE', #9963, #23157, #20822 ) ;
#1616 = PRODUCT_DEFINITION_SHAPE ( 'NONE', 'NONE',  #35203 ) ;
#1617 = VERTEX_POINT ( 'NONE', #31408 ) ;
#1618 = CARTESIAN_POINT ( 'NONE',  ( 15.99999999999997868, -145.0000000000000000, -186.9999999999999716 ) ) ;
#1619 = SURFACE_SIDE_STYLE ('',( #32036 ) ) ;
#1620 = CARTESIAN_POINT ( 'NONE',  ( 2.567399184519788768, -37.78162119159484433, -36.68877005347593467 ) ) ;
#1621 = CIRCLE ( 'NONE', #19248, 16.00000000000000000 ) ;
#1623 = CARTESIAN_POINT ( 'NONE',  ( -5.021133111225092982, -11.61907005722761532, -67.50000000000000000 ) ) ;
#1622 = FACE_OUTER_BOUND ( 'NONE', #15105, .T. ) ;
#1624 = CARTESIAN_POINT ( 'NONE',  ( 0.000000000000000000, 0.000000000000000000, -3.000000000000000000 ) ) ;
#1625 = DIRECTION ( 'NONE',  ( -5.546364386991661285E-52, 0.000000000000000000, -1.000000000000000000 ) ) ;
#1626 = CARTESIAN_POINT ( 'NONE',  ( 0.01642902444827818234, 28.19451832957808435, -12.86842533592864868 ) ) ;
#1627 = CARTESIAN_POINT ( 'NONE',  ( -499.9999999999999432, -145.0000000000000000, -187.0000000000000000 ) ) ;
#1628 = AXIS2_PLACEMENT_3D ( 'NONE', #14190, #24007, #830 ) ;
#1629 = ORIENTED_EDGE ( 'NONE', *, *, #19026, .F. ) ;
#1630 =( NAMED_UNIT ( * ) SI_UNIT ( $, .STERADIAN. ) SOLID_ANGLE_UNIT ( ) );
#1631 = ORIENTED_EDGE ( 'NONE', *, *, #12031, .F. ) ;
#1632 = EDGE_LOOP ( 'NONE', ( #11200, #2339 ) ) ;
#1633 = ADVANCED_FACE ( 'NONE', ( #34077 ), #26587, .T. ) ;
#1634 = MECHANICAL_DESIGN_GEOMETRIC_PRESENTATION_REPRESENTATION (  '', ( #21543 ), #23797 ) ;
#1635 = EDGE_CURVE ( 'NONE', #15525, #19610, #9424, .T. ) ;
#1636 = DIRECTION ( 'NONE',  ( 0.000000000000000000, 0.000000000000000000, 1.000000000000000000 ) ) ;
#1637 = ORIENTED_EDGE ( 'NONE', *, *, #15211, .T. ) ;
#1638 = ORIENTED_EDGE ( 'NONE', *, *, #5076, .T. ) ;
#1639 = VERTEX_POINT ( 'NONE', #1853 ) ;
#1640 = EDGE_CURVE ( 'NONE', #21299, #6869, #11120, .T. ) ;
#1641 = CYLINDRICAL_SURFACE ( 'NONE', #33225, 34.41491905851385269 ) ;
#1642 = CIRCLE ( 'NONE', #33458, 4.000000000000003553 ) ;
#1643 = ITEM_DEFINED_TRANSFORMATION ( 'NONE', 'NONE', #29777,  #28566 ) ;
#1644 = ORIENTED_EDGE ( 'NONE', *, *, #4995, .F. ) ;
#1645 = FACE_OUTER_BOUND ( 'NONE', #15064, .T. ) ;
#1646 = DIRECTION ( 'NONE',  ( 0.000000000000000000, 1.000000000000000000, 3.374343856708137958E-53 ) ) ;
#1647 = EDGE_LOOP ( 'NONE', ( #35054, #12511, #7318, #1089 ) ) ;
#1648 = ORIENTED_EDGE ( 'NONE', *, *, #30047, .F. ) ;
#1649 = FACE_OUTER_BOUND ( 'NONE', #18770, .T. ) ;
#1650 = FACE_OUTER_BOUND ( 'NONE', #15361, .T. ) ;
#1651 = EDGE_CURVE ( 'NONE', #12523, #25735, #8256, .T. ) ;
#1652 = LINE ( 'NONE', #10193, #28394 ) ;
#1653 = LINE ( 'NONE', #31040, #5724 ) ;
#1654 = DIRECTION ( 'NONE',  ( 0.8835120444460229372, 0.4684084406997900407, -0.000000000000000000 ) ) ;
#1655 = EDGE_LOOP ( 'NONE', ( #29027, #28886, #34662, #16670 ) ) ;
#1656 = DIRECTION ( 'NONE',  ( 0.000000000000000000, 0.000000000000000000, 1.000000000000000000 ) ) ;
#1657 = PLANE ( 'NONE',  #11701 ) ;
#1658 = AXIS2_PLACEMENT_3D ( 'NONE', #31039, #31375, #3613 ) ;
#1659 = CARTESIAN_POINT ( 'NONE',  ( 2.789999999999999147, -29.32277567846606203, 8.169899392882690847 ) ) ;
#1660 = ORIENTED_EDGE ( 'NONE', *, *, #33278, .F. ) ;
#1661 = DIRECTION ( 'NONE',  ( 0.000000000000000000, 0.000000000000000000, -1.000000000000000000 ) ) ;
#1662 = CARTESIAN_POINT ( 'NONE',  ( 145.0000000000000568, -167.8552739801376390, -46.75049602362128809 ) ) ;
#1663 = DIRECTION ( 'NONE',  ( 0.000000000000000000, 0.000000000000000000, 1.000000000000000000 ) ) ;
#1664 = DIRECTION ( 'NONE',  ( 1.000000000000000000, 0.000000000000000000, -0.000000000000000000 ) ) ;
#1666 = CARTESIAN_POINT ( 'NONE',  ( 8.000000000000000000, 0.000000000000000000, 0.000000000000000000 ) ) ;
#1665 = DIRECTION ( 'NONE',  ( 1.000000000000000000, 0.000000000000000000, 0.000000000000000000 ) ) ;
#1667 = VECTOR ( 'NONE', #14363, 1000.000000000000000 ) ;
#1668 = CARTESIAN_POINT ( 'NONE',  ( 145.0000000000000568, -97.49999999999998579, 51.88904920397793319 ) ) ;
#1669 = ORIENTED_EDGE ( 'NONE', *, *, #20197, .F. ) ;
#1670 = CARTESIAN_POINT ( 'NONE',  ( 19.99999999999998934, -137.0000000000000000, 155.0000000000000000 ) ) ;
#1672 = CARTESIAN_POINT ( 'NONE',  ( -414.0000000000000568, 124.9999999999999432, -162.9999999999999716 ) ) ;
#1671 = CARTESIAN_POINT ( 'NONE',  ( 2.765921099433441999, 26.03801215795542134, -16.98986790278583570 ) ) ;
#1673 = AXIS2_PLACEMENT_3D ( 'NONE', #6817, #34409, #17706 ) ;
#1674 = ORIENTED_EDGE ( 'NONE', *, *, #937, .F. ) ;
#1675 = DIRECTION ( 'NONE',  ( 1.000000000000000000, 3.469446951953834515E-18, 0.000000000000000000 ) ) ;
#1676 = EDGE_LOOP ( 'NONE', ( #26031, #3781, #26289, #18122 ) ) ;
#1677 = EDGE_CURVE ( 'NONE', #5400, #14586, #12828, .T. ) ;
#1678 = VECTOR ( 'NONE', #2137, 1000.000000000000000 ) ;
#1679 = APPLICATION_CONTEXT ( 'automotive_design' ) ;
#1680 = ORIENTED_EDGE ( 'NONE', *, *, #10734, .F. ) ;
#1681 = CARTESIAN_POINT ( 'NONE',  ( 2.789999999999999147, -20.35927063852789232, -24.61013060777193218 ) ) ;
#1682 = ORIENTED_EDGE ( 'NONE', *, *, #28659, .T. ) ;
#1683 = VERTEX_POINT ( 'NONE', #4679 ) ;
#1684 = EDGE_CURVE ( 'NONE', #12202, #22339, #4337, .T. ) ;
#1685 = DIRECTION ( 'NONE',  ( 0.000000000000000000, 1.000000000000000000, 5.053935297177146739E-49 ) ) ;
#1686 = EDGE_CURVE ( 'NONE', #14706, #14486, #11041, .T. ) ;
#1687 = CARTESIAN_POINT ( 'NONE',  ( -20.00000000000007461, 136.9999999999999432, 162.9999999999999716 ) ) ;
#1688 = DIRECTION ( 'NONE',  ( 0.000000000000000000, -5.053935297177146739E-49, -1.000000000000000000 ) ) ;
#1689 = EDGE_CURVE ( 'NONE', #15148, #19084, #5353, .T. ) ;
#1690 = EDGE_LOOP ( 'NONE', ( #7739, #345, #3044, #15845 ) ) ;
#1691 = EDGE_CURVE ( 'NONE', #9401, #23007, #20725, .T. ) ;
#1692 = ORIENTED_EDGE ( 'NONE', *, *, #27472, .F. ) ;
#1693 = DIRECTION ( 'NONE',  ( 0.000000000000000000, 0.000000000000000000, 1.000000000000000000 ) ) ;
#1694 = CARTESIAN_POINT ( 'NONE',  ( 11.99999999999995559, -145.0000000000000000, 187.0000000000000000 ) ) ;
#1695 = DIRECTION ( 'NONE',  ( -5.546364386991661285E-52, 0.000000000000000000, -1.000000000000000000 ) ) ;
#1696 = EDGE_CURVE ( 'NONE', #23220, #32336, #12547, .T. ) ;
#1697 = CARTESIAN_POINT ( 'NONE',  ( -442.0000000000000000, 124.9999999999999574, -194.9999999999999716 ) ) ;
#1698 = CARTESIAN_POINT ( 'NONE',  ( -442.0000000000000000, -137.0000000000000000, -155.0000000000000000 ) ) ;
#1699 = ORIENTED_EDGE ( 'NONE', *, *, #11310, .F. ) ;
#1700 = VECTOR ( 'NONE', #12167, 1000.000000000000000 ) ;
#1701 = ORIENTED_EDGE ( 'NONE', *, *, #32394, .F. ) ;
#1702 = CARTESIAN_POINT ( 'NONE',  ( 1.749999999999999778, -18.66807150955392913, -28.91175816027522671 ) ) ;
#1703 = LINE ( 'NONE', #15247, #2230 ) ;
#1704 = VERTEX_POINT ( 'NONE', #20733 ) ;
#1705 = CARTESIAN_POINT ( 'NONE',  ( 0.7564103443181301456, 33.57753319639230227, 4.776354065835291429 ) ) ;
#1706 = DIRECTION ( 'NONE',  ( -1.000000000000000000, -0.000000000000000000, -0.000000000000000000 ) ) ;
#1707 = EDGE_CURVE ( 'NONE', #9925, #10965, #18424, .T. ) ;
#1708 = FACE_OUTER_BOUND ( 'NONE', #15646, .T. ) ;
#1709 = EDGE_LOOP ( 'NONE', ( #8360, #692, #21365, #8682, #1372, #28525, #28831, #21209 ) ) ;
#1710 = B_SPLINE_CURVE_WITH_KNOTS ( 'NONE', 3,
 ( #22334, #12024, #8988, #8621, #30342, #32997 ),
 .UNSPECIFIED., .F., .F.,
 ( 4, 2, 4 ),
 ( 2.555309558411697678E-07, 0.001873453885876980246, 0.003746652240798119347 ),
 .UNSPECIFIED. ) ;
#1711 = DIRECTION ( 'NONE',  ( 0.000000000000000000, 1.000000000000000000, 0.000000000000000000 ) ) ;
#1712 = VERTEX_POINT ( 'NONE', #7183 ) ;
#1714 = CARTESIAN_POINT ( 'NONE',  ( -499.9999999999999432, 144.9999999999999716, 187.0000000000000000 ) ) ;
#1713 = CARTESIAN_POINT ( 'NONE',  ( -20.00000000000007461, -113.0000000000000000, -190.9999999999999716 ) ) ;
#1715 = DIRECTION ( 'NONE',  ( 1.000000000000000000, 0.000000000000000000, -0.000000000000000000 ) ) ;
#1716 = VERTEX_POINT ( 'NONE', #4860 ) ;
#1717 = CARTESIAN_POINT ( 'NONE',  ( -445.9999999999999432, -125.0000000000000000, 162.9999999999999716 ) ) ;
#1718 = LINE ( 'NONE', #10084, #33852 ) ;
#1719 = EDGE_LOOP ( 'NONE', ( #29333, #7728, #12429, #25576 ) ) ;
#1720 = CIRCLE ( 'NONE', #8530, 7.999999999999979572 ) ;
#1721 = DIRECTION ( 'NONE',  ( -7.893605728314051750E-14, 1.618803117314786530E-15, 1.000000000000000000 ) ) ;
#1722 = VERTEX_POINT ( 'NONE', #2207 ) ;
#1723 = CARTESIAN_POINT ( 'NONE',  ( 104.2381396081001412, -5.690476701307018104, 11.12964202013672299 ) ) ;
#1724 = ORIENTED_EDGE ( 'NONE', *, *, #30385, .T. ) ;
#1725 = CARTESIAN_POINT ( 'NONE',  ( -499.9999999999999432, -113.0000000000000000, -159.0000000000000000 ) ) ;
#1726 = DIRECTION ( 'NONE',  ( 1.000000000000000000, 0.000000000000000000, 0.000000000000000000 ) ) ;
#1727 = DIRECTION ( 'NONE',  ( 0.000000000000000000, 0.000000000000000000, 1.000000000000000000 ) ) ;
#1728 = VECTOR ( 'NONE', #27829, 1000.000000000000000 ) ;
#1729 = DIRECTION ( 'NONE',  ( -1.000000000000000000, 0.000000000000000000, 0.000000000000000000 ) ) ;
#1730 = CONTEXT_DEPENDENT_SHAPE_REPRESENTATION ( #32390, #6311 ) ;
#1731 = ADVANCED_FACE ( 'NONE', ( #23905, #34783, #32098, #7714, #18599, #29443, #5209, #10756, #16815, #24081, #24427, #7896, #8069, #19127, #8423 ), #13955, .F. ) ;
#1732 = ORIENTED_EDGE ( 'NONE', *, *, #9450, .T. ) ;
#1733 = ADVANCED_FACE ( 'NONE', ( #34963, #26940 ), #5393, .T. ) ;
#1734 = ORIENTED_EDGE ( 'NONE', *, *, #18176, .F. ) ;
#1735 = ORIENTED_EDGE ( 'NONE', *, *, #12554, .F. ) ;
#1736 = DIRECTION ( 'NONE',  ( 1.000000000000000000, 3.469446951953834515E-18, 0.000000000000000000 ) ) ;
#1737 = DIRECTION ( 'NONE',  ( 3.697785493223492838E-32, 1.934419779023891545E-16, -1.000000000000000000 ) ) ;
#1738 = CARTESIAN_POINT ( 'NONE',  ( 19.99999999999998934, -55.00000000000000711, 154.9999999999999716 ) ) ;
#1739 = DIRECTION ( 'NONE',  ( 0.000000000000000000, 0.000000000000000000, -1.000000000000000000 ) ) ;
#1740 = DIRECTION ( 'NONE',  ( -1.000000000000000000, 6.792721752314501023E-48, -3.697785493223492838E-32 ) ) ;
#1741 = DIRECTION ( 'NONE',  ( 0.000000000000000000, -0.000000000000000000, -1.000000000000000000 ) ) ;
#1742 = VERTEX_POINT ( 'NONE', #22131 ) ;
#1743 = AXIS2_PLACEMENT_3D ( 'NONE', #32287, #22148, #16647 ) ;
#1744 = CYLINDRICAL_SURFACE ( 'NONE', #33902, 16.19999999999999574 ) ;
#1745 = CARTESIAN_POINT ( 'NONE',  ( -414.0000000000000568, 113.0000000000000000, -155.0000000000000000 ) ) ;
#1746 = ADVANCED_FACE ( 'NONE', ( #3255 ), #24605, .F. ) ;
#1747 = ORIENTED_EDGE ( 'NONE', *, *, #21577, .F. ) ;
#1748 = LINE ( 'NONE', #9245, #34250 ) ;
#1749 = EDGE_LOOP ( 'NONE', ( #32130, #272, #159, #32027 ) ) ;
#1750 = DIRECTION ( 'NONE',  ( 1.000000000000000000, 0.000000000000000000, 0.000000000000000000 ) ) ;
#1751 = EDGE_CURVE ( 'NONE', #23608, #11201, #16457, .T. ) ;
#1752 = FACE_OUTER_BOUND ( 'NONE', #33427, .T. ) ;
#1753 = ADVANCED_FACE ( 'NONE', ( #18774 ), #29613, .F. ) ;
#1754 = EDGE_CURVE ( 'NONE', #26155, #22562, #14485, .T. ) ;
#1755 = VECTOR ( 'NONE', #29586, 1000.000000000000000 ) ;
#1756 = CIRCLE ( 'NONE', #21651, 44.99999999999998579 ) ;
#1757 = DIRECTION ( 'NONE',  ( 0.000000000000000000, 1.000000000000000000, 5.145227585319922065E-49 ) ) ;
#1758 = MECHANICAL_DESIGN_GEOMETRIC_PRESENTATION_REPRESENTATION (  '', ( #9156 ), #23929 ) ;
#1759 = DIRECTION ( 'NONE',  ( 0.000000000000000000, 0.000000000000000000, -1.000000000000000000 ) ) ;
#1760 = FACE_BOUND ( 'NONE', #2139, .T. ) ;
#1761 = EDGE_CURVE ( 'NONE', #2593, #32910, #21774, .T. ) ;
#1762 = ORIENTED_EDGE ( 'NONE', *, *, #9120, .F. ) ;
#1763 = ORIENTED_EDGE ( 'NONE', *, *, #31218, .T. ) ;
#1764 = DIRECTION ( 'NONE',  ( -0.1063910735369017202, 0.9943243633099136947, -1.000770725407181676E-14 ) ) ;
#1765 = ORIENTED_EDGE ( 'NONE', *, *, #4038, .T. ) ;
#1766 = AXIS2_PLACEMENT_3D ( 'NONE', #4866, #15764, #4174 ) ;
#1767 = LINE ( 'NONE', #14967, #32858 ) ;
#1768 = DIRECTION ( 'NONE',  ( 0.000000000000000000, 1.836970198721029441E-16, -1.000000000000000000 ) ) ;
#1769 = CARTESIAN_POINT ( 'NONE',  ( 105.1990410865049057, -5.738006884272855324, 4.829624934769205069 ) ) ;
#1770 = CONTEXT_DEPENDENT_SHAPE_REPRESENTATION ( #1223, #20610 ) ;
#1771 = VERTEX_POINT ( 'NONE', #21603 ) ;
#1772 = CARTESIAN_POINT ( 'NONE',  ( -5.527271473480783293, -1.747512292859696226, -0.7500000000000000000 ) ) ;
#1774 = FACE_OUTER_BOUND ( 'NONE', #27919, .T. ) ;
#1773 = CARTESIAN_POINT ( 'NONE',  ( 2.765921099433442887, 24.20451283648829133, 19.51346322004938827 ) ) ;
#1776 = ORIENTED_EDGE ( 'NONE', *, *, #17601, .F. ) ;
#1775 = CIRCLE ( 'NONE', #26215, 32.54542015209055705 ) ;
#1777 = ORIENTED_EDGE ( 'NONE', *, *, #16323, .F. ) ;
#1778 = LINE ( 'NONE', #4964, #24830 ) ;
#1779 = AXIS2_PLACEMENT_3D ( 'NONE', #30254, #8011, #30087 ) ;
#1780 = VERTEX_POINT ( 'NONE', #2894 ) ;
#1781 = VECTOR ( 'NONE', #20154, 1000.000000000000000 ) ;
#1782 = FACE_OUTER_BOUND ( 'NONE', #3943, .T. ) ;
#1783 = CARTESIAN_POINT ( 'NONE',  ( 11.99999999999999645, -124.9999999999999432, -154.9999999999999716 ) ) ;
#1784 = ORIENTED_EDGE ( 'NONE', *, *, #18783, .F. ) ;
#1785 = CARTESIAN_POINT ( 'NONE',  ( 2.789999999999999147, -20.92506858792740587, -22.14933852381698642 ) ) ;
#1786 = ORIENTED_EDGE ( 'NONE', *, *, #28659, .F. ) ;
#1787 = CARTESIAN_POINT ( 'NONE',  ( 11.99999999999999645, 144.9999999999999147, 155.0000000000000000 ) ) ;
#1788 = DIRECTION ( 'NONE',  ( 0.000000000000000000, -1.000000000000000000, 0.000000000000000000 ) ) ;
#1789 = AXIS2_PLACEMENT_3D ( 'NONE', #23876, #11559, #21871 ) ;
#1790 = DIRECTION ( 'NONE',  ( -1.000000000000000000, 0.000000000000000000, 0.000000000000000000 ) ) ;
#1791 = ADVANCED_FACE ( 'NONE', ( #8591 ), #32443, .F. ) ;
#1793 = CARTESIAN_POINT ( 'NONE',  ( 2.765921099433441555, -0.3931553186911057041, -31.08824725498900676 ) ) ;
#1792 = CARTESIAN_POINT ( 'NONE',  ( 2.789999999999999147, -7.666252171205286459, -29.49034198003814566 ) ) ;
#1794 = ADVANCED_FACE ( 'NONE', ( #27110 ), #24791, .T. ) ;
#1795 = DIRECTION ( 'NONE',  ( -0.000000000000000000, -0.000000000000000000, 1.000000000000000000 ) ) ;
#1796 = CARTESIAN_POINT ( 'NONE',  ( -418.0000000000000000, -124.9999999999999858, -73.99999999999998579 ) ) ;
#1797 = DIRECTION ( 'NONE',  ( -1.000000000000000000, -0.000000000000000000, -0.000000000000000000 ) ) ;
#1798 = FILL_AREA_STYLE ('',( #1113 ) ) ;
#1799 = PRODUCT_DEFINITION_SHAPE ( 'NONE', 'NONE',  #35130 ) ;
#1800 = AXIS2_PLACEMENT_3D ( 'NONE', #12982, #7969, #16185 ) ;
#1801 = VERTEX_POINT ( 'NONE', #11106 ) ;
#1802 = AXIS2_PLACEMENT_3D ( 'NONE', #23257, #14557, #11885 ) ;
#1803 = AXIS2_PLACEMENT_3D ( 'NONE', #25568, #28253, #22915 ) ;
#1804 = VECTOR ( 'NONE', #19250, 1000.000000000000000 ) ;
#1805 = TOROIDAL_SURFACE ( 'NONE', #33644, 30.47050528711511674, 8.000000000000000000 ) ;
#1806 = ORIENTED_EDGE ( 'NONE', *, *, #16042, .F. ) ;
#1807 = ORIENTED_EDGE ( 'NONE', *, *, #6445, .F. ) ;
#1808 = CARTESIAN_POINT ( 'NONE',  ( 110.5382509904757313, 1.550744593849150865, 7.348056298371736794 ) ) ;
#1809 = DIRECTION ( 'NONE',  ( 2.511857874265824811E-14, 1.173547878685569722E-14, 1.000000000000000000 ) ) ;
#1810 = ORIENTED_EDGE ( 'NONE', *, *, #7138, .F. ) ;
#1811 = ORIENTED_EDGE ( 'NONE', *, *, #24121, .F. ) ;
#1812 = VERTEX_POINT ( 'NONE', #8243 ) ;
#1813 = DIRECTION ( 'NONE',  ( 0.2675283385292216987, -0.9635499925192227977, 0.000000000000000000 ) ) ;
#1814 = ORIENTED_EDGE ( 'NONE', *, *, #8906, .F. ) ;
#1815 = CARTESIAN_POINT ( 'NONE',  ( -27.84632068199329780, 25.66368763279034226, 68.31122994652405112 ) ) ;
#1816 = CARTESIAN_POINT ( 'NONE',  ( -418.0000000000000000, -125.0000000000000000, 194.9999999999999716 ) ) ;
#1817 = ORIENTED_EDGE ( 'NONE', *, *, #6051, .F. ) ;
#1818 = ORIENTED_EDGE ( 'NONE', *, *, #9423, .F. ) ;
#1819 = LINE ( 'NONE', #12700, #27634 ) ;
#1820 = DIRECTION ( 'NONE',  ( 0.000000000000000000, -1.000000000000000000, 3.421138828918010427E-49 ) ) ;
#1821 = CARTESIAN_POINT ( 'NONE',  ( 2.789999999999999147, 20.99477179376825120, 22.93149026599753526 ) ) ;
#1822 = CARTESIAN_POINT ( 'NONE',  ( 2.789999999999999147, -29.32277567846594835, -8.169899392883101186 ) ) ;
#1823 = CARTESIAN_POINT ( 'NONE',  ( 119.9999999999998295, 1.224646799147353256E-15, -10.00000000000000000 ) ) ;
#1824 = ORIENTED_EDGE ( 'NONE', *, *, #20677, .F. ) ;
#1825 = VECTOR ( 'NONE', #18332, 1000.000000000000114 ) ;
#1826 = DIRECTION ( 'NONE',  ( 0.000000000000000000, -1.000000000000000000, 0.000000000000000000 ) ) ;
#1827 = DIRECTION ( 'NONE',  ( 0.000000000000000000, -1.000000000000000000, 6.123233995736766036E-17 ) ) ;
#1828 = VECTOR ( 'NONE', #34629, 1000.000000000000000 ) ;
#1829 = DIRECTION ( 'NONE',  ( 3.697785493223492838E-32, 1.934419779023891545E-16, -1.000000000000000000 ) ) ;
#1830 = ORIENTED_EDGE ( 'NONE', *, *, #3032, .T. ) ;
#1831 = VECTOR ( 'NONE', #8844, 1000.000000000000000 ) ;
#1832 = CARTESIAN_POINT ( 'NONE',  ( 0.000000000000000000, 12.80000000000000071, -3.000000000000000000 ) ) ;
#1833 = EDGE_CURVE ( 'NONE', #1364, #11691, #30931, .T. ) ;
#1834 = LINE ( 'NONE', #13234, #29745 ) ;
#1835 = CARTESIAN_POINT ( 'NONE',  ( 110.3448550603046527, 2.096151729099205774, -7.203423290846323823 ) ) ;
#1837 = CARTESIAN_POINT ( 'NONE',  ( -108.8342207477093240, 3.400963087932895146, -6.689628992625347159 ) ) ;
#1836 = CARTESIAN_POINT ( 'NONE',  ( -414.0000000000000568, -125.0000000000000000, 107.9999999999999858 ) ) ;
#1838 = ADVANCED_FACE ( 'NONE', ( #30133 ), #16631, .T. ) ;
#1839 = DIRECTION ( 'NONE',  ( 0.000000000000000000, 0.000000000000000000, 1.000000000000000000 ) ) ;
#1840 = ORIENTED_EDGE ( 'NONE', *, *, #24407, .T. ) ;
#1841 = EDGE_CURVE ( 'NONE', #5027, #30076, #11284, .T. ) ;
#1842 = DIRECTION ( 'NONE',  ( 0.000000000000000000, -1.000000000000000000, -2.465190328815662439E-32 ) ) ;
#1844 = CYLINDRICAL_SURFACE ( 'NONE', #396, 7.999999999999979572 ) ;
#1843 =( LENGTH_UNIT ( ) NAMED_UNIT ( * ) SI_UNIT ( .MILLI., .METRE. ) );
#1845 = ORIENTED_EDGE ( 'NONE', *, *, #34788, .F. ) ;
#1846 = DIRECTION ( 'NONE',  ( 0.000000000000000000, 0.9048270524660234626, -0.4257792915650642773 ) ) ;
#1847 = PRODUCT_DEFINITION_SHAPE ( 'NONE', 'NONE',  #35120 ) ;
#1848 = VERTEX_POINT ( 'NONE', #30841 ) ;
#1849 = AXIS2_PLACEMENT_3D ( 'NONE', #21766, #21427, #13769 ) ;
#1850 = CIRCLE ( 'NONE', #21749, 7.999999999999979572 ) ;
#1851 = AXIS2_PLACEMENT_3D ( 'NONE', #14872, #12538, #26057 ) ;
#1852 = ORIENTED_EDGE ( 'NONE', *, *, #29644, .T. ) ;
#1853 = CARTESIAN_POINT ( 'NONE',  ( 60.00000000000000000, 33.69708579775584667, -49.43553178847298568 ) ) ;
#1854 = ORIENTED_EDGE ( 'NONE', *, *, #33044, .F. ) ;
#1855 = ORIENTED_EDGE ( 'NONE', *, *, #15617, .T. ) ;
#1856 = DIRECTION ( 'NONE',  ( 0.000000000000000000, -1.000000000000000000, -0.000000000000000000 ) ) ;
#1857 = CARTESIAN_POINT ( 'NONE',  ( 0.000000000000000000, -32.54542015209054995, -36.68877005347592757 ) ) ;
#1858 = DIRECTION ( 'NONE',  ( -1.000000000000000000, 0.000000000000000000, 0.000000000000000000 ) ) ;
#1859 = ORIENTED_EDGE ( 'NONE', *, *, #23919, .F. ) ;
#1860 = ORIENTED_EDGE ( 'NONE', *, *, #33232, .F. ) ;
#1861 = CARTESIAN_POINT ( 'NONE',  ( -20.00000000000007461, 136.9999999999999432, 194.9999999999999716 ) ) ;
#1862 = CARTESIAN_POINT ( 'NONE',  ( 11.99999999999999645, -55.00000000000000711, 162.9999999999999716 ) ) ;
#1863 = DIRECTION ( 'NONE',  ( 1.000000000000000000, 0.000000000000000000, 0.000000000000000000 ) ) ;
#1864 = CARTESIAN_POINT ( 'NONE',  ( -19.99999999999998934, -105.0000000000000142, 162.9999999999999716 ) ) ;
#1865 = FACE_OUTER_BOUND ( 'NONE', #3125, .T. ) ;
#1866 = ORIENTED_EDGE ( 'NONE', *, *, #9937, .F. ) ;
#1867 = ORIENTED_EDGE ( 'NONE', *, *, #17479, .T. ) ;
#1868 = CARTESIAN_POINT ( 'NONE',  ( -42.55956070192386420, -17.65143121711728469, 0.000000000000000000 ) ) ;
#1869 = DIRECTION ( 'NONE',  ( -1.000000000000000000, -0.000000000000000000, -0.000000000000000000 ) ) ;
#1870 = VERTEX_POINT ( 'NONE', #7097 ) ;
#1871 = CARTESIAN_POINT ( 'NONE',  ( 2.033589655505266158, -10.98355401466430337, -32.08778326630013567 ) ) ;
#1872 = CARTESIAN_POINT ( 'NONE',  ( 99.26191511054632599, 1.643815732525060864E-21, 12.50000000000000000 ) ) ;
#1873 = EDGE_CURVE ( 'NONE', #8552, #23988, #13891, .T. ) ;
#1874 = AXIS2_PLACEMENT_3D ( 'NONE', #27592, #33460, #16758 ) ;
#1875 = CARTESIAN_POINT ( 'NONE',  ( -418.0000000000000000, 109.0000000000000142, -175.0000000000000000 ) ) ;
#1876 = VERTEX_POINT ( 'NONE', #33680 ) ;
#1877 = AXIS2_PLACEMENT_3D ( 'NONE', #3498, #19362, #16524 ) ;
#1878 = AXIS2_PLACEMENT_3D ( 'NONE', #8187, #21720, #29213 ) ;
#1879 = CARTESIAN_POINT ( 'NONE',  ( 2.789999999999999147, 31.93991905851385837, 0.000000000000000000 ) ) ;
#1880 = ORIENTED_EDGE ( 'NONE', *, *, #20443, .F. ) ;
#1881 = EDGE_CURVE ( 'NONE', #1134, #13484, #14128, .T. ) ;
#1883 = PLANE ( 'NONE',  #374 ) ;
#1882 = DIRECTION ( 'NONE',  ( -1.000000000000000000, -0.000000000000000000, -0.000000000000000000 ) ) ;
#1884 = FACE_OUTER_BOUND ( 'NONE', #34354, .T. ) ;
#1885 = ORIENTED_EDGE ( 'NONE', *, *, #15153, .F. ) ;
#1886 = EDGE_CURVE ( 'NONE', #29036, #3883, #21854, .T. ) ;
#1887 = FACE_BOUND ( 'NONE', #19466, .T. ) ;
#1888 = CARTESIAN_POINT ( 'NONE',  ( -7.654999999999999361, 0.000000000000000000, -0.7500000000000000000 ) ) ;
#1889 = EDGE_CURVE ( 'NONE', #30258, #28753, #22427, .T. ) ;
#1890 = VERTEX_POINT ( 'NONE', #28998 ) ;
#1891 = CIRCLE ( 'NONE', #29164, 7.999999999999979572 ) ;
#1892 = CARTESIAN_POINT ( 'NONE',  ( 766.3743060314519653, 1249.272396330896072, 1753.598338701303646 ) ) ;
#1893 = VERTEX_POINT ( 'NONE', #948 ) ;
#1894 = CARTESIAN_POINT ( 'NONE',  ( 102.4434507907919141, -5.150622582557323526, 11.39062369188951607 ) ) ;
#1895 = ORIENTED_EDGE ( 'NONE', *, *, #26937, .F. ) ;
#1896 = PLANE ( 'NONE',  #808 ) ;
#1897 = AXIS2_PLACEMENT_3D ( 'NONE', #15486, #33635, #9258 ) ;
#1898 = DIRECTION ( 'NONE',  ( 0.000000000000000000, 0.000000000000000000, -1.000000000000000000 ) ) ;
#1899 = AXIS2_PLACEMENT_3D ( 'NONE', #12201, #34064, #30525 ) ;
#1900 = DIRECTION ( 'NONE',  ( 0.000000000000000000, 1.310824597558155437E-49, 1.000000000000000000 ) ) ;
#1901 = CARTESIAN_POINT ( 'NONE',  ( 10.00000000000000000, 0.000000000000000000, 13.50000000000000178 ) ) ;
#1902 = ITEM_DEFINED_TRANSFORMATION ( 'NONE', 'NONE', #31450,  #28566 ) ;
#1903 = ORIENTED_EDGE ( 'NONE', *, *, #33134, .F. ) ;
#1904 = ORIENTED_EDGE ( 'NONE', *, *, #11177, .F. ) ;
#1905 = VECTOR ( 'NONE', #15165, 1000.000000000000000 ) ;
#1906 = ORIENTED_EDGE ( 'NONE', *, *, #14574, .T. ) ;
#1907 = DIRECTION ( 'NONE',  ( -5.546364386991661285E-52, 0.000000000000000000, 1.000000000000000000 ) ) ;
#1908 = FACE_OUTER_BOUND ( 'NONE', #32205, .T. ) ;
#1909 = CARTESIAN_POINT ( 'NONE',  ( 2.604019713817498527, 32.15598440394879987, 2.846506069495843061 ) ) ;
#1910 = CARTESIAN_POINT ( 'NONE',  ( -33.45384370633241389, -29.82153911781839994, 31.38501356826949618 ) ) ;
#1911 = CARTESIAN_POINT ( 'NONE',  ( -12.00000000000001066, -60.99999999999997158, 154.9999999999999716 ) ) ;
#1912 =( NAMED_UNIT ( * ) PLANE_ANGLE_UNIT ( ) SI_UNIT ( $, .RADIAN. ) );
#1913 = ORIENTED_EDGE ( 'NONE', *, *, #29312, .T. ) ;
#1914 = FACE_OUTER_BOUND ( 'NONE', #15328, .T. ) ;
#1915 = LINE ( 'NONE', #23642, #16620 ) ;
#1916 = CYLINDRICAL_SURFACE ( 'NONE', #17762, 2.000000000000001776 ) ;
#1917 = VERTEX_POINT ( 'NONE', #17343 ) ;
#1918 = AXIS2_PLACEMENT_3D ( 'NONE', #33594, #9217, #16543 ) ;
#1919 = CARTESIAN_POINT ( 'NONE',  ( -20.00000000000001776, -109.0000000000000142, 187.0000000000000000 ) ) ;
#1920 = ORIENTED_EDGE ( 'NONE', *, *, #7383, .F. ) ;
#1921 = LINE ( 'NONE', #34144, #2363 ) ;
#1922 = EDGE_CURVE ( 'NONE', #3499, #33582, #12992, .T. ) ;
#1923 = DIRECTION ( 'NONE',  ( 0.000000000000000000, -5.145227585319922065E-49, -1.000000000000000000 ) ) ;
#1924 = AXIS2_PLACEMENT_3D ( 'NONE', #18205, #13387, #9998 ) ;
#1925 = VECTOR ( 'NONE', #4663, 1000.000000000000000 ) ;
#1926 = EDGE_CURVE ( 'NONE', #22879, #32966, #31662, .T. ) ;
#1927 = EDGE_CURVE ( 'NONE', #29708, #30081, #11821, .T. ) ;
#1928 = CIRCLE ( 'NONE', #7613, 3.999999999999976019 ) ;
#1929 = DIRECTION ( 'NONE',  ( -1.000000000000000000, 0.000000000000000000, -0.000000000000000000 ) ) ;
#1930 = FACE_OUTER_BOUND ( 'NONE', #28195, .T. ) ;
#1931 = CARTESIAN_POINT ( 'NONE',  ( -20.63749999999999929, 0.000000000000000000, 0.000000000000000000 ) ) ;
#1932 = AXIS2_PLACEMENT_3D ( 'NONE', #2031, #21071, #12909 ) ;
#1933 = EDGE_LOOP ( 'NONE', ( #3858, #9699, #27243, #315 ) ) ;
#1934 = EDGE_LOOP ( 'NONE', ( #11019, #16399, #2768, #7931 ) ) ;
#1935 = DIRECTION ( 'NONE',  ( -0.1063910735369017202, 0.9943243633099136947, -1.000770725407181676E-14 ) ) ;
#1936 =( REPRESENTATION_RELATIONSHIP ('NONE','NONE', #23037, #28231 ) REPRESENTATION_RELATIONSHIP_WITH_TRANSFORMATION ( #26024 )SHAPE_REPRESENTATION_RELATIONSHIP( ) );
#1937 = VERTEX_POINT ( 'NONE', #8953 ) ;
#1938 = EDGE_CURVE ( 'NONE', #5864, #27222, #9959, .T. ) ;
#1939 = CARTESIAN_POINT ( 'NONE',  ( 0.02407890056655564992, -30.46391896562403190, -6.211548095912885259 ) ) ;
#1940 = CIRCLE ( 'NONE', #9901, 32.54542015209057126 ) ;
#1941 = LINE ( 'NONE', #18343, #30370 ) ;
#1942 = CARTESIAN_POINT ( 'NONE',  ( 103.0920869195258689, -5.424061631995436450, 5.183681401394261812 ) ) ;
#1943 = CONTEXT_DEPENDENT_SHAPE_REPRESENTATION ( #14907, #31678 ) ;
#1944 = VERTEX_POINT ( 'NONE', #16991 ) ;
#1945 = LINE ( 'NONE', #6931, #34649 ) ;
#1946 = VECTOR ( 'NONE', #3218, 999.9999999999998863 ) ;
#1947 = EDGE_CURVE ( 'NONE', #32236, #1870, #22836, .T. ) ;
#1948 = ORIENTED_EDGE ( 'NONE', *, *, #31263, .F. ) ;
#1949 = ADVANCED_FACE ( 'NONE', ( #3780 ), #17900, .T. ) ;
#1951 = LINE ( 'NONE', #13005, #5578 ) ;
#1950 = LINE ( 'NONE', #14801, #10474 ) ;
#1952 = EDGE_CURVE ( 'NONE', #32238, #7140, #20145, .T. ) ;
#1953 = ORIENTED_EDGE ( 'NONE', *, *, #9611, .T. ) ;
#1954 = ORIENTED_EDGE ( 'NONE', *, *, #14723, .F. ) ;
#1955 = VECTOR ( 'NONE', #34547, 1000.000000000000000 ) ;
#1956 = CARTESIAN_POINT ( 'NONE',  ( 2.265105787010242011, 21.86923048072728548, -25.21799932878511896 ) ) ;
#1957 = ORIENTED_EDGE ( 'NONE', *, *, #8248, .F. ) ;
#1958 = VECTOR ( 'NONE', #30308, 1000.000000000000000 ) ;
#1959 = EDGE_CURVE ( 'NONE', #15766, #27456, #3071, .T. ) ;
#1960 = DIRECTION ( 'NONE',  ( 0.000000000000000000, 5.053935297177146739E-49, 1.000000000000000000 ) ) ;
#1961 = LINE ( 'NONE', #18878, #10317 ) ;
#1962 = ORIENTED_EDGE ( 'NONE', *, *, #24634, .F. ) ;
#1963 = DIRECTION ( 'NONE',  ( 0.000000000000000000, 0.000000000000000000, 1.000000000000000000 ) ) ;
#1964 = ORIENTED_EDGE ( 'NONE', *, *, #8386, .F. ) ;
#1965 = DIRECTION ( 'NONE',  ( -1.000000000000000000, -0.000000000000000000, -0.000000000000000000 ) ) ;
#1966 = DIRECTION ( 'NONE',  ( 0.000000000000000000, 0.000000000000000000, 1.000000000000000000 ) ) ;
#1967 = DIRECTION ( 'NONE',  ( -0.000000000000000000, -0.000000000000000000, -1.000000000000000000 ) ) ;
#1969 = FACE_OUTER_BOUND ( 'NONE', #30427, .T. ) ;
#1968 = DIRECTION ( 'NONE',  ( -1.000000000000000000, 0.000000000000000000, 0.000000000000000000 ) ) ;
#1970 = CIRCLE ( 'NONE', #33813, 7.999999999999979572 ) ;
#1971 = ADVANCED_FACE ( 'NONE', ( #30496 ), #4424, .T. ) ;
#1972 = EDGE_CURVE ( 'NONE', #7819, #30998, #34340, .T. ) ;
#1973 = DIRECTION ( 'NONE',  ( -0.1081190184239419622, 0.9941379571543595972, 0.000000000000000000 ) ) ;
#1974 = DIRECTION ( 'NONE',  ( -1.000000000000000000, -0.000000000000000000, -0.000000000000000000 ) ) ;
#1975 = DIRECTION ( 'NONE',  ( 0.000000000000000000, 0.000000000000000000, -1.000000000000000000 ) ) ;
#1976 = DIRECTION ( 'NONE',  ( -0.9635499925192230197, 0.2675283385292205329, 0.000000000000000000 ) ) ;
#1977 = AXIS2_PLACEMENT_3D ( 'NONE', #17267, #14592, #22231 ) ;
#1978 = ORIENTED_EDGE ( 'NONE', *, *, #20074, .T. ) ;
#1980 = ORIENTED_EDGE ( 'NONE', *, *, #27672, .T. ) ;
#1979 = AXIS2_PLACEMENT_3D ( 'NONE', #25827, #34190, #22993 ) ;
#1981 = AXIS2_PLACEMENT_3D ( 'NONE', #3376, #20293, #6747 ) ;
#1982 = EDGE_LOOP ( 'NONE', ( #31595, #16984, #9012, #11873, #16346, #19167 ) ) ;
#1983 = ORIENTED_EDGE ( 'NONE', *, *, #4996, .T. ) ;
#1984 = FACE_OUTER_BOUND ( 'NONE', #24660, .T. ) ;
#1985 = DIRECTION ( 'NONE',  ( 0.000000000000000000, -1.000000000000000000, 0.000000000000000000 ) ) ;
#1986 = ORIENTED_EDGE ( 'NONE', *, *, #5359, .T. ) ;
#1987 = ORIENTED_EDGE ( 'NONE', *, *, #29412, .T. ) ;
#1988 = ORIENTED_EDGE ( 'NONE', *, *, #29206, .F. ) ;
#1989 = DIRECTION ( 'NONE',  ( 0.000000000000000000, 1.000000000000000000, -1.224646799147353207E-16 ) ) ;
#1990 = EDGE_CURVE ( 'NONE', #17916, #31492, #14309, .T. ) ;
#1991 = CONTEXT_DEPENDENT_SHAPE_REPRESENTATION ( #17201, #5327 ) ;
#1992 = ADVANCED_FACE ( 'NONE', ( #7270 ), #25133, .T. ) ;
#1993 = AXIS2_PLACEMENT_3D ( 'NONE', #12689, #29576, #10002 ) ;
#1994 = ORIENTED_EDGE ( 'NONE', *, *, #19502, .T. ) ;
#1995 = DIRECTION ( 'NONE',  ( 0.3193015301359802827, 0.9476531711828023452, 0.000000000000000000 ) ) ;
#1996 = DIRECTION ( 'NONE',  ( 0.000000000000000000, -0.000000000000000000, -1.000000000000000000 ) ) ;
#1997 = ORIENTED_EDGE ( 'NONE', *, *, #1696, .T. ) ;
#1998 = ORIENTED_EDGE ( 'NONE', *, *, #14607, .F. ) ;
#1999 = DIRECTION ( 'NONE',  ( -1.000000000000000000, 0.000000000000000000, 0.000000000000000000 ) ) ;
#2000 = AXIS2_PLACEMENT_3D ( 'NONE', #20065, #34275, #9891 ) ;
#2001 = CARTESIAN_POINT ( 'NONE',  ( 2.790000000000080860, 27.73561032191001274, -12.87169219037303236 ) ) ;
#2002 = CARTESIAN_POINT ( 'NONE',  ( -5.491809612354312087, 32.07872192057775607, -36.68877005347593467 ) ) ;
#2003 = CARTESIAN_POINT ( 'NONE',  ( 1.040000000000000924, 14.89726405156217126, 31.02351007835982344 ) ) ;
#2004 = CARTESIAN_POINT ( 'NONE',  ( -8.267476927982274404, 31.47782073335738673, 68.31122994652405112 ) ) ;
#2005 = ORIENTED_EDGE ( 'NONE', *, *, #446, .F. ) ;
#2006 = DIRECTION ( 'NONE',  ( -1.000000000000000000, 0.000000000000000000, -5.546364386991661285E-52 ) ) ;
#2007 = CARTESIAN_POINT ( 'NONE',  ( -35.71762877834949990, -12.58147180936567011, 68.31122994652405112 ) ) ;
#2008 = VECTOR ( 'NONE', #30745, 1000.000000000000227 ) ;
#2009 = ORIENTED_EDGE ( 'NONE', *, *, #7383, .T. ) ;
#2010 = ADVANCED_FACE ( 'NONE', ( #17162 ), #12824, .F. ) ;
#2011 = AXIS2_PLACEMENT_3D ( 'NONE', #23063, #33908, #20391 ) ;
#2012 = CLOSED_SHELL ( 'NONE', ( #34325, #26112, #26388, #31073, #14924, #33339, #520, #9363, #1520, #23091, #13003, #18943, #31759, #33948, #20338, #28285, #26628, #15262 ) ) ;
#2013 = CARTESIAN_POINT ( 'NONE',  ( 0.07098929342602722237, -24.04031276246357152, -20.65449384219786211 ) ) ;
#2014 = LINE ( 'NONE', #13059, #20110 ) ;
#2015 = CARTESIAN_POINT ( 'NONE',  ( 109.5206256355305214, 3.553124229080486085, -6.613494096335986505 ) ) ;
#2017 = CARTESIAN_POINT ( 'NONE',  ( -108.1229279508730627, 4.063889691276223459, -6.307349793299454888 ) ) ;
#2016 = CARTESIAN_POINT ( 'NONE',  ( 22.89764159710613001, 4.274639749586560455, -77.50000000000000000 ) ) ;
#2018 = AXIS2_PLACEMENT_3D ( 'NONE', #25544, #30893, #9697 ) ;
#2019 = LINE ( 'NONE', #26054, #20664 ) ;
#2020 = ORIENTED_EDGE ( 'NONE', *, *, #34727, .T. ) ;
#2021 = CARTESIAN_POINT ( 'NONE',  ( 110.7380848894536598, 7.027143731242819742E-16, -12.50000000000000000 ) ) ;
#2023 = CARTESIAN_POINT ( 'NONE',  ( -35.00000000000000000, 11.30824010203865271, -28.57494248152495331 ) ) ;
#2022 = PLANE ( 'NONE',  #23453 ) ;
#2024 = CIRCLE ( 'NONE', #9434, 7.500000000000000000 ) ;
#2025 = ORIENTED_EDGE ( 'NONE', *, *, #17902, .T. ) ;
#2026 = CARTESIAN_POINT ( 'NONE',  ( 2.789999999999999147, -13.59935610937951900, -28.90010281771846223 ) ) ;
#2027 = EDGE_CURVE ( 'NONE', #17138, #4598, #10484, .T. ) ;
#2028 = TOROIDAL_SURFACE ( 'NONE', #3167, 30.47050528711511674, 8.000000000000000000 ) ;
#2029 = ORIENTED_EDGE ( 'NONE', *, *, #6051, .T. ) ;
#2030 = ORIENTED_EDGE ( 'NONE', *, *, #10622, .T. ) ;
#2031 = CARTESIAN_POINT ( 'NONE',  ( -12.00000000000001066, -137.0000000000000000, -155.0000000000000284 ) ) ;
#2032 = VERTEX_POINT ( 'NONE', #32012 ) ;
#2033 = ORIENTED_EDGE ( 'NONE', *, *, #1761, .T. ) ;
#2034 = DIRECTION ( 'NONE',  ( -5.546364386991661285E-52, 0.000000000000000000, -1.000000000000000000 ) ) ;
#2035 = AXIS2_PLACEMENT_3D ( 'NONE', #23508, #6950, #9472 ) ;
#2036 = EDGE_CURVE ( 'NONE', #5629, #3012, #1511, .T. ) ;
#2037 = EDGE_CURVE ( 'NONE', #109, #31150, #1941, .T. ) ;
#2038 = CIRCLE ( 'NONE', #10022, 7.999999999999979572 ) ;
#2039 = EDGE_CURVE ( 'NONE', #17702, #15632, #27034, .T. ) ;
#2040 = FACE_OUTER_BOUND ( 'NONE', #35068, .T. ) ;
#2041 = CARTESIAN_POINT ( 'NONE',  ( 0.02407890056655825201, -23.70329957282570632, -20.11932597908854703 ) ) ;
#2042 = ORIENTED_EDGE ( 'NONE', *, *, #610, .T. ) ;
#2043 = VERTEX_POINT ( 'NONE', #34883 ) ;
#2044 = DIRECTION ( 'NONE',  ( -0.000000000000000000, 1.836970198721029688E-16, -1.000000000000000000 ) ) ;
#2045 = DIRECTION ( 'NONE',  ( -0.000000000000000000, -0.000000000000000000, 1.000000000000000000 ) ) ;
#2046 = DIRECTION ( 'NONE',  ( 0.000000000000000000, 0.000000000000000000, 1.000000000000000000 ) ) ;
#2047 = DIRECTION ( 'NONE',  ( -1.000000000000000000, 0.000000000000000000, 0.000000000000000000 ) ) ;
#2048 = PLANE ( 'NONE',  #630 ) ;
#2049 = UNCERTAINTY_MEASURE_WITH_UNIT (LENGTH_MEASURE( 1.000000000000000082E-05 ), #3564, 'distance_accuracy_value', 'NONE');
#2050 = ORIENTED_EDGE ( 'NONE', *, *, #31346, .T. ) ;
#2051 = EDGE_LOOP ( 'NONE', ( #4526, #33909, #32838, #13816 ) ) ;
#2052 = VECTOR ( 'NONE', #32977, 1000.000000000000000 ) ;
#2053 = DIRECTION ( 'NONE',  ( 0.000000000000000000, -1.000000000000000000, -2.309213040847544338E-50 ) ) ;
#2054 = LINE ( 'NONE', #34449, #3922 ) ;
#2055 = EDGE_LOOP ( 'NONE', ( #30550, #34729, #25241, #13654 ) ) ;
#2056 = VECTOR ( 'NONE', #12798, 1000.000000000000000 ) ;
#2057 = DIRECTION ( 'NONE',  ( 1.000000000000000000, 0.000000000000000000, -0.000000000000000000 ) ) ;
#2058 = DIRECTION ( 'NONE',  ( 0.000000000000000000, 0.000000000000000000, 1.000000000000000000 ) ) ;
#2059 = FACE_OUTER_BOUND ( 'NONE', #6196, .T. ) ;
#2060 = ORIENTED_EDGE ( 'NONE', *, *, #14332, .F. ) ;
#2061 = DIRECTION ( 'NONE',  ( 0.000000000000000000, 0.000000000000000000, 1.000000000000000000 ) ) ;
#2062 = ORIENTED_EDGE ( 'NONE', *, *, #16987, .T. ) ;
#2063 = DIRECTION ( 'NONE',  ( 1.000000000000000000, 0.000000000000000000, -0.000000000000000000 ) ) ;
#2064 = ORIENTED_EDGE ( 'NONE', *, *, #25749, .F. ) ;
#2066 = LINE ( 'NONE', #12581, #3177 ) ;
#2065 = CARTESIAN_POINT ( 'NONE',  ( -500.0000000000000000, -109.0000000000000142, 162.9999999999999716 ) ) ;
#2067 = CIRCLE ( 'NONE', #16283, 2.525000000000003020 ) ;
#2068 = ORIENTED_EDGE ( 'NONE', *, *, #12031, .T. ) ;
#2069 = CARTESIAN_POINT ( 'NONE',  ( 0.000000000000000000, 0.000000000000000000, 3.180000000000000160 ) ) ;
#2070 = CARTESIAN_POINT ( 'NONE',  ( 11.99999999999999645, -137.0000000000000000, 155.0000000000000000 ) ) ;
#2071 = VERTEX_POINT ( 'NONE', #2465 ) ;
#2072 = VECTOR ( 'NONE', #26157, 1000.000000000000000 ) ;
#2073 = DIRECTION ( 'NONE',  ( -7.893605728314051750E-14, 1.618803117314786530E-15, 1.000000000000000000 ) ) ;
#2074 = EDGE_CURVE ( 'NONE', #21429, #4511, #10494, .T. ) ;
#2075 = ORIENTED_EDGE ( 'NONE', *, *, #29949, .F. ) ;
#2076 = DIRECTION ( 'NONE',  ( 0.000000000000000000, 0.000000000000000000, 1.000000000000000000 ) ) ;
#2077 = ORIENTED_EDGE ( 'NONE', *, *, #10363, .F. ) ;
#2078 = AXIS2_PLACEMENT_3D ( 'NONE', #14512, #5581, #19673 ) ;
#2079 = CYLINDRICAL_SURFACE ( 'NONE', #24675, 4.750000000000004441 ) ;
#2080 = ADVANCED_FACE ( 'NONE', ( #2647 ), #4955, .F. ) ;
#2081 = CARTESIAN_POINT ( 'NONE',  ( -361.0000000000000000, -125.0000000000000284, 164.9999999999999716 ) ) ;
#2082 = B_SPLINE_CURVE_WITH_KNOTS ( 'NONE', 3,
 ( #2722, #26446, #34958, #8239 ),
 .UNSPECIFIED., .F., .F.,
 ( 4, 4 ),
 ( 1.979774382698240400E-07, 0.0006879336733830264785 ),
 .UNSPECIFIED. ) ;
#2083 = EDGE_CURVE ( 'NONE', #2208, #15011, #18447, .T. ) ;
#2084 = CARTESIAN_POINT ( 'NONE',  ( -1.155000000000000027, 0.000000000000000000, 3.931000000000000494 ) ) ;
#2085 = DIRECTION ( 'NONE',  ( 0.000000000000000000, 0.000000000000000000, 1.000000000000000000 ) ) ;
#2086 = VERTEX_POINT ( 'NONE', #10135 ) ;
#2087 = ORIENTED_EDGE ( 'NONE', *, *, #26225, .T. ) ;
#2088 = VERTEX_POINT ( 'NONE', #7978 ) ;
#2089 = EDGE_CURVE ( 'NONE', #20006, #22497, #10840, .T. ) ;
#2090 = DIRECTION ( 'NONE',  ( 0.000000000000000000, 0.000000000000000000, -1.000000000000000000 ) ) ;
#2091 = VECTOR ( 'NONE', #12539, 1000.000000000000000 ) ;
#2092 = CARTESIAN_POINT ( 'NONE',  ( 15.99999999999998579, 4.559999999999909015, -168.2400000000000091 ) ) ;
#2093 = CARTESIAN_POINT ( 'NONE',  ( -23.46927268871045058, -22.54767421130284077, 68.31122994652405112 ) ) ;
#2094 = PLANE ( 'NONE',  #104 ) ;
#2095 = DIRECTION ( 'NONE',  ( 0.000000000000000000, -1.000000000000000000, 0.000000000000000000 ) ) ;
#2096 = FACE_OUTER_BOUND ( 'NONE', #14350, .T. ) ;
#2097 = VERTEX_POINT ( 'NONE', #21686 ) ;
#2098 = PRODUCT_DEFINITION_SHAPE ( 'NONE', 'NONE',  #35187 ) ;
#2099 = AXIS2_PLACEMENT_3D ( 'NONE', #20150, #16970, #22465 ) ;
#2100 = DIRECTION ( 'NONE',  ( 1.000000000000000000, 0.000000000000000000, -0.000000000000000000 ) ) ;
#2101 = EDGE_CURVE ( 'NONE', #14860, #30400, #4774, .T. ) ;
#2102 = DIRECTION ( 'NONE',  ( 0.4198891015602645438, -0.9075754196709570065, -0.000000000000000000 ) ) ;
#2103 = DIRECTION ( 'NONE',  ( 0.000000000000000000, 2.309213040847544338E-50, 1.000000000000000000 ) ) ;
#2104 = ORIENTED_EDGE ( 'NONE', *, *, #27915, .T. ) ;
#2105 = CIRCLE ( 'NONE', #10052, 7.999999999999979572 ) ;
#2106 = CARTESIAN_POINT ( 'NONE',  ( 15.99999999999998579, -124.9999999999999432, -186.9999999999999716 ) ) ;
#2107 = EDGE_LOOP ( 'NONE', ( #4532, #34179, #24526, #34171 ) ) ;
#2108 = CARTESIAN_POINT ( 'NONE',  ( 2.719051671025304984, -24.04001846604966630, -20.65402650742342061 ) ) ;
#2109 = CARTESIAN_POINT ( 'NONE',  ( 0.000000000000000000, 33.69708579775584667, -49.43553178847298568 ) ) ;
#2110 = ORIENTED_EDGE ( 'NONE', *, *, #1080, .T. ) ;
#2111 = DIRECTION ( 'NONE',  ( 1.000000000000000000, 3.469446951953834515E-18, 0.000000000000000000 ) ) ;
#2112 = CARTESIAN_POINT ( 'NONE',  ( -499.9999999999999432, 112.9999999999999574, -162.9999999999999716 ) ) ;
#2113 = CARTESIAN_POINT ( 'NONE',  ( 0.000000000000000000, 2.515464910414410839E-14, -49.43553178847298568 ) ) ;
#2114 = ORIENTED_EDGE ( 'NONE', *, *, #34192, .F. ) ;
#2115 = VERTEX_POINT ( 'NONE', #26503 ) ;
#2116 = DIRECTION ( 'NONE',  ( -0.1063910735369017202, 0.9943243633099136947, -1.000770725407181676E-14 ) ) ;
#2117 = EDGE_LOOP ( 'NONE', ( #2255, #11135, #14646, #758, #24030, #12999 ) ) ;
#2118 = FACE_OUTER_BOUND ( 'NONE', #32218, .T. ) ;
#2119 = DIRECTION ( 'NONE',  ( -0.000000000000000000, -0.000000000000000000, -1.000000000000000000 ) ) ;
#2120 = VECTOR ( 'NONE', #21830, 1000.000000000000000 ) ;
#2121 = AXIS2_PLACEMENT_3D ( 'NONE', #8045, #23887, #24240 ) ;
#2122 = DIRECTION ( 'NONE',  ( -1.000000000000000000, -0.000000000000000000, -0.000000000000000000 ) ) ;
#2123 = CARTESIAN_POINT ( 'NONE',  ( 104.6067242497968834, -5.728011724833245388, 4.841576811596270069 ) ) ;
#2124 = ORIENTED_EDGE ( 'NONE', *, *, #24437, .T. ) ;
#2125 = EDGE_CURVE ( 'NONE', #17537, #5382, #32535, .T. ) ;
#2126 = LINE ( 'NONE', #3647, #6152 ) ;
#2127 = EDGE_CURVE ( 'NONE', #26408, #23670, #4212, .T. ) ;
#2128 = AXIS2_PLACEMENT_3D ( 'NONE', #4393, #12961, #1736 ) ;
#2130 = CARTESIAN_POINT ( 'NONE',  ( -20.02113311122498729, -1.691831803474591833, -67.50000000000000000 ) ) ;
#2129 = DIRECTION ( 'NONE',  ( 0.000000000000000000, 1.836970198721029441E-16, -1.000000000000000000 ) ) ;
#2131 = ORIENTED_EDGE ( 'NONE', *, *, #19818, .T. ) ;
#2132 = EDGE_LOOP ( 'NONE', ( #22132, #26725, #26763, #30796, #23754, #18166, #9844, #10548, #18223 ) ) ;
#2133 = EDGE_CURVE ( 'NONE', #26553, #30412, #7059, .T. ) ;
#2134 = EDGE_CURVE ( 'NONE', #20509, #30714, #33214, .T. ) ;
#2135 = DIRECTION ( 'NONE',  ( -1.000000000000000000, -0.000000000000000000, -0.000000000000000000 ) ) ;
#2136 = EDGE_LOOP ( 'NONE', ( #15980, #30214, #23106, #20246 ) ) ;
#2137 = DIRECTION ( 'NONE',  ( -0.000000000000000000, -0.000000000000000000, 1.000000000000000000 ) ) ;
#2138 = CARTESIAN_POINT ( 'NONE',  ( -441.9999999999999432, -105.0000000000000142, 135.9999999999999716 ) ) ;
#2139 = EDGE_LOOP ( 'NONE', ( #20851, #13081, #25315, #33907, #19387, #18939, #11786, #25534 ) ) ;
#2140 = FACE_OUTER_BOUND ( 'NONE', #7438, .T. ) ;
#2141 = AXIS2_PLACEMENT_3D ( 'NONE', #28233, #6846, #28049 ) ;
#2142 = ORIENTED_EDGE ( 'NONE', *, *, #10636, .F. ) ;
#2143 = DIRECTION ( 'NONE',  ( 0.000000000000000000, 1.000000000000000000, 0.000000000000000000 ) ) ;
#2144 = DIRECTION ( 'NONE',  ( -8.433758354584418579E-81, 1.000000000000000000, 3.421138828918010427E-49 ) ) ;
#2145 = EDGE_CURVE ( 'NONE', #12065, #19610, #21352, .T. ) ;
#2146 = CARTESIAN_POINT ( 'NONE',  ( 0.006892420738473521713, 30.38148214875513631, -5.469007969453248741 ) ) ;
#2148 = CARTESIAN_POINT ( 'NONE',  ( -442.0000000000000000, -125.0000000000000000, 155.0000000000000000 ) ) ;
#2147 = DIRECTION ( 'NONE',  ( -0.000000000000000000, 1.000000000000000000, 0.000000000000000000 ) ) ;
#2149 = VECTOR ( 'NONE', #5904, 1000.000000000000000 ) ;
#2150 =( REPRESENTATION_RELATIONSHIP ('NONE','NONE', #23037, #15767 ) REPRESENTATION_RELATIONSHIP_WITH_TRANSFORMATION ( #3172 )SHAPE_REPRESENTATION_RELATIONSHIP( ) );
#2151 = CYLINDRICAL_SURFACE ( 'NONE', #19584, 16.00000000000000000 ) ;
#2152 = DIRECTION ( 'NONE',  ( 1.000000000000000000, 0.000000000000000000, 0.000000000000000000 ) ) ;
#2153 = LINE ( 'NONE', #34370, #8765 ) ;
#2154 = CARTESIAN_POINT ( 'NONE',  ( 2.765921099433443331, 18.59128259035506758, -24.91982945642901726 ) ) ;
#2155 = VECTOR ( 'NONE', #1176, 1000.000000000000000 ) ;
#2156 = ADVANCED_FACE ( 'NONE', ( #32197 ), #18526, .T. ) ;
#2157 = ORIENTED_EDGE ( 'NONE', *, *, #1003, .F. ) ;
#2158 = ADVANCED_FACE ( 'NONE', ( #26680 ), #13166, .F. ) ;
#2159 = DIRECTION ( 'NONE',  ( 2.631201909438060269E-14, -5.396010391056495992E-16, 0.9999999999999998890 ) ) ;
#2160 = EDGE_LOOP ( 'NONE', ( #17517, #12192, #1027, #11996 ) ) ;
#2161 = VERTEX_POINT ( 'NONE', #16902 ) ;
#2162 = CONICAL_SURFACE ( 'NONE', #12977, 12.50000000000000000, 0.7853981633974431720 ) ;
#2163 = DIRECTION ( 'NONE',  ( -1.000000000000000000, -0.000000000000000000, -0.000000000000000000 ) ) ;
#2164 = DIRECTION ( 'NONE',  ( 0.1063910735369155841, -0.9943243633099125844, -3.335902418025060287E-15 ) ) ;
#2165 = EDGE_LOOP ( 'NONE', ( #25285, #8276, #2405, #3867 ) ) ;
#2166 = ORIENTED_EDGE ( 'NONE', *, *, #23931, .T. ) ;
#2167 = DIRECTION ( 'NONE',  ( 1.000000000000000000, 0.000000000000000000, -0.000000000000000000 ) ) ;
#2168 = CARTESIAN_POINT ( 'NONE',  ( 2.604019716835467513, 21.49213631816418513, 24.08729967255630910 ) ) ;
#2169 = ITEM_DEFINED_TRANSFORMATION ( 'NONE', 'NONE', #24627,  #28566 ) ;
#2170 = LINE ( 'NONE', #17866, #19258 ) ;
#2171 = DIRECTION ( 'NONE',  ( -0.000000000000000000, 1.000000000000000000, -0.000000000000000000 ) ) ;
#2172 = ORIENTED_EDGE ( 'NONE', *, *, #16791, .F. ) ;
#2173 = ORIENTED_EDGE ( 'NONE', *, *, #3208, .T. ) ;
#2174 = EDGE_CURVE ( 'NONE', #18033, #11540, #23587, .T. ) ;
#2175 = ADVANCED_FACE ( 'NONE', ( #27731 ), #30407, .F. ) ;
#2176 = CARTESIAN_POINT ( 'NONE',  ( 11.99999999999999645, 140.9999999999999716, -175.0000000000000284 ) ) ;
#2177 = DIRECTION ( 'NONE',  ( -1.000000000000000000, -0.000000000000000000, -0.000000000000000000 ) ) ;
#2178 = DIRECTION ( 'NONE',  ( -1.000000000000000000, 0.000000000000000000, 0.000000000000000000 ) ) ;
#2179 = CARTESIAN_POINT ( 'NONE',  ( -442.0000000000000000, 105.0000000000000142, 100.0000000000000000 ) ) ;
#2180 = DIRECTION ( 'NONE',  ( 0.000000000000000000, 1.131431318426415506E-52, 1.000000000000000000 ) ) ;
#2181 = VERTEX_POINT ( 'NONE', #29884 ) ;
#2182 = PLANE ( 'NONE',  #19747 ) ;
#2183 = CARTESIAN_POINT ( 'NONE',  ( -130.6469666100234406, 6.000000000000000000, 62.49999999999999289 ) ) ;
#2184 = CARTESIAN_POINT ( 'NONE',  ( 212.5000000000000000, 0.000000000000000000, 7.500000000000000000 ) ) ;
#2185 = CARTESIAN_POINT ( 'NONE',  ( -345.0000000000000000, -125.0000000000000284, 126.0000000000000000 ) ) ;
#2186 = AXIS2_PLACEMENT_3D ( 'NONE', #8358, #32550, #24193 ) ;
#2187 = DIRECTION ( 'NONE',  ( -1.000000000000000000, -0.000000000000000000, -0.000000000000000000 ) ) ;
#2189 = DIRECTION ( 'NONE',  ( 0.000000000000000000, 0.000000000000000000, 1.000000000000000000 ) ) ;
#2188 = CARTESIAN_POINT ( 'NONE',  ( -20.00000000000007461, 112.9999999999999574, 159.0000000000000000 ) ) ;
#2190 = AXIS2_PLACEMENT_3D ( 'NONE', #27959, #9270, #6407 ) ;
#2191 = CARTESIAN_POINT ( 'NONE',  ( 1.749999999999999778, 27.68252950111368094, -20.44661865013457458 ) ) ;
#2192 = ORIENTED_EDGE ( 'NONE', *, *, #4524, .T. ) ;
#2193 = CYLINDRICAL_SURFACE ( 'NONE', #11633, 3.999999999999976019 ) ;
#2195 = FACE_OUTER_BOUND ( 'NONE', #19836, .T. ) ;
#2194 = DIRECTION ( 'NONE',  ( -1.000000000000000000, 0.000000000000000000, 0.000000000000000000 ) ) ;
#2196 = EDGE_CURVE ( 'NONE', #2517, #13256, #7869, .T. ) ;
#2197 = EDGE_CURVE ( 'NONE', #6435, #26862, #5936, .T. ) ;
#2198 = ADVANCED_FACE ( 'NONE', ( #6004 ), #13911, .T. ) ;
#2199 = ORIENTED_EDGE ( 'NONE', *, *, #6355, .F. ) ;
#2200 = DIRECTION ( 'NONE',  ( 0.000000000000000000, 0.000000000000000000, 1.000000000000000000 ) ) ;
#2201 = PRODUCT_DEFINITION_SHAPE ( 'NONE', 'NONE',  #35233 ) ;
#2202 = EDGE_CURVE ( 'NONE', #9416, #13484, #32718, .T. ) ;
#2203 = ORIENTED_EDGE ( 'NONE', *, *, #4582, .F. ) ;
#2204 = AXIS2_PLACEMENT_3D ( 'NONE', #21496, #307, #5793 ) ;
#2205 = EDGE_CURVE ( 'NONE', #15586, #8663, #6504, .T. ) ;
#2206 = VERTEX_POINT ( 'NONE', #27554 ) ;
#2207 = CARTESIAN_POINT ( 'NONE',  ( 143.0000000000000568, -175.8248315648716016, -46.05325008164005851 ) ) ;
#2208 = VERTEX_POINT ( 'NONE', #33062 ) ;
#2209 = ORIENTED_EDGE ( 'NONE', *, *, #4188, .T. ) ;
#2210 = FACE_BOUND ( 'NONE', #20490, .T. ) ;
#2211 = CIRCLE ( 'NONE', #17010, 32.54542015209056416 ) ;
#2212 = DIRECTION ( 'NONE',  ( 0.000000000000000000, -0.000000000000000000, -1.000000000000000000 ) ) ;
#2213 = DIRECTION ( 'NONE',  ( -1.000000000000000000, 0.000000000000000000, 0.000000000000000000 ) ) ;
#2214 = VERTEX_POINT ( 'NONE', #22221 ) ;
#2215 = ORIENTED_EDGE ( 'NONE', *, *, #2461, .F. ) ;
#2216 = LINE ( 'NONE', #23916, #17432 ) ;
#2217 = CARTESIAN_POINT ( 'NONE',  ( 0.02407890056655564992, -30.46391896562403190, -6.211548095912885259 ) ) ;
#2218 = DIRECTION ( 'NONE',  ( -0.000000000000000000, -0.000000000000000000, 1.000000000000000000 ) ) ;
#2219 = CARTESIAN_POINT ( 'NONE',  ( 15.99999999999998579, 112.9999999999999574, -175.0000000000000284 ) ) ;
#2220 = FACE_OUTER_BOUND ( 'NONE', #13490, .T. ) ;
#2221 = ORIENTED_EDGE ( 'NONE', *, *, #29603, .F. ) ;
#2222 = CIRCLE ( 'NONE', #19876, 32.54542015209055705 ) ;
#2223 = DIRECTION ( 'NONE',  ( -0.000000000000000000, 1.000000000000000000, -0.000000000000000000 ) ) ;
#2224 = LINE ( 'NONE', #23927, #4468 ) ;
#2225 = ORIENTED_EDGE ( 'NONE', *, *, #7608, .T. ) ;
#2226 = DIRECTION ( 'NONE',  ( 0.000000000000000000, -1.000000000000000000, 0.000000000000000000 ) ) ;
#2227 = DIRECTION ( 'NONE',  ( 3.040835319149746090E-31, 1.000000000000000000, 0.000000000000000000 ) ) ;
#2228 = CARTESIAN_POINT ( 'NONE',  ( 2.033589660436532220, -9.974843919189428476, 32.41553303492214866 ) ) ;
#2229 = ORIENTED_EDGE ( 'NONE', *, *, #4752, .T. ) ;
#2230 = VECTOR ( 'NONE', #34272, 1000.000000000000000 ) ;
#2231 = DIRECTION ( 'NONE',  ( -1.000000000000000000, 0.000000000000000000, 0.000000000000000000 ) ) ;
#2232 = ORIENTED_EDGE ( 'NONE', *, *, #32979, .F. ) ;
#2233 = CARTESIAN_POINT ( 'NONE',  ( -418.0000000000000000, -124.9999999999999716, 139.9999999999999716 ) ) ;
#2234 = VERTEX_POINT ( 'NONE', #24516 ) ;
#2236 = CARTESIAN_POINT ( 'NONE',  ( 23.31255882915079880, -22.70966696615090896, 68.31122994652405112 ) ) ;
#2235 = DIRECTION ( 'NONE',  ( 1.000000000000000000, -0.000000000000000000, -0.000000000000000000 ) ) ;
#2237 = DIRECTION ( 'NONE',  ( -0.000000000000000000, 1.836970198721029688E-16, -1.000000000000000000 ) ) ;
#2238 = EDGE_CURVE ( 'NONE', #19731, #10008, #8685, .T. ) ;
#2239 = EDGE_CURVE ( 'NONE', #18709, #27398, #3345, .T. ) ;
#2240 = AXIS2_PLACEMENT_3D ( 'NONE', #7866, #23538, #34222 ) ;
#2241 = ORIENTED_EDGE ( 'NONE', *, *, #34180, .T. ) ;
#2242 = DIRECTION ( 'NONE',  ( 0.000000000000000000, 0.000000000000000000, -1.000000000000000000 ) ) ;
#2243 = DIRECTION ( 'NONE',  ( 0.000000000000000000, -0.000000000000000000, 1.000000000000000000 ) ) ;
#2244 = EDGE_LOOP ( 'NONE', ( #4738, #4058, #9492, #10473 ) ) ;
#2245 = CARTESIAN_POINT ( 'NONE',  ( 758.0758068150074678, 1326.829654430702021, 1753.598338701303874 ) ) ;
#2246 = ORIENTED_EDGE ( 'NONE', *, *, #26521, .T. ) ;
#2247 = DIRECTION ( 'NONE',  ( 0.000000000000000000, 0.000000000000000000, 1.000000000000000000 ) ) ;
#2248 = ORIENTED_EDGE ( 'NONE', *, *, #8887, .F. ) ;
#2249 = CARTESIAN_POINT ( 'NONE',  ( -445.9999999999999432, 137.0000000000000000, -175.0000000000000000 ) ) ;
#2250 = AXIS2_PLACEMENT_3D ( 'NONE', #28082, #22575, #33416 ) ;
#2251 = PRESENTATION_STYLE_ASSIGNMENT (( #2598 ) ) ;
#2252 = CARTESIAN_POINT ( 'NONE',  ( -101.1679389503612612, -3.403480489512942686, -6.688370467007151099 ) ) ;
#2253 = CYLINDRICAL_SURFACE ( 'NONE', #13690, 7.999999999999979572 ) ;
#2254 = VERTEX_POINT ( 'NONE', #21863 ) ;
#2255 = ORIENTED_EDGE ( 'NONE', *, *, #8623, .F. ) ;
#2256 = ORIENTED_EDGE ( 'NONE', *, *, #9336, .T. ) ;
#2257 = DIRECTION ( 'NONE',  ( -1.000000000000000000, 0.000000000000000000, 0.000000000000000000 ) ) ;
#2258 = CARTESIAN_POINT ( 'NONE',  ( 2.789999999999999147, 2.005524111408653720, -31.87689292423236154 ) ) ;
#2259 = CARTESIAN_POINT ( 'NONE',  ( -418.0000000000000000, -141.0000000000000000, 154.9999999999999716 ) ) ;
#2260 = CARTESIAN_POINT ( 'NONE',  ( -35.00000000000000000, 11.30824010203864205, 68.31122994652405112 ) ) ;
#2261 = PLANE ( 'NONE',  #2939 ) ;
#2262 = LINE ( 'NONE', #13136, #15790 ) ;
#2263 = LINE ( 'NONE', #10985, #15880 ) ;
#2264 = ORIENTED_EDGE ( 'NONE', *, *, #32975, .F. ) ;
#2265 = LINE ( 'NONE', #8133, #24224 ) ;
#2266 = CARTESIAN_POINT ( 'NONE',  ( 0.7564103367120450505, 27.74660763222631132, -19.50359089280043534 ) ) ;
#2267 = CARTESIAN_POINT ( 'NONE',  ( 2.719051659750488792, 28.92406410882585277, -12.95800229409215909 ) ) ;
#2268 = ORIENTED_EDGE ( 'NONE', *, *, #1972, .T. ) ;
#2269 = CYLINDRICAL_SURFACE ( 'NONE', #31981, 5.738084889453667792 ) ;
#2270 = ORIENTED_EDGE ( 'NONE', *, *, #27716, .T. ) ;
#2271 = DIRECTION ( 'NONE',  ( 0.000000000000000000, 1.000000000000000000, 0.000000000000000000 ) ) ;
#2272 = EDGE_CURVE ( 'NONE', #23099, #33855, #19613, .T. ) ;
#2273 = FACE_OUTER_BOUND ( 'NONE', #27988, .T. ) ;
#2274 = TOROIDAL_SURFACE ( 'NONE', #27278, 30.47050528711511674, 8.000000000000000000 ) ;
#2275 = EDGE_CURVE ( 'NONE', #19944, #30605, #32892, .T. ) ;
#2276 = ORIENTED_EDGE ( 'NONE', *, *, #10213, .T. ) ;
#2277 = CARTESIAN_POINT ( 'NONE',  ( -5.021133111225092982, -11.61907005722761532, -67.50000000000000000 ) ) ;
#2278 = LINE ( 'NONE', #2978, #14533 ) ;
#2280 = ADVANCED_FACE ( 'NONE', ( #25047, #33251 ), #5649, .T. ) ;
#2279 = CYLINDRICAL_SURFACE ( 'NONE', #5773, 4.306175033202026547 ) ;
#2281 = ORIENTED_EDGE ( 'NONE', *, *, #25267, .T. ) ;
#2282 = ORIENTED_EDGE ( 'NONE', *, *, #5572, .F. ) ;
#2283 = DIRECTION ( 'NONE',  ( -7.893605728314050488E-14, 1.618803117314786135E-15, 0.9999999999999998890 ) ) ;
#2284 = ORIENTED_EDGE ( 'NONE', *, *, #8508, .F. ) ;
#2285 = DIRECTION ( 'NONE',  ( -0.000000000000000000, 1.000000000000000000, 0.000000000000000000 ) ) ;
#2286 = DIRECTION ( 'NONE',  ( 0.000000000000000000, 0.000000000000000000, -1.000000000000000000 ) ) ;
#2287 = CARTESIAN_POINT ( 'NONE',  ( -105.0000000000000000, 0.000000000000000000, 60.00000000000000000 ) ) ;
#2288 = CARTESIAN_POINT ( 'NONE',  ( 99.27229867161369725, -0.3974226492620277496, 7.492047161373153408 ) ) ;
#2289 = ORIENTED_EDGE ( 'NONE', *, *, #33790, .T. ) ;
#2290 = AXIS2_PLACEMENT_3D ( 'NONE', #22014, #33027, #29848 ) ;
#2291 = CARTESIAN_POINT ( 'NONE',  ( -442.0000000000000000, 124.9999999999999432, -162.9999999999999716 ) ) ;
#2292 = AXIS2_PLACEMENT_3D ( 'NONE', #17440, #20269, #11548 ) ;
#2294 = DIRECTION ( 'NONE',  ( 1.000000000000000000, 0.000000000000000000, 0.000000000000000000 ) ) ;
#2293 = DIRECTION ( 'NONE',  ( 0.8568571761675893850, 0.5155538571770216238, 9.470570714698666623E-17 ) ) ;
#2295 = VERTEX_POINT ( 'NONE', #11547 ) ;
#2296 = ORIENTED_EDGE ( 'NONE', *, *, #9919, .T. ) ;
#2297 = CARTESIAN_POINT ( 'NONE',  ( -449.9999999999999432, -105.0000000000000142, -174.9999999999999716 ) ) ;
#2298 = ORIENTED_EDGE ( 'NONE', *, *, #7538, .F. ) ;
#2299 = CYLINDRICAL_SURFACE ( 'NONE', #33443, 2.524999999999999467 ) ;
#2300 = DIRECTION ( 'NONE',  ( 0.000000000000000000, 1.000000000000000000, 2.465190328815662439E-32 ) ) ;
#2301 = ORIENTED_EDGE ( 'NONE', *, *, #21912, .F. ) ;
#2302 = CARTESIAN_POINT ( 'NONE',  ( -1.649999999999999911, 0.000000000000000000, 0.000000000000000000 ) ) ;
#2303 = AXIS2_PLACEMENT_3D ( 'NONE', #214, #8563, #11077 ) ;
#2304 = VECTOR ( 'NONE', #5071, 1000.000000000000000 ) ;
#2305 = FACE_OUTER_BOUND ( 'NONE', #6168, .T. ) ;
#2306 = ORIENTED_EDGE ( 'NONE', *, *, #2507, .T. ) ;
#2307 = DIRECTION ( 'NONE',  ( 3.697785493223492838E-32, 1.934419779023891545E-16, -1.000000000000000000 ) ) ;
#2308 = CARTESIAN_POINT ( 'NONE',  ( 2.789999999999999147, 23.28319895603578971, 21.86437915510226659 ) ) ;
#2309 = EDGE_CURVE ( 'NONE', #10302, #15568, #13862, .T. ) ;
#2310 = DIRECTION ( 'NONE',  ( 0.000000000000000000, 1.000000000000000000, -3.374343856708137958E-53 ) ) ;
#2312 = FACE_OUTER_BOUND ( 'NONE', #4217, .T. ) ;
#2311 = CARTESIAN_POINT ( 'NONE',  ( 0.5288002570077341424, -33.38088972941606869, -0.7716149733917129216 ) ) ;
#2313 = DIRECTION ( 'NONE',  ( 0.000000000000000000, 0.000000000000000000, -1.000000000000000000 ) ) ;
#2314 = CYLINDRICAL_SURFACE ( 'NONE', #26398, 11.22499999999999787 ) ;
#2315 = AXIS2_PLACEMENT_3D ( 'NONE', #13091, #31932, #28752 ) ;
#2317 = ADVANCED_FACE ( 'NONE', ( #3517 ), #25228, .T. ) ;
#2316 = CARTESIAN_POINT ( 'NONE',  ( 2.265105789152631388, 5.490830290249586909, 32.92508943594316406 ) ) ;
#2318 = ADVANCED_FACE ( 'NONE', ( #30223 ), #12261, .F. ) ;
#2319 = VECTOR ( 'NONE', #16286, 1000.000000000000000 ) ;
#2320 = VERTEX_POINT ( 'NONE', #22755 ) ;
#2321 = EDGE_CURVE ( 'NONE', #29803, #12309, #28615, .T. ) ;
#2322 = EDGE_CURVE ( 'NONE', #11932, #10023, #1388, .T. ) ;
#2323 = CARTESIAN_POINT ( 'NONE',  ( 129.3530333899765594, -6.000000000000000000, -57.49999999999999289 ) ) ;
#2324 = VERTEX_POINT ( 'NONE', #31282 ) ;
#2325 = ORIENTED_EDGE ( 'NONE', *, *, #5872, .T. ) ;
#2326 = EDGE_CURVE ( 'NONE', #34521, #2181, #27545, .T. ) ;
#2327 = VECTOR ( 'NONE', #11791, 1000.000000000000000 ) ;
#2328 = CARTESIAN_POINT ( 'NONE',  ( 110.6969072286498204, 0.7888478034546075879, 7.468363897292212172 ) ) ;
#2329 = CARTESIAN_POINT ( 'NONE',  ( 801.1656699447482879, 1369.357496751726330, 1753.598338701304101 ) ) ;
#2330 = AXIS2_PLACEMENT_3D ( 'NONE', #23825, #21512, #16361 ) ;
#2331 = ORIENTED_EDGE ( 'NONE', *, *, #3397, .F. ) ;
#2332 = VECTOR ( 'NONE', #17025, 1000.000000000000000 ) ;
#2333 = CIRCLE ( 'NONE', #11444, 7.999999999999979572 ) ;
#2334 = LINE ( 'NONE', #29039, #5391 ) ;
#2335 = DIRECTION ( 'NONE',  ( -0.000000000000000000, 1.836970198721029934E-16, -1.000000000000000000 ) ) ;
#2336 = B_SPLINE_CURVE_WITH_KNOTS ( 'NONE', 3,
 ( #9511, #12012, #8979, #28197 ),
 .UNSPECIFIED., .F., .F.,
 ( 4, 4 ),
 ( 2.038594426256260137E-07, 0.0006242955995025980349 ),
 .UNSPECIFIED. ) ;
#2337 = CARTESIAN_POINT ( 'NONE',  ( 9.199999999999999289, 0.000000000000000000, 0.000000000000000000 ) ) ;
#2338 = ORIENTED_EDGE ( 'NONE', *, *, #3646, .F. ) ;
#2339 = ORIENTED_EDGE ( 'NONE', *, *, #22792, .T. ) ;
#2340 = CARTESIAN_POINT ( 'NONE',  ( 1.040000000000001146, 6.183021911002323456, -33.85493898757056286 ) ) ;
#2342 = DIRECTION ( 'NONE',  ( 1.000000000000000000, 0.000000000000000000, 0.000000000000000000 ) ) ;
#2341 = CIRCLE ( 'NONE', #6887, 2.524999999999999467 ) ;
#2343 = LINE ( 'NONE', #9837, #2794 ) ;
#2344 = CARTESIAN_POINT ( 'NONE',  ( -7.176301005103106867, -1.505030548027689097, 3.180000000000000160 ) ) ;
#2345 = FACE_OUTER_BOUND ( 'NONE', #21509, .T. ) ;
#2346 = ORIENTED_EDGE ( 'NONE', *, *, #11507, .F. ) ;
#2347 = VECTOR ( 'NONE', #33690, 1000.000000000000000 ) ;
#2348 = PLANE ( 'NONE',  #23173 ) ;
#2349 = DIRECTION ( 'NONE',  ( 3.469446951953832974E-18, 1.000000000000000000, -7.888609052210118054E-31 ) ) ;
#2350 = CARTESIAN_POINT ( 'NONE',  ( 2.789999999999999147, 28.95078156989571383, -9.502838467757751317 ) ) ;
#2351 = APPLICATION_CONTEXT ( 'automotive_design' ) ;
#2352 = LINE ( 'NONE', #2184, #18636 ) ;
#2353 = PLANE ( 'NONE',  #8708 ) ;
#2354 = CARTESIAN_POINT ( 'NONE',  ( 11.99999999999999645, -109.0000000000000142, 174.9999999999999432 ) ) ;
#2356 = DIRECTION ( 'NONE',  ( 0.000000000000000000, 0.000000000000000000, -1.000000000000000000 ) ) ;
#2355 = FACE_OUTER_BOUND ( 'NONE', #25633, .T. ) ;
#2357 = AXIS2_PLACEMENT_3D ( 'NONE', #5981, #25023, #662 ) ;
#2358 = VECTOR ( 'NONE', #8325, 1000.000000000000000 ) ;
#2359 = CARTESIAN_POINT ( 'NONE',  ( 2.789999999999999147, -29.00730259674844902, 9.328884633908842261 ) ) ;
#2361 = ORIENTED_EDGE ( 'NONE', *, *, #23316, .F. ) ;
#2360 = AXIS2_PLACEMENT_3D ( 'NONE', #13291, #2588, #10616 ) ;
#2363 = VECTOR ( 'NONE', #7257, 1000.000000000000000 ) ;
#2362 = CARTESIAN_POINT ( 'NONE',  ( 105.1857752594875990, 5.738231822805251348, -11.10507521702373879 ) ) ;
#2364 = FACE_OUTER_BOUND ( 'NONE', #5108, .T. ) ;
#2365 = EDGE_CURVE ( 'NONE', #23877, #12319, #23112, .T. ) ;
#2366 = ORIENTED_EDGE ( 'NONE', *, *, #17822, .F. ) ;
#2367 = EDGE_CURVE ( 'NONE', #7970, #14594, #30963, .T. ) ;
#2368 = ADVANCED_FACE ( 'NONE', ( #4032 ), #26990, .T. ) ;
#2369 = CARTESIAN_POINT ( 'NONE',  ( 2.789999999999998703, -23.48484457444959972, 19.71282888652477538 ) ) ;
#2370 = VERTEX_POINT ( 'NONE', #31116 ) ;
#2371 = AXIS2_PLACEMENT_3D ( 'NONE', #4558, #7413, #5096 ) ;
#2372 = ORIENTED_EDGE ( 'NONE', *, *, #25340, .F. ) ;
#2373 = CARTESIAN_POINT ( 'NONE',  ( -3.250000000000000000, -5.838643359331793015, 0.000000000000000000 ) ) ;
#2374 = ORIENTED_EDGE ( 'NONE', *, *, #13917, .T. ) ;
#2375 = ORIENTED_EDGE ( 'NONE', *, *, #7992, .T. ) ;
#2376 = DIRECTION ( 'NONE',  ( 0.000000000000000000, 0.000000000000000000, 1.000000000000000000 ) ) ;
#2377 = EDGE_CURVE ( 'NONE', #25411, #173, #14928, .T. ) ;
#2378 = VECTOR ( 'NONE', #15660, 1000.000000000000000 ) ;
#2379 = CARTESIAN_POINT ( 'NONE',  ( 1.749999999999999778, 0.000000000000000000, 0.000000000000000000 ) ) ;
#2380 = DIRECTION ( 'NONE',  ( 0.000000000000000000, 0.000000000000000000, 1.000000000000000000 ) ) ;
#2381 = ORIENTED_EDGE ( 'NONE', *, *, #9348, .F. ) ;
#2382 = ORIENTED_EDGE ( 'NONE', *, *, #15611, .F. ) ;
#2383 = CARTESIAN_POINT ( 'NONE',  ( -418.0000000000000000, 105.0000000000000000, -77.99999999999997158 ) ) ;
#2384 = AXIS2_PLACEMENT_3D ( 'NONE', #23820, #10289, #31645 ) ;
#2385 = CARTESIAN_POINT ( 'NONE',  ( 29.63313772848250238, -13.45665341906703816, 68.31122994652405112 ) ) ;
#2386 = EDGE_CURVE ( 'NONE', #32063, #28687, #25581, .T. ) ;
#2387 = DIRECTION ( 'NONE',  ( 0.000000000000000000, 0.000000000000000000, 1.000000000000000000 ) ) ;
#2388 = CARTESIAN_POINT ( 'NONE',  ( 8.000000000000000000, 0.000000000000000000, 0.000000000000000000 ) ) ;
#2389 = EDGE_LOOP ( 'NONE', ( #23753, #18036, #25360, #34828 ) ) ;
#2390 = EDGE_CURVE ( 'NONE', #22410, #13078, #29117, .T. ) ;
#2391 = EDGE_CURVE ( 'NONE', #35, #29789, #12600, .T. ) ;
#2392 = CARTESIAN_POINT ( 'NONE',  ( -19.99999999999998934, -145.0000000000000000, 162.9999999999999716 ) ) ;
#2393 = CARTESIAN_POINT ( 'NONE',  ( -418.0000000000000000, -145.0000000000000000, -175.0000000000000000 ) ) ;
#2394 = ORIENTED_EDGE ( 'NONE', *, *, #29927, .T. ) ;
#2395 = CARTESIAN_POINT ( 'NONE',  ( -499.9999999999999432, 140.9999999999999716, 187.0000000000000000 ) ) ;
#2396 = ADVANCED_FACE ( 'NONE', ( #9578 ), #23281, .F. ) ;
#2397 = CARTESIAN_POINT ( 'NONE',  ( 2.789999999999999147, -20.35927063852824048, 24.61013060777164796 ) ) ;
#2398 = FACE_OUTER_BOUND ( 'NONE', #27764, .T. ) ;
#2399 = VERTEX_POINT ( 'NONE', #33596 ) ;
#2400 = CARTESIAN_POINT ( 'NONE',  ( -500.0000000000000000, -105.0000000000000142, 194.9999999999999716 ) ) ;
#2401 = ORIENTED_EDGE ( 'NONE', *, *, #25438, .T. ) ;
#2402 =( REPRESENTATION_RELATIONSHIP ('NONE','NONE', #23037, #8672 ) REPRESENTATION_RELATIONSHIP_WITH_TRANSFORMATION ( #15144 )SHAPE_REPRESENTATION_RELATIONSHIP( ) );
#2403 = CARTESIAN_POINT ( 'NONE',  ( 9.199999999999999289, 11.69134295108991672, 6.750000000000011546 ) ) ;
#2404 = CLOSED_SHELL ( 'NONE', ( #25394, #6924, #14172, #22095, #26228, #1731, #26540, #35035, #16608, #25299, #15205, #28724, #4289, #27001, #15151, #12148, #4929, #13693, #19058, #9481, #69, #34512, #16321, #14599, #31413, #11999, #19753, #32002, #23004, #15411, #3055, #26923, #26580, #33122, #3737, #31038, #1597, #10619, #18090, #8504, #33967, #11825, #8830, #26343, #22220, #9244, #16707, #31653, #1327, #17147, #8281, #18299, #5634, #5038, #29346, #14743, #34920, #10964, #3643, #1559, #24262, #7948, #25910, #11961, #11353, #9081, #14970, #8783, #19657, #12688, #19176, #33886, #1753, #9168, #6251, #2396, #25890, #11558, #9926, #19309, #2175, #27307, #32739, #23784, #11667, #3280, #22028, #8960, #25190, #25750, #3283, #1063, #30967, #1075, #27714, #11131, #19733, #7599, #18549, #8235, #523, #22645, #16829, #11553, #28897, #4609, #26023, #13580, #30168, #30537, #8458, #7412, #28021, #24, #27454, #31101, #6903, #17190, #26176, #8507, #14921, #12349, #17341, #4362, #25437, #20901, #18359, #24684, #15878, #26423, #5232, #4276, #17015, #22345, #3765, #11585, #23068, #30736, #28292, #33036, #4332, #10171, #18311, #12474, #34073, #16706, #12234, #11446, #1500, #28458, #8074, #3417, #28373, #11709, #20681, #24566, #24063, #33436, #31962, #30889, #2731, #28259, #34780, #29251, #8678, #16855, #32424, #1971, #16854, #33835, #11663, #24099, #14656, #23861, #489, #8182, #23741, #5633, #33094, #11877, #23059, #7790, #1561, #28167, #13438, #2317, #15700, #14265, #10614, #33470, #21911, #22302, #17644, #18518, #13423, #22863, #25679, #6470, #4395, #5168, #7610, #29450, #26872, #29566, #17474, #28960, #32016, #22344, #27871, #20196, #21145, #30311, #29891, #28410, #22616, #611, #6254, #22651, #9199, #21506, #32209, #6368, #33953, #5418, #9286, #29538, #18206, #19793, #9041, #4879, #19196, #1791, #28531, #33477, #15175 ) ) ;
#2405 = ORIENTED_EDGE ( 'NONE', *, *, #25499, .T. ) ;
#2407 = LINE ( 'NONE', #15607, #27062 ) ;
#2406 = DIRECTION ( 'NONE',  ( -1.000000000000000000, 0.000000000000000000, 0.000000000000000000 ) ) ;
#2408 = CYLINDRICAL_SURFACE ( 'NONE', #28466, 16.19999999999999574 ) ;
#2410 = ORIENTED_EDGE ( 'NONE', *, *, #19984, .F. ) ;
#2409 = AXIS2_PLACEMENT_3D ( 'NONE', #19586, #33271, #9068 ) ;
#2411 = AXIS2_PLACEMENT_3D ( 'NONE', #17555, #1332, #12204 ) ;
#2412 = EDGE_CURVE ( 'NONE', #6259, #3630, #12436, .T. ) ;
#2413 = AXIS2_PLACEMENT_3D ( 'NONE', #31258, #6515, #6859 ) ;
#2414 = PRESENTATION_STYLE_ASSIGNMENT (( #26800 ) ) ;
#2415 = PLANE ( 'NONE',  #26807 ) ;
#2416 = ORIENTED_EDGE ( 'NONE', *, *, #8034, .T. ) ;
#2417 = DIRECTION ( 'NONE',  ( -7.893605728314051750E-14, 1.618803117314786530E-15, 1.000000000000000000 ) ) ;
#2418 = ORIENTED_EDGE ( 'NONE', *, *, #3028, .F. ) ;
#2419 = CARTESIAN_POINT ( 'NONE',  ( -105.3457392332551734, 5.115129524682074269, 5.485020507536670031 ) ) ;
#2420 = ORIENTED_EDGE ( 'NONE', *, *, #15759, .T. ) ;
#2421 = DIRECTION ( 'NONE',  ( -1.000000000000000000, -0.000000000000000000, 0.000000000000000000 ) ) ;
#2422 = CARTESIAN_POINT ( 'NONE',  ( -105.8662310357297400, -5.044029065977393422, -5.550668370081900171 ) ) ;
#2423 = DIRECTION ( 'NONE',  ( 1.000000000000000000, 0.000000000000000000, 0.000000000000000000 ) ) ;
#2424 = ORIENTED_EDGE ( 'NONE', *, *, #14612, .T. ) ;
#2425 = VERTEX_POINT ( 'NONE', #7061 ) ;
#2426 = ORIENTED_EDGE ( 'NONE', *, *, #11147, .T. ) ;
#2427 = FACE_OUTER_BOUND ( 'NONE', #2848, .T. ) ;
#2428 = DIRECTION ( 'NONE',  ( -1.000000000000000000, -0.000000000000000000, 0.000000000000000000 ) ) ;
#2429 = CARTESIAN_POINT ( 'NONE',  ( -445.9999999999999432, 124.9999999999999432, -162.9999999999999716 ) ) ;
#2430 = EDGE_CURVE ( 'NONE', #34071, #27140, #17962, .T. ) ;
#2431 = AXIS2_PLACEMENT_3D ( 'NONE', #34915, #27066, #2684 ) ;
#2432 = EDGE_CURVE ( 'NONE', #21158, #16944, #20268, .T. ) ;
#2433 = FACE_OUTER_BOUND ( 'NONE', #21921, .T. ) ;
#2434 = FACE_OUTER_BOUND ( 'NONE', #31762, .T. ) ;
#2435 = VECTOR ( 'NONE', #15082, 1000.000000000000000 ) ;
#2436 = DIRECTION ( 'NONE',  ( -1.000000000000000000, 0.000000000000000000, 0.000000000000000000 ) ) ;
#2437 = VECTOR ( 'NONE', #14111, 1000.000000000000114 ) ;
#2438 = CARTESIAN_POINT ( 'NONE',  ( 11.99999999999999645, -124.9999999999999432, -186.9999999999999716 ) ) ;
#2439 = VERTEX_POINT ( 'NONE', #30935 ) ;
#2440 = CARTESIAN_POINT ( 'NONE',  ( 53.89849999999999852, 0.000000000000000000, 0.000000000000000000 ) ) ;
#2441 = CARTESIAN_POINT ( 'NONE',  ( 99.45027429990390999, 1.507575458593797046, 12.41447922803859072 ) ) ;
#2442 = CARTESIAN_POINT ( 'NONE',  ( -442.0000000000000000, -112.9999999999999858, 155.0000000000000000 ) ) ;
#2443 = VERTEX_POINT ( 'NONE', #22927 ) ;
#2444 = EDGE_CURVE ( 'NONE', #7133, #7970, #6542, .T. ) ;
#2445 = CARTESIAN_POINT ( 'NONE',  ( -15.99999999999998579, -137.0000000000000000, 155.0000000000000000 ) ) ;
#2446 = EDGE_LOOP ( 'NONE', ( #12551, #26713, #15573, #807 ) ) ;
#2447 = CARTESIAN_POINT ( 'NONE',  ( -109.8484943653665056, 1.663653002832651051, -12.39274845084345600 ) ) ;
#2448 = FACE_OUTER_BOUND ( 'NONE', #18477, .T. ) ;
#2449 = VECTOR ( 'NONE', #29989, 1000.000000000000000 ) ;
#2450 = ORIENTED_EDGE ( 'NONE', *, *, #5372, .T. ) ;
#2451 = CARTESIAN_POINT ( 'NONE',  ( -12.00000000000001066, 112.9999999999999574, -155.0000000000000000 ) ) ;
#2452 = DIRECTION ( 'NONE',  ( -1.000000000000000000, 6.792721752314501023E-48, -3.697785493223492838E-32 ) ) ;
#2453 = LINE ( 'NONE', #32185, #1825 ) ;
#2454 = VERTEX_POINT ( 'NONE', #28266 ) ;
#2455 = AXIS2_PLACEMENT_3D ( 'NONE', #4584, #31656, #18167 ) ;
#2456 = VERTEX_POINT ( 'NONE', #26285 ) ;
#2457 = CIRCLE ( 'NONE', #22338, 7.999999999999992895 ) ;
#2458 = CARTESIAN_POINT ( 'NONE',  ( 764.2996812273407841, 1268.661710855847332, 1753.598338701303419 ) ) ;
#2459 = VECTOR ( 'NONE', #23170, 1000.000000000000114 ) ;
#2460 = DIRECTION ( 'NONE',  ( 0.000000000000000000, 0.000000000000000000, 1.000000000000000000 ) ) ;
#2461 = EDGE_CURVE ( 'NONE', #32511, #18108, #21126, .T. ) ;
#2462 = ORIENTED_EDGE ( 'NONE', *, *, #14480, .F. ) ;
#2463 = CARTESIAN_POINT ( 'NONE',  ( 7.700000000000000178, 0.000000000000000000, 0.000000000000000000 ) ) ;
#2464 = CARTESIAN_POINT ( 'NONE',  ( 1.394999999999999574, -18.66807150955393624, -28.91175816027523027 ) ) ;
#2465 = CARTESIAN_POINT ( 'NONE',  ( 60.00000000000000000, 33.69708579775584667, 49.43553178847298568 ) ) ;
#2466 = CARTESIAN_POINT ( 'NONE',  ( 107.5858466720334974, -5.135784989587515170, 5.469495349232144754 ) ) ;
#2467 = CONTEXT_DEPENDENT_SHAPE_REPRESENTATION ( #23970, #18079 ) ;
#2468 = ORIENTED_EDGE ( 'NONE', *, *, #8263, .T. ) ;
#2469 = LINE ( 'NONE', #33603, #10130 ) ;
#2470 = EDGE_CURVE ( 'NONE', #6969, #19088, #21305, .T. ) ;
#2471 = EDGE_CURVE ( 'NONE', #26514, #17916, #10433, .T. ) ;
#2472 = EDGE_CURVE ( 'NONE', #12505, #8625, #18135, .T. ) ;
#2473 = AXIS2_PLACEMENT_3D ( 'NONE', #17316, #14461, #30817 ) ;
#2475 = CARTESIAN_POINT ( 'NONE',  ( -20.00000000000007461, 108.9999999999999858, 162.9999999999999716 ) ) ;
#2474 = CARTESIAN_POINT ( 'NONE',  ( 0.000000000000000000, 33.69708579775584667, -36.68877005347592757 ) ) ;
#2476 = VERTEX_POINT ( 'NONE', #4551 ) ;
#2477 = ORIENTED_EDGE ( 'NONE', *, *, #27413, .F. ) ;
#2478 = CARTESIAN_POINT ( 'NONE',  ( 17.27856612038524631, 33.69708579775584667, 68.31122994652405112 ) ) ;
#2479 = EDGE_LOOP ( 'NONE', ( #29551, #31827, #32049, #16985 ) ) ;
#2480 = CARTESIAN_POINT ( 'NONE',  ( -430.0000000000000000, -135.0000000000000000, 113.9999999999999858 ) ) ;
#2481 = DIRECTION ( 'NONE',  ( 0.000000000000000000, -3.374343856708137958E-53, 1.000000000000000000 ) ) ;
#2482 = ORIENTED_EDGE ( 'NONE', *, *, #6366, .T. ) ;
#2483 = AXIS2_PLACEMENT_3D ( 'NONE', #2245, #32314, #7932 ) ;
#2484 = CARTESIAN_POINT ( 'NONE',  ( 10.00000000000000000, 7.794228634059932048, -13.49999999999999822 ) ) ;
#2485 = AXIS2_PLACEMENT_3D ( 'NONE', #24632, #16659, #21985 ) ;
#2486 = VECTOR ( 'NONE', #4152, 1000.000000000000000 ) ;
#2487 = PRODUCT_DEFINITION_SHAPE ( 'NONE', 'NONE',  #35219 ) ;
#2488 = CARTESIAN_POINT ( 'NONE',  ( 0.5355294694855877724, -14.31130214556279867, -2.212097561415799607 ) ) ;
#2489 = VERTEX_POINT ( 'NONE', #15447 ) ;
#2490 = DIRECTION ( 'NONE',  ( 1.000000000000000000, 0.000000000000000000, 0.000000000000000000 ) ) ;
#2491 = CARTESIAN_POINT ( 'NONE',  ( -12.00000000000001066, 136.9999999999999716, 155.0000000000000000 ) ) ;
#2492 = CARTESIAN_POINT ( 'NONE',  ( 0.07094833732824711026, -0.5905164915254609292, -31.68852467239035420 ) ) ;
#2493 = FACE_OUTER_BOUND ( 'NONE', #4348, .T. ) ;
#2494 = CARTESIAN_POINT ( 'NONE',  ( 22.89764159710613001, 4.274639749586560455, -77.50000000000000000 ) ) ;
#2495 = DIRECTION ( 'NONE',  ( -0.000000000000000000, 1.000000000000000000, -0.000000000000000000 ) ) ;
#2496 = VECTOR ( 'NONE', #5781, 1000.000000000000000 ) ;
#2497 = ORIENTED_EDGE ( 'NONE', *, *, #17584, .T. ) ;
#2498 = CARTESIAN_POINT ( 'NONE',  ( 22.89764159710615132, -3.615060903476078114, -87.50000000000000000 ) ) ;
#2499 = DIRECTION ( 'NONE',  ( -1.047444401652940007E-14, 1.000000000000000000, 6.982962677686266711E-15 ) ) ;
#2500 = PRODUCT_DEFINITION_CONTEXT ( 'detailed design', #4164, 'design' ) ;
#2501 = ORIENTED_EDGE ( 'NONE', *, *, #18732, .T. ) ;
#2502 = CIRCLE ( 'NONE', #7660, 1.154999999999999805 ) ;
#2503 = ORIENTED_EDGE ( 'NONE', *, *, #2089, .F. ) ;
#2504 = EDGE_CURVE ( 'NONE', #19925, #4827, #10920, .T. ) ;
#2505 = CIRCLE ( 'NONE', #31479, 15.00000000000000000 ) ;
#2506 = DIRECTION ( 'NONE',  ( 1.000000000000000000, 0.000000000000000000, 0.000000000000000000 ) ) ;
#2507 = EDGE_CURVE ( 'NONE', #4850, #28271, #16924, .T. ) ;
#2508 = ORIENTED_EDGE ( 'NONE', *, *, #18257, .T. ) ;
#2509 = DIRECTION ( 'NONE',  ( -0.000000000000000000, -1.000000000000000000, -0.000000000000000000 ) ) ;
#2510 = CARTESIAN_POINT ( 'NONE',  ( -0.9727285265192158192, -1.747512292859697114, 5.429999999999999716 ) ) ;
#2511 = AXIS2_PLACEMENT_3D ( 'NONE', #13425, #16104, #24258 ) ;
#2512 = EDGE_CURVE ( 'NONE', #15960, #1246, #1554, .T. ) ;
#2513 = CONTEXT_DEPENDENT_SHAPE_REPRESENTATION ( #21954, #32031 ) ;
#2514 = EDGE_CURVE ( 'NONE', #18417, #33401, #8920, .T. ) ;
#2515 = CARTESIAN_POINT ( 'NONE',  ( 2.604019710756261929, -18.30372525367464220, -26.59104308589841992 ) ) ;
#2516 = ORIENTED_EDGE ( 'NONE', *, *, #361, .T. ) ;
#2517 = VERTEX_POINT ( 'NONE', #25009 ) ;
#2518 = CARTESIAN_POINT ( 'NONE',  ( -8.205391194442450056E-14, 7.412271713511258575, -29.75335163721776865 ) ) ;
#2519 = LINE ( 'NONE', #18218, #24681 ) ;
#2520 = EDGE_CURVE ( 'NONE', #31799, #12400, #12928, .T. ) ;
#2521 = DIRECTION ( 'NONE',  ( 0.000000000000000000, -0.000000000000000000, 1.000000000000000000 ) ) ;
#2522 = CARTESIAN_POINT ( 'NONE',  ( 0.02407890056655825201, 14.63235270440936731, 27.43224275967444470 ) ) ;
#2523 = FACE_OUTER_BOUND ( 'NONE', #18954, .T. ) ;
#2524 = VERTEX_POINT ( 'NONE', #13643 ) ;
#2525 = DIRECTION ( 'NONE',  ( 0.9075754196709571175, 0.4198891015602645438, 7.713237663339539704E-17 ) ) ;
#2526 = FACE_OUTER_BOUND ( 'NONE', #25809, .T. ) ;
#2527 = TOROIDAL_SURFACE ( 'NONE', #11642, 30.47050528711512030, 8.000000000000000000 ) ;
#2528 = CARTESIAN_POINT ( 'NONE',  ( -361.0000000000000000, 124.9999999999999432, 166.9999999999999716 ) ) ;
#2529 = B_SPLINE_CURVE_WITH_KNOTS ( 'NONE', 3,
 ( #34558, #15895, #2328, #1808, #24036, #23523, #34923, #20855, #10539, #26366, #21391, #23702, #21029, #31866, #32237, #25093, #13724, #198, #16768, #13905, #18903, #729, #2688, #24748, #551, #19429, #16418, #8381, #14263, #11063, #11595, #5689, #16949, #11237, #2854, #8021, #16589, #32932, #32577, #22445, #8200, #11406, #22265, #5348, #24561 ),
 .UNSPECIFIED., .F., .F.,
 ( 4, 2, 2, 2, 2, 2, 2, 2, 2, 2, 1, 2, 2, 2, 2, 2, 2, 2, 2, 2, 2, 2, 4 ),
 ( 3.984693255910324139E-19, 0.001177949164446570477, 0.002355898328893140520, 0.003533847493339711213, 0.004711796657786281907, 0.005889745822232853034, 0.007067694986679424161, 0.007656669568902727506, 0.008245644151126031718, 0.008834618733349335062, 0.009423593315572640142, 0.01001256789779594349, 0.01060154248001924683, 0.01119051706224255191, 0.01177949164446585525, 0.01295744080891246194, 0.01413538997335907210, 0.01531333913780567879, 0.01590231372002897173, 0.01649128830225226466, 0.01708026288447555760, 0.01766923746669885054, 0.01884718663114543988 ),
 .UNSPECIFIED. ) ;
#2530 = PLANE ( 'NONE',  #32804 ) ;
#2531 = CARTESIAN_POINT ( 'NONE',  ( 0.5248942728107164335, 7.015288891536787474, 32.63428354963185285 ) ) ;
#2532 = EDGE_CURVE ( 'NONE', #9716, #34419, #22007, .T. ) ;
#2533 = EDGE_CURVE ( 'NONE', #25357, #28271, #2777, .T. ) ;
#2534 = LINE ( 'NONE', #32545, #22690 ) ;
#2535 = DIRECTION ( 'NONE',  ( 1.000000000000000000, 0.000000000000000000, 0.000000000000000000 ) ) ;
#2537 = CYLINDRICAL_SURFACE ( 'NONE', #12853, 7.999999999999979572 ) ;
#2536 = CARTESIAN_POINT ( 'NONE',  ( 19.99999999999998224, 112.9999999999999574, 155.0000000000000000 ) ) ;
#2538 = VECTOR ( 'NONE', #8049, 999.9999999999998863 ) ;
#2539 = AXIS2_PLACEMENT_3D ( 'NONE', #2112, #20805, #23826 ) ;
#2540 = CARTESIAN_POINT ( 'NONE',  ( 2.765921099433441999, 26.03801215795542134, -16.98986790278583570 ) ) ;
#2541 = ORIENTED_EDGE ( 'NONE', *, *, #33568, .T. ) ;
#2542 = CARTESIAN_POINT ( 'NONE',  ( -12.00000000000001066, 104.9999999999999858, 154.9999999999999432 ) ) ;
#2544 = PLANE ( 'NONE',  #14038 ) ;
#2543 = CARTESIAN_POINT ( 'NONE',  ( -12.00000000000001066, -145.0000000000000000, -186.9999999999999716 ) ) ;
#2545 = EDGE_LOOP ( 'NONE', ( #1596, #26188, #15712, #31943 ) ) ;
#2546 = DIRECTION ( 'NONE',  ( -1.000000000000000000, -0.000000000000000000, -0.000000000000000000 ) ) ;
#2547 = EDGE_LOOP ( 'NONE', ( #27809, #20644, #34283, #22240 ) ) ;
#2548 = VECTOR ( 'NONE', #21211, 1000.000000000000000 ) ;
#2549 = ORIENTED_EDGE ( 'NONE', *, *, #24788, .T. ) ;
#2550 = DIRECTION ( 'NONE',  ( 0.6876994588534233177, -0.7259954919231308423, 0.000000000000000000 ) ) ;
#2551 = ORIENTED_EDGE ( 'NONE', *, *, #10036, .F. ) ;
#2552 = ORIENTED_EDGE ( 'NONE', *, *, #3159, .F. ) ;
#2553 = LINE ( 'NONE', #21254, #26975 ) ;
#2554 = DIRECTION ( 'NONE',  ( 0.3701381553399133995, -0.9289767198167917517, -0.000000000000000000 ) ) ;
#2555 = FACE_OUTER_BOUND ( 'NONE', #28740, .T. ) ;
#2556 = ORIENTED_EDGE ( 'NONE', *, *, #6456, .T. ) ;
#2557 = ORIENTED_EDGE ( 'NONE', *, *, #25305, .F. ) ;
#2558 = VECTOR ( 'NONE', #4203, 1000.000000000000000 ) ;
#2559 = DIRECTION ( 'NONE',  ( -3.040835319149746090E-31, -1.000000000000000000, 0.000000000000000000 ) ) ;
#2560 = CARTESIAN_POINT ( 'NONE',  ( 2.789999999999999147, -26.45933846664182099, -16.32596387352474565 ) ) ;
#2561 = CLOSED_SHELL ( 'NONE', ( #17393, #4919, #18542, #16810, #20931, #33380, #20339, #33676, #17841, #34520, #6844, #30058, #1144, #16743, #14168, #19359, #11021, #4523 ) ) ;
#2562 = EDGE_CURVE ( 'NONE', #24130, #18561, #30361, .T. ) ;
#2563 = FACE_OUTER_BOUND ( 'NONE', #29011, .T. ) ;
#2564 = DIRECTION ( 'NONE',  ( -1.000000000000000000, 6.792721752314501023E-48, -3.697785493223492838E-32 ) ) ;
#2565 = ORIENTED_EDGE ( 'NONE', *, *, #19560, .F. ) ;
#2566 = DIRECTION ( 'NONE',  ( 1.000000000000000000, 3.040835319149746090E-31, 1.232595164407830946E-32 ) ) ;
#2567 = EDGE_CURVE ( 'NONE', #8018, #25712, #5266, .T. ) ;
#2568 = EDGE_CURVE ( 'NONE', #14276, #22576, #24657, .T. ) ;
#2569 = FACE_OUTER_BOUND ( 'NONE', #17868, .T. ) ;
#2570 = EDGE_LOOP ( 'NONE', ( #10804, #5901, #20792, #29362 ) ) ;
#2571 = CARTESIAN_POINT ( 'NONE',  ( -499.9999999999999432, 112.9999999999999574, 159.0000000000000000 ) ) ;
#2572 = CARTESIAN_POINT ( 'NONE',  ( 2.790000000000000036, -30.07665394020993688, 5.960573492977232490 ) ) ;
#2573 = CARTESIAN_POINT ( 'NONE',  ( 0.000000000000000000, 0.000000000000000000, 87.50000000000000000 ) ) ;
#2574 = VERTEX_POINT ( 'NONE', #27514 ) ;
#2575 = DIRECTION ( 'NONE',  ( 1.000000000000000000, 0.000000000000000000, 0.000000000000000000 ) ) ;
#2576 = ORIENTED_EDGE ( 'NONE', *, *, #9965, .F. ) ;
#2577 = AXIS2_PLACEMENT_3D ( 'NONE', #7021, #31756, #14894 ) ;
#2578 = VECTOR ( 'NONE', #26046, 1000.000000000000000 ) ;
#2579 = LINE ( 'NONE', #13452, #12724 ) ;
#2580 = ORIENTED_EDGE ( 'NONE', *, *, #29927, .F. ) ;
#2582 = LINE ( 'NONE', #30161, #11766 ) ;
#2581 = DIRECTION ( 'NONE',  ( 0.000000000000000000, 2.309213040847544338E-50, 1.000000000000000000 ) ) ;
#2583 = AXIS2_PLACEMENT_3D ( 'NONE', #20877, #1827, #13055 ) ;
#2584 = CARTESIAN_POINT ( 'NONE',  ( -45.00000000000000000, 3.353962854566122864, 15.81122994652406355 ) ) ;
#2585 = EDGE_CURVE ( 'NONE', #27140, #731, #11334, .T. ) ;
#2586 = ORIENTED_EDGE ( 'NONE', *, *, #23860, .T. ) ;
#2587 = SURFACE_SIDE_STYLE ('',( #24459 ) ) ;
#2588 = DIRECTION ( 'NONE',  ( -0.000000000000000000, -0.000000000000000000, -1.000000000000000000 ) ) ;
#2589 = CIRCLE ( 'NONE', #322, 3.999999999999982681 ) ;
#2590 = ORIENTED_EDGE ( 'NONE', *, *, #24493, .T. ) ;
#2591 = ADVANCED_FACE ( 'NONE', ( #29840 ), #3129, .F. ) ;
#2592 = EDGE_CURVE ( 'NONE', #18981, #33679, #10388, .T. ) ;
#2593 = VERTEX_POINT ( 'NONE', #13822 ) ;
#2594 = DIRECTION ( 'NONE',  ( 0.000000000000000000, 1.836970198721029688E-16, -1.000000000000000000 ) ) ;
#2595 = CARTESIAN_POINT ( 'NONE',  ( -104.6485238499209203, 5.105882603317797752, 5.493682664683364081 ) ) ;
#2596 = ORIENTED_EDGE ( 'NONE', *, *, #4717, .F. ) ;
#2597 = LINE ( 'NONE', #35012, #1375 ) ;
#2598 = SURFACE_STYLE_USAGE ( .BOTH. , #13642 ) ;
#2599 = VECTOR ( 'NONE', #29093, 1000.000000000000000 ) ;
#2600 = CARTESIAN_POINT ( 'NONE',  ( -107.3019298601570881, -4.579683091146231178, -5.941712070794213929 ) ) ;
#2601 = DIRECTION ( 'NONE',  ( -0.000000000000000000, -0.000000000000000000, 1.000000000000000000 ) ) ;
#2602 = ORIENTED_EDGE ( 'NONE', *, *, #7802, .F. ) ;
#2603 = EDGE_LOOP ( 'NONE', ( #8262, #17852, #24670, #10697 ) ) ;
#2604 = VERTEX_POINT ( 'NONE', #8645 ) ;
#2605 = CARTESIAN_POINT ( 'NONE',  ( 0.000000000000000000, -33.69708579775584667, -49.43553178847298568 ) ) ;
#2606 = DIRECTION ( 'NONE',  ( 0.000000000000000000, 0.000000000000000000, 1.000000000000000000 ) ) ;
#2607 = AXIS2_PLACEMENT_3D ( 'NONE', #9022, #27704, #25022 ) ;
#2608 = CARTESIAN_POINT ( 'NONE',  ( 2.604019705252365480, 7.229557500018881200, 31.46177729073544072 ) ) ;
#2609 = CARTESIAN_POINT ( 'NONE',  ( -349.0000000000000000, -125.0000000000000284, 126.0000000000000000 ) ) ;
#2610 = CARTESIAN_POINT ( 'NONE',  ( 2.789999999999999147, -20.35927063852789232, -24.61013060777193218 ) ) ;
#2611 = EDGE_CURVE ( 'NONE', #14020, #18600, #14001, .T. ) ;
#2612 = EDGE_CURVE ( 'NONE', #2702, #19872, #5964, .T. ) ;
#2614 = CARTESIAN_POINT ( 'NONE',  ( 0.000000000000000000, 2.296212748401288367E-15, 87.50000000000000000 ) ) ;
#2613 =( REPRESENTATION_RELATIONSHIP ('NONE','NONE', #23037, #15767 ) REPRESENTATION_RELATIONSHIP_WITH_TRANSFORMATION ( #32537 )SHAPE_REPRESENTATION_RELATIONSHIP( ) );
#2615 = FACE_BOUND ( 'NONE', #28818, .T. ) ;
#2616 = ORIENTED_EDGE ( 'NONE', *, *, #26320, .T. ) ;
#2617 = AXIS2_PLACEMENT_3D ( 'NONE', #29913, #32389, #29730 ) ;
#2618 = PLANE ( 'NONE',  #35048 ) ;
#2619 = CARTESIAN_POINT ( 'NONE',  ( -2.216215597024040029, -32.46987467335853239, 68.31122994652405112 ) ) ;
#2620 = EDGE_CURVE ( 'NONE', #32635, #26400, #25402, .T. ) ;
#2621 = DIRECTION ( 'NONE',  ( -0.000000000000000000, -1.000000000000000000, -0.000000000000000000 ) ) ;
#2622 = ORIENTED_EDGE ( 'NONE', *, *, #22348, .T. ) ;
#2623 = VECTOR ( 'NONE', #28744, 1000.000000000000000 ) ;
#2624 = CIRCLE ( 'NONE', #22530, 7.999999999999979572 ) ;
#2625 = DIRECTION ( 'NONE',  ( 0.000000000000000000, 0.000000000000000000, -1.000000000000000000 ) ) ;
#2626 = ORIENTED_EDGE ( 'NONE', *, *, #4967, .F. ) ;
#2627 = FACE_OUTER_BOUND ( 'NONE', #6214, .T. ) ;
#2628 = DIRECTION ( 'NONE',  ( 0.000000000000000000, 1.000000000000000000, -3.374343856708137958E-53 ) ) ;
#2629 = CIRCLE ( 'NONE', #33914, 3.999999999999982681 ) ;
#2630 = ORIENTED_EDGE ( 'NONE', *, *, #18757, .T. ) ;
#2631 = CARTESIAN_POINT ( 'NONE',  ( 1.395000000000002238, -33.26546734453825849, 8.820166447041648539 ) ) ;
#2632 = DIRECTION ( 'NONE',  ( 1.000000000000000000, -0.000000000000000000, -0.000000000000000000 ) ) ;
#2633 = CARTESIAN_POINT ( 'NONE',  ( -445.9999999999999432, 113.0000000000000000, -155.0000000000000000 ) ) ;
#2634 = AXIS2_PLACEMENT_3D ( 'NONE', #24105, #26962, #27301 ) ;
#2635 = VERTEX_POINT ( 'NONE', #115 ) ;
#2636 = EDGE_CURVE ( 'NONE', #25782, #11484, #3306, .T. ) ;
#2637 = EDGE_CURVE ( 'NONE', #25524, #21875, #5442, .T. ) ;
#2638 = ORIENTED_EDGE ( 'NONE', *, *, #5711, .T. ) ;
#2639 = DIRECTION ( 'NONE',  ( -7.893605728314050488E-14, 1.618803117314786135E-15, 0.9999999999999998890 ) ) ;
#2640 = CARTESIAN_POINT ( 'NONE',  ( 0.7561992242453015045, -33.91102616014372728, 0.5305038583916231731 ) ) ;
#2641 = ORIENTED_EDGE ( 'NONE', *, *, #10650, .T. ) ;
#2642 = AXIS2_PLACEMENT_3D ( 'NONE', #4328, #34068, #26576 ) ;
#2643 = CARTESIAN_POINT ( 'NONE',  ( -35.00000000000000000, 42.49491490430484220, -36.69637551990492597 ) ) ;
#2644 = EDGE_CURVE ( 'NONE', #21537, #19872, #21820, .T. ) ;
#2645 = DIRECTION ( 'NONE',  ( -0.000000000000000000, -0.000000000000000000, -1.000000000000000000 ) ) ;
#2646 = EDGE_CURVE ( 'NONE', #3173, #10330, #10658, .T. ) ;
#2647 = FACE_OUTER_BOUND ( 'NONE', #2650, .T. ) ;
#2648 = CARTESIAN_POINT ( 'NONE',  ( -100.0251193558530076, -1.201525761660788838, 7.405089084531746302 ) ) ;
#2649 = ORIENTED_EDGE ( 'NONE', *, *, #29824, .T. ) ;
#2651 = EDGE_CURVE ( 'NONE', #33917, #12803, #19177, .T. ) ;
#2650 = EDGE_LOOP ( 'NONE', ( #21092, #2897, #17562, #29919 ) ) ;
#2652 = DIRECTION ( 'NONE',  ( 0.000000000000000000, 0.000000000000000000, 1.000000000000000000 ) ) ;
#2653 = AXIS2_PLACEMENT_3D ( 'NONE', #2484, #24015, #34897 ) ;
#2654 = AXIS2_PLACEMENT_3D ( 'NONE', #18704, #29372, #15864 ) ;
#2656 = DIRECTION ( 'NONE',  ( 0.000000000000000000, 1.000000000000000000, 0.000000000000000000 ) ) ;
#2655 = LINE ( 'NONE', #11023, #8782 ) ;
#2657 = ORIENTED_EDGE ( 'NONE', *, *, #5324, .T. ) ;
#2658 = ORIENTED_EDGE ( 'NONE', *, *, #679, .T. ) ;
#2659 = DIRECTION ( 'NONE',  ( 0.000000000000000000, -2.309213040847544338E-50, -1.000000000000000000 ) ) ;
#2660 = VERTEX_POINT ( 'NONE', #25724 ) ;
#2661 = CARTESIAN_POINT ( 'NONE',  ( -45.00000000000000000, 16.36947364650383818, -36.69637551990492597 ) ) ;
#2662 = CARTESIAN_POINT ( 'NONE',  ( 0.006871079570366611135, -21.36428053051087161, -22.28216981039808786 ) ) ;
#2663 = ORIENTED_EDGE ( 'NONE', *, *, #17299, .T. ) ;
#2664 = ORIENTED_EDGE ( 'NONE', *, *, #23750, .F. ) ;
#2665 = FACE_OUTER_BOUND ( 'NONE', #32945, .T. ) ;
#2666 = CARTESIAN_POINT ( 'NONE',  ( -499.9999999999999432, -113.0000000000000000, -162.9999999999999716 ) ) ;
#2667 = VERTEX_POINT ( 'NONE', #25368 ) ;
#2668 = EDGE_CURVE ( 'NONE', #25012, #24957, #28293, .T. ) ;
#2669 = CARTESIAN_POINT ( 'NONE',  ( 2.789999999999999147, 28.52477022197300727, 10.62590764890735606 ) ) ;
#2670 = LINE ( 'NONE', #21375, #25694 ) ;
#2671 = CARTESIAN_POINT ( 'NONE',  ( 145.0000000000000568, -87.50000000000000000, 65.00000000000000000 ) ) ;
#2672 = DIRECTION ( 'NONE',  ( 0.5611870653623813876, -0.8276889981568911203, -0.000000000000000000 ) ) ;
#2673 = CARTESIAN_POINT ( 'NONE',  ( -10.00000000000000000, 0.000000000000000000, 0.000000000000000000 ) ) ;
#2674 = DIRECTION ( 'NONE',  ( -1.000000000000000000, -0.000000000000000000, -0.000000000000000000 ) ) ;
#2675 = CARTESIAN_POINT ( 'NONE',  ( -31.68358972719163091, 7.440061483287530919, 68.31122994652405112 ) ) ;
#2676 = AXIS2_PLACEMENT_3D ( 'NONE', #27749, #22602, #25066 ) ;
#2677 = EDGE_CURVE ( 'NONE', #10047, #2660, #10588, .T. ) ;
#2678 = EDGE_CURVE ( 'NONE', #3718, #31108, #1489, .T. ) ;
#2679 = CIRCLE ( 'NONE', #12381, 2.524999999999999467 ) ;
#2680 = AXIS2_PLACEMENT_3D ( 'NONE', #26348, #23504, #18018 ) ;
#2681 = EDGE_CURVE ( 'NONE', #22142, #2574, #16284, .T. ) ;
#2682 = ORIENTED_EDGE ( 'NONE', *, *, #30425, .F. ) ;
#2683 = CARTESIAN_POINT ( 'NONE',  ( 0.5594631266314759044, 30.83012635351326480, 13.00174666746673324 ) ) ;
#2684 = DIRECTION ( 'NONE',  ( 0.1063910735369155841, -0.9943243633099125844, -3.335902418025060287E-15 ) ) ;
#2685 = ORIENTED_EDGE ( 'NONE', *, *, #7210, .T. ) ;
#2686 = ORIENTED_EDGE ( 'NONE', *, *, #670, .T. ) ;
#2687 = AXIS2_PLACEMENT_3D ( 'NONE', #122, #4917, #15984 ) ;
#2688 = CARTESIAN_POINT ( 'NONE',  ( 104.2155338827948867, 5.687621871124707518, 4.888959764314519063 ) ) ;
#2689 = ITEM_DEFINED_TRANSFORMATION ( 'NONE', 'NONE', #4674,  #28566 ) ;
#2690 = VERTEX_POINT ( 'NONE', #20227 ) ;
#2691 = CARTESIAN_POINT ( 'NONE',  ( -414.0000000000000568, 113.0000000000000000, 154.9999999999999716 ) ) ;
#2692 = SURFACE_SIDE_STYLE ('',( #27077 ) ) ;
#2693 = CARTESIAN_POINT ( 'NONE',  ( -21.67835495107042476, 31.04982069277122747, 68.31122994652405112 ) ) ;
#2694 = AXIS2_PLACEMENT_3D ( 'NONE', #10403, #12739, #13734 ) ;
#2695 = ORIENTED_EDGE ( 'NONE', *, *, #4672, .T. ) ;
#2696 = ORIENTED_EDGE ( 'NONE', *, *, #29374, .F. ) ;
#2697 = CARTESIAN_POINT ( 'NONE',  ( 0.02407890056655564992, -0.3931553186911057041, -31.08824725498900676 ) ) ;
#2698 = DIRECTION ( 'NONE',  ( -1.000000000000000000, -0.000000000000000000, -0.000000000000000000 ) ) ;
#2699 = PLANE ( 'NONE',  #7928 ) ;
#2700 = CARTESIAN_POINT ( 'NONE',  ( 8.000000000000000000, 0.000000000000000000, 0.000000000000000000 ) ) ;
#2701 = DIRECTION ( 'NONE',  ( 0.000000000000000000, 0.08715574274765885976, 0.9961946980917454342 ) ) ;
#2702 = VERTEX_POINT ( 'NONE', #28577 ) ;
#2704 = DIRECTION ( 'NONE',  ( 0.000000000000000000, 0.000000000000000000, 1.000000000000000000 ) ) ;
#2703 = AXIS2_PLACEMENT_3D ( 'NONE', #21409, #27444, #24239 ) ;
#2706 = DIRECTION ( 'NONE',  ( 0.000000000000000000, 0.000000000000000000, 1.000000000000000000 ) ) ;
#2705 = VECTOR ( 'NONE', #29725, 1000.000000000000000 ) ;
#2707 = DIRECTION ( 'NONE',  ( 0.000000000000000000, 1.000000000000000000, 1.224646799147353207E-16 ) ) ;
#2708 = DIRECTION ( 'NONE',  ( 1.000000000000000000, 0.000000000000000000, 0.000000000000000000 ) ) ;
#2709 = PLANE ( 'NONE',  #189 ) ;
#2710 =( GEOMETRIC_REPRESENTATION_CONTEXT ( 3 ) GLOBAL_UNCERTAINTY_ASSIGNED_CONTEXT ( ( #30659 ) ) GLOBAL_UNIT_ASSIGNED_CONTEXT ( ( #18957, #29975, #29798 ) ) REPRESENTATION_CONTEXT ( 'NONE', 'WORKASPACE' ) );
#2712 = CARTESIAN_POINT ( 'NONE',  ( -102.4161755605319968, 4.417479313406522223, -6.061799023038633827 ) ) ;
#2711 = CARTESIAN_POINT ( 'NONE',  ( 2.765921099433441555, 18.59128259035472297, 24.91982945642928016 ) ) ;
#2713 = CARTESIAN_POINT ( 'NONE',  ( -1.341640786499875171, 0.000000000000000000, 0.000000000000000000 ) ) ;
#2714 = EDGE_LOOP ( 'NONE', ( #10883, #4586, #4670, #12603, #27163 ) ) ;
#2715 = DIRECTION ( 'NONE',  ( 1.000000000000000000, 0.000000000000000000, -1.232595164407831220E-32 ) ) ;
#2717 = CARTESIAN_POINT ( 'NONE',  ( 145.0000000000000568, -177.8172209610550851, -45.87893859614474223 ) ) ;
#2716 = PLANE ( 'NONE',  #25146 ) ;
#2718 = EDGE_CURVE ( 'NONE', #20895, #32553, #27626, .T. ) ;
#2719 = EDGE_CURVE ( 'NONE', #18446, #21633, #34462, .T. ) ;
#2720 = AXIS2_PLACEMENT_3D ( 'NONE', #22313, #19133, #24610 ) ;
#2721 = ORIENTED_EDGE ( 'NONE', *, *, #6742, .T. ) ;
#2722 = CARTESIAN_POINT ( 'NONE',  ( 0.02407890056655738464, -11.07880054387241664, 29.04985141099759360 ) ) ;
#2723 = EDGE_CURVE ( 'NONE', #27344, #10477, #2038, .T. ) ;
#2724 = ORIENTED_EDGE ( 'NONE', *, *, #15400, .T. ) ;
#2725 = CIRCLE ( 'NONE', #6149, 2.033421858999711951 ) ;
#2726 = VERTEX_POINT ( 'NONE', #22539 ) ;
#2727 = DIRECTION ( 'NONE',  ( -0.7259954919231308423, -0.6876994588534233177, -1.263283411590317421E-16 ) ) ;
#2728 = ORIENTED_EDGE ( 'NONE', *, *, #28653, .T. ) ;
#2729 = VERTEX_POINT ( 'NONE', #4345 ) ;
#2730 = DIRECTION ( 'NONE',  ( -1.000000000000000000, 0.000000000000000000, 0.000000000000000000 ) ) ;
#2731 = ADVANCED_FACE ( 'NONE', ( #23240 ), #9176, .T. ) ;
#2732 = CIRCLE ( 'NONE', #5014, 34.41491905851385269 ) ;
#2733 = CARTESIAN_POINT ( 'NONE',  ( -349.0000000000000000, 134.9999999999999716, 130.0000000000000000 ) ) ;
#2734 = FACE_OUTER_BOUND ( 'NONE', #7990, .T. ) ;
#2735 = ORIENTED_EDGE ( 'NONE', *, *, #2430, .T. ) ;
#2736 = ORIENTED_EDGE ( 'NONE', *, *, #20942, .T. ) ;
#2737 = CARTESIAN_POINT ( 'NONE',  ( 0.5248940516409021928, -29.61686074518734202, -15.39650178189456398 ) ) ;
#2738 = LINE ( 'NONE', #10594, #16975 ) ;
#2739 = CARTESIAN_POINT ( 'NONE',  ( 1.040000000000000480, -10.89151784028265979, -32.64600270996228204 ) ) ;
#2740 = AXIS2_PLACEMENT_3D ( 'NONE', #847, #5142, #5842 ) ;
#2741 = CARTESIAN_POINT ( 'NONE',  ( -19.99999999999998934, -145.0000000000000000, -186.9999999999999716 ) ) ;
#2742 = ORIENTED_EDGE ( 'NONE', *, *, #4936, .F. ) ;
#2743 = CARTESIAN_POINT ( 'NONE',  ( -20.00000000000001776, -145.0000000000000000, 162.9999999999999716 ) ) ;
#2744 = AXIS2_PLACEMENT_3D ( 'NONE', #9095, #27781, #6227 ) ;
#2745 = CYLINDRICAL_SURFACE ( 'NONE', #15332, 16.00000000000000000 ) ;
#2746 = ORIENTED_EDGE ( 'NONE', *, *, #32285, .T. ) ;
#2747 = CARTESIAN_POINT ( 'NONE',  ( -8.499999999999998224, 0.000000000000000000, 5.429999999999999716 ) ) ;
#2748 = DIRECTION ( 'NONE',  ( -1.000000000000000000, -0.000000000000000000, -0.000000000000000000 ) ) ;
#2749 = CYLINDRICAL_SURFACE ( 'NONE', #3235, 32.54542015209057126 ) ;
#2750 = FACE_OUTER_BOUND ( 'NONE', #30146, .T. ) ;
#2751 = VERTEX_POINT ( 'NONE', #3824 ) ;
#2752 =( GEOMETRIC_REPRESENTATION_CONTEXT ( 3 ) GLOBAL_UNCERTAINTY_ASSIGNED_CONTEXT ( ( #29100 ) ) GLOBAL_UNIT_ASSIGNED_CONTEXT ( ( #16721, #22754, #3692 ) ) REPRESENTATION_CONTEXT ( 'NONE', 'WORKASPACE' ) );
#2753 = CARTESIAN_POINT ( 'NONE',  ( 2.789999999999999147, -13.59935610937992401, 28.90010281771827039 ) ) ;
#2754 = VERTEX_POINT ( 'NONE', #33915 ) ;
#2755 = CARTESIAN_POINT ( 'NONE',  ( 9.199999999999999289, 0.000000000000000000, 0.000000000000000000 ) ) ;
#2756 = LINE ( 'NONE', #25481, #6290 ) ;
#2757 = EDGE_CURVE ( 'NONE', #30850, #6804, #4173, .T. ) ;
#2758 = CIRCLE ( 'NONE', #22674, 7.999999999999979572 ) ;
#2759 = VERTEX_POINT ( 'NONE', #3650 ) ;
#2760 = CARTESIAN_POINT ( 'NONE',  ( -5.491809612354312087, 32.07872192057773475, 68.31122994652405112 ) ) ;
#2761 = CARTESIAN_POINT ( 'NONE',  ( 1.394999999999999574, -10.89151784028311809, 32.64600270996213283 ) ) ;
#2762 = EDGE_CURVE ( 'NONE', #28976, #3173, #19877, .T. ) ;
#2763 = EDGE_CURVE ( 'NONE', #7154, #25708, #9449, .T. ) ;
#2764 = VERTEX_POINT ( 'NONE', #1523 ) ;
#2765 = CIRCLE ( 'NONE', #27773, 7.999999999999979572 ) ;
#2766 = ADVANCED_FACE ( 'NONE', ( #12390 ), #33735, .T. ) ;
#2767 = EDGE_CURVE ( 'NONE', #4014, #24757, #22889, .T. ) ;
#2768 = ORIENTED_EDGE ( 'NONE', *, *, #19291, .T. ) ;
#2769 = CARTESIAN_POINT ( 'NONE',  ( 3.235562306570555532E-30, 4.168562732279004202, -67.50000000000000000 ) ) ;
#2770 = CARTESIAN_POINT ( 'NONE',  ( 129.3530333899765594, 6.000000000000000000, 62.49999999999999289 ) ) ;
#2771 = ORIENTED_EDGE ( 'NONE', *, *, #440, .F. ) ;
#2772 = ORIENTED_EDGE ( 'NONE', *, *, #18265, .F. ) ;
#2773 = CARTESIAN_POINT ( 'NONE',  ( 19.99999999999990763, -134.9999999999999716, -186.9999999999999716 ) ) ;
#2774 = ADVANCED_FACE ( 'NONE', ( #20561 ), #821, .F. ) ;
#2775 = CARTESIAN_POINT ( 'NONE',  ( 23.31255882915078814, -22.70966696615089830, 49.43553178847298568 ) ) ;
#2776 = VECTOR ( 'NONE', #27329, 1000.000000000000000 ) ;
#2777 = LINE ( 'NONE', #30015, #7204 ) ;
#2778 = DIRECTION ( 'NONE',  ( -1.000000000000000000, 0.000000000000000000, 0.000000000000000000 ) ) ;
#2779 = ORIENTED_EDGE ( 'NONE', *, *, #29449, .F. ) ;
#2780 = VERTEX_POINT ( 'NONE', #6313 ) ;
#2781 = CARTESIAN_POINT ( 'NONE',  ( 15.99999999999998579, 124.9999999999999716, 162.9999999999999716 ) ) ;
#2782 = PLANE ( 'NONE',  #18115 ) ;
#2783 = CYLINDRICAL_SURFACE ( 'NONE', #14085, 16.19999999999999574 ) ;
#2784 = CARTESIAN_POINT ( 'NONE',  ( 42.44043929807611448, -20.15143121711728469, 20.00000000000000000 ) ) ;
#2785 = AXIS2_PLACEMENT_3D ( 'NONE', #972, #32986, #28194 ) ;
#2786 = DIRECTION ( 'NONE',  ( 0.000000000000000000, 0.000000000000000000, 1.000000000000000000 ) ) ;
#2787 = CARTESIAN_POINT ( 'NONE',  ( -12.00000000000001066, -24.99999999999999289, -154.9999999999999716 ) ) ;
#2788 = DIRECTION ( 'NONE',  ( 0.000000000000000000, 0.000000000000000000, -1.000000000000000000 ) ) ;
#2789 = ORIENTED_EDGE ( 'NONE', *, *, #23686, .F. ) ;
#2790 = DIRECTION ( 'NONE',  ( 0.000000000000000000, 0.000000000000000000, 1.000000000000000000 ) ) ;
#2791 = CARTESIAN_POINT ( 'NONE',  ( -10.84269519964070305, -36.27449394610879096, 68.31122994652405112 ) ) ;
#2792 = CARTESIAN_POINT ( 'NONE',  ( 2.765921099433443775, -31.05158812718220673, -1.559667679918931738 ) ) ;
#2793 = ORIENTED_EDGE ( 'NONE', *, *, #23749, .T. ) ;
#2794 = VECTOR ( 'NONE', #13223, 1000.000000000000114 ) ;
#2795 = CARTESIAN_POINT ( 'NONE',  ( 12.00000000000001066, -24.99999999999999289, -175.0000000000000000 ) ) ;
#2796 = EDGE_LOOP ( 'NONE', ( #16490, #1957, #8917, #16128, #9760, #32886 ) ) ;
#2797 = CARTESIAN_POINT ( 'NONE',  ( -107.5694449394638070, 4.435438170924840939, -11.68828588916098532 ) ) ;
#2798 = DIRECTION ( 'NONE',  ( 0.000000000000000000, 0.000000000000000000, 1.000000000000000000 ) ) ;
#2799 =( GEOMETRIC_REPRESENTATION_CONTEXT ( 3 ) GLOBAL_UNCERTAINTY_ASSIGNED_CONTEXT ( ( #4875 ) ) GLOBAL_UNIT_ASSIGNED_CONTEXT ( ( #13910, #16067, #30272 ) ) REPRESENTATION_CONTEXT ( 'NONE', 'WORKASPACE' ) );
#2800 = ORIENTED_EDGE ( 'NONE', *, *, #6915, .F. ) ;
#2801 = CARTESIAN_POINT ( 'NONE',  ( -5.781867695661277118, -1.866624223957557671, 0.000000000000000000 ) ) ;
#2802 = LINE ( 'NONE', #19204, #25278 ) ;
#2803 = DIRECTION ( 'NONE',  ( 0.000000000000000000, 1.000000000000000000, -1.224646799147353207E-16 ) ) ;
#2804 = ORIENTED_EDGE ( 'NONE', *, *, #33019, .T. ) ;
#2805 = CIRCLE ( 'NONE', #27250, 2.033421858999711951 ) ;
#2806 = ORIENTED_EDGE ( 'NONE', *, *, #27808, .T. ) ;
#2807 = ADVANCED_FACE ( 'NONE', ( #17219 ), #9362, .T. ) ;
#2808 = ADVANCED_FACE ( 'NONE', ( #2040 ), #26416, .T. ) ;
#2809 = DIRECTION ( 'NONE',  ( 0.1063910735369155841, -0.9943243633099125844, -3.335902418025060287E-15 ) ) ;
#2810 = LINE ( 'NONE', #32193, #22381 ) ;
#2811 = VERTEX_POINT ( 'NONE', #7719 ) ;
#2812 = CARTESIAN_POINT ( 'NONE',  ( 30.98406361983693103, 9.959526819984924728, 49.43553178847298568 ) ) ;
#2813 = DIRECTION ( 'NONE',  ( -0.000000000000000000, -0.000000000000000000, 1.000000000000000000 ) ) ;
#2814 = AXIS2_PLACEMENT_3D ( 'NONE', #29009, #29375, #7461 ) ;
#2815 = CARTESIAN_POINT ( 'NONE',  ( 0.000000000000000000, 0.000000000000000000, 0.000000000000000000 ) ) ;
#2816 = CARTESIAN_POINT ( 'NONE',  ( -104.3033539127188902, -5.070312235224276876, 5.526528498279830615 ) ) ;
#2817 = CONTEXT_DEPENDENT_SHAPE_REPRESENTATION ( #19684, #11746 ) ;
#2818 = ORIENTED_EDGE ( 'NONE', *, *, #9035, .F. ) ;
#2820 = ORIENTED_EDGE ( 'NONE', *, *, #25287, .T. ) ;
#2819 =( REPRESENTATION_RELATIONSHIP ('NONE','NONE', #23037, #15767 ) REPRESENTATION_RELATIONSHIP_WITH_TRANSFORMATION ( #11549 )SHAPE_REPRESENTATION_RELATIONSHIP( ) );
#2821 = ORIENTED_EDGE ( 'NONE', *, *, #5114, .F. ) ;
#2822 = DIRECTION ( 'NONE',  ( 1.000000000000000000, 3.469446951953834515E-18, 0.000000000000000000 ) ) ;
#2823 = EDGE_CURVE ( 'NONE', #25524, #24033, #15234, .T. ) ;
#2824 = CARTESIAN_POINT ( 'NONE',  ( 0.006871057928818130774, -30.82708482934414462, -1.618146408792933810 ) ) ;
#2825 = CYLINDRICAL_SURFACE ( 'NONE', #28658, 2.525000000000001243 ) ;
#2826 = ORIENTED_EDGE ( 'NONE', *, *, #29090, .T. ) ;
#2827 = ORIENTED_EDGE ( 'NONE', *, *, #11782, .F. ) ;
#2828 = DIRECTION ( 'NONE',  ( 0.000000000000000000, 0.000000000000000000, -1.000000000000000000 ) ) ;
#2829 = ORIENTED_EDGE ( 'NONE', *, *, #1250, .T. ) ;
#2830 = EDGE_CURVE ( 'NONE', #11221, #1041, #7904, .T. ) ;
#2831 = LINE ( 'NONE', #22065, #29483 ) ;
#2832 = CARTESIAN_POINT ( 'NONE',  ( -19.99999999999998934, 4.559999999999908127, 172.9900000000000091 ) ) ;
#2833 = ORIENTED_EDGE ( 'NONE', *, *, #18375, .F. ) ;
#2834 = EDGE_CURVE ( 'NONE', #1944, #995, #15679, .T. ) ;
#2836 = EDGE_CURVE ( 'NONE', #23824, #10179, #4314, .T. ) ;
#2835 = VERTEX_POINT ( 'NONE', #31752 ) ;
#2837 = CARTESIAN_POINT ( 'NONE',  ( 1.341640786499872284, 0.000000000000000000, 0.000000000000000000 ) ) ;
#2838 = CARTESIAN_POINT ( 'NONE',  ( 1.532562817202168137, 32.50931595846690669, 68.31122994652405112 ) ) ;
#2839 = ORIENTED_EDGE ( 'NONE', *, *, #27763, .T. ) ;
#2840 = DIRECTION ( 'NONE',  ( 0.000000000000000000, 0.000000000000000000, 1.000000000000000000 ) ) ;
#2841 = FACE_OUTER_BOUND ( 'NONE', #22149, .T. ) ;
#2842 = EDGE_CURVE ( 'NONE', #7715, #26754, #12556, .T. ) ;
#2843 = CARTESIAN_POINT ( 'NONE',  ( 1.749999999999999778, -30.02688531850407472, 16.81585001935568613 ) ) ;
#2844 = DIRECTION ( 'NONE',  ( 1.000000000000000000, 0.000000000000000000, 0.000000000000000000 ) ) ;
#2845 = CARTESIAN_POINT ( 'NONE',  ( -70.00000000000000000, 4.559999999999909015, -168.2400000000000091 ) ) ;
#2846 = DIRECTION ( 'NONE',  ( 1.000000000000000000, 0.000000000000000000, 0.000000000000000000 ) ) ;
#2847 = LINE ( 'NONE', #25263, #23474 ) ;
#2848 = EDGE_LOOP ( 'NONE', ( #8992, #33439, #11552, #27371 ) ) ;
#2849 = EDGE_CURVE ( 'NONE', #9840, #13159, #18778, .T. ) ;
#2850 = DIRECTION ( 'NONE',  ( 0.000000000000000000, 1.000000000000000000, 0.000000000000000000 ) ) ;
#2851 = DIRECTION ( 'NONE',  ( 0.000000000000000000, 0.000000000000000000, 1.000000000000000000 ) ) ;
#2852 = VERTEX_POINT ( 'NONE', #23399 ) ;
#2853 = ORIENTED_EDGE ( 'NONE', *, *, #687, .T. ) ;
#2854 = CARTESIAN_POINT ( 'NONE',  ( 100.1670491183068208, 3.098707215121725422, 6.832002823648420708 ) ) ;
#2855 = CONTEXT_DEPENDENT_SHAPE_REPRESENTATION ( #18284, #6365 ) ;
#2856 = VERTEX_POINT ( 'NONE', #10224 ) ;
#2857 = LINE ( 'NONE', #22093, #1421 ) ;
#2858 = LINE ( 'NONE', #11241, #10205 ) ;
#2860 = DIRECTION ( 'NONE',  ( 0.000000000000000000, 0.000000000000000000, 1.000000000000000000 ) ) ;
#2859 = CARTESIAN_POINT ( 'NONE',  ( -499.9999999999999432, 136.9999999999999432, 190.9999999999999716 ) ) ;
#2862 = ORIENTED_EDGE ( 'NONE', *, *, #25345, .F. ) ;
#2861 = TOROIDAL_SURFACE ( 'NONE', #6348, 30.47050528711512030, 8.000000000000000000 ) ;
#2863 = VERTEX_POINT ( 'NONE', #9874 ) ;
#2864 = CARTESIAN_POINT ( 'NONE',  ( -5.491809612354312975, 32.07872192057773475, 68.31122994652405112 ) ) ;
#2865 = CARTESIAN_POINT ( 'NONE',  ( 19.99999999999996092, -145.0000000000000000, 187.0000000000000000 ) ) ;
#2866 = DIRECTION ( 'NONE',  ( -0.000000000000000000, 1.836970198721029934E-16, -1.000000000000000000 ) ) ;
#2867 = CARTESIAN_POINT ( 'NONE',  ( 10.96230482721425403, -12.47301499840864025, -77.50000000000000000 ) ) ;
#2868 = DIRECTION ( 'NONE',  ( 0.000000000000000000, -1.131431318426415506E-52, -1.000000000000000000 ) ) ;
#2869 = EDGE_LOOP ( 'NONE', ( #2685, #2630, #33156, #15051 ) ) ;
#2870 = EDGE_CURVE ( 'NONE', #32496, #17537, #2624, .T. ) ;
#2871 = CYLINDRICAL_SURFACE ( 'NONE', #14673, 7.999999999999979572 ) ;
#2872 = CARTESIAN_POINT ( 'NONE',  ( 30.98406361983693103, 9.959526819984924728, 49.43553178847298568 ) ) ;
#2873 = EDGE_CURVE ( 'NONE', #18186, #23654, #34258, .T. ) ;
#2874 = LINE ( 'NONE', #13406, #7241 ) ;
#2875 = VECTOR ( 'NONE', #24618, 1000.000000000000000 ) ;
#2876 = CARTESIAN_POINT ( 'NONE',  ( -365.0000000000000000, 118.9999999999999716, 126.0000000000000000 ) ) ;
#2877 = CARTESIAN_POINT ( 'NONE',  ( -418.0000000000000000, 104.9999999999999858, -190.9999999999999716 ) ) ;
#2878 = AXIS2_PLACEMENT_3D ( 'NONE', #7905, #11115, #27288 ) ;
#2879 = CARTESIAN_POINT ( 'NONE',  ( 2.789999999999999147, 23.53611639059738536, -19.35207786518964213 ) ) ;
#2881 = DIRECTION ( 'NONE',  ( 0.000000000000000000, 1.000000000000000000, 0.000000000000000000 ) ) ;
#2880 = DIRECTION ( 'NONE',  ( 0.000000000000000000, 1.836970198721029934E-16, -1.000000000000000000 ) ) ;
#2882 = CARTESIAN_POINT ( 'NONE',  ( 12.00000000000001066, -60.99999999999997158, -175.0000000000000000 ) ) ;
#2883 = ORIENTED_EDGE ( 'NONE', *, *, #11401, .T. ) ;
#2884 = CYLINDRICAL_SURFACE ( 'NONE', #9910, 2.000000000000001776 ) ;
#2886 = CARTESIAN_POINT ( 'NONE',  ( 2.033800775754698975, -33.91102616014372018, -0.5305038583921004580 ) ) ;
#2885 = LINE ( 'NONE', #29957, #32538 ) ;
#2887 = ORIENTED_EDGE ( 'NONE', *, *, #4477, .T. ) ;
#2888 = VECTOR ( 'NONE', #6809, 1000.000000000000227 ) ;
#2889 = DIRECTION ( 'NONE',  ( 0.000000000000000000, -0.000000000000000000, 1.000000000000000000 ) ) ;
#2890 = VECTOR ( 'NONE', #1110, 1000.000000000000000 ) ;
#2891 = CIRCLE ( 'NONE', #13155, 13.50000000000000178 ) ;
#2892 = ORIENTED_EDGE ( 'NONE', *, *, #25388, .T. ) ;
#2893 = EDGE_LOOP ( 'NONE', ( #13763, #14228, #35021, #11969, #19644, #12214 ) ) ;
#2894 = CARTESIAN_POINT ( 'NONE',  ( -15.99999999999998579, -112.9999999999999858, 155.0000000000000000 ) ) ;
#2895 = EDGE_LOOP ( 'NONE', ( #29008, #11211, #28715, #34782, #8518, #32872, #13532, #19129, #17560, #923, #20347, #17292, #33269 ) ) ;
#2896 = B_SPLINE_CURVE_WITH_KNOTS ( 'NONE', 3,
 ( #10136, #15318, #2288, #31663, #34341, #7271, #21353, #16020, #4425, #4775, #15851, #34694, #15490, #23662, #29536, #1942, #26854, #20993, #18694, #2123, #7447, #1769, #15671, #21168, #7629, #18527, #29361, #2466, #9783, #20647, #4956, #31490, #12646, #23481, #9960, #20819, #30408, #27035, #514, #22049, #32365, #32893 ),
 .UNSPECIFIED., .F., .F.,
 ( 4, 2, 2, 2, 2, 2, 2, 2, 2, 2, 2, 2, 2, 2, 2, 2, 2, 2, 2, 2, 4 ),
 ( 0.01884718663114543988, 0.01943499450852638824, 0.02002280238590734007, 0.02119841814066924027, 0.02237403389543114046, 0.02354964965019304066, 0.02472526540495494085, 0.02590088115971684452, 0.02707649691447874471, 0.02766430479185969654, 0.02825211266924064490, 0.02883992054662159674, 0.02942772842400254510, 0.03060334417876444529, 0.03177895993352634896, 0.03295457568828825262, 0.03413019144305015629, 0.03471799932043109771, 0.03530580719781203913, 0.03648142295257392198, 0.03765703870733580483 ),
 .UNSPECIFIED. ) ;
#2897 = ORIENTED_EDGE ( 'NONE', *, *, #29209, .F. ) ;
#2898 = AXIS2_PLACEMENT_3D ( 'NONE', #17177, #17360, #3961 ) ;
#2899 = DIRECTION ( 'NONE',  ( -0.000000000000000000, -0.000000000000000000, 1.000000000000000000 ) ) ;
#2900 = AXIS2_PLACEMENT_3D ( 'NONE', #28578, #15236, #29087 ) ;
#2901 = CARTESIAN_POINT ( 'NONE',  ( 8.927936315454010341, -31.29690601358701940, 68.31122994652405112 ) ) ;
#2902 = DIRECTION ( 'NONE',  ( 0.000000000000000000, 1.000000000000000000, -6.123233995736766036E-17 ) ) ;
#2903 = ORIENTED_EDGE ( 'NONE', *, *, #5568, .T. ) ;
#2904 = EDGE_LOOP ( 'NONE', ( #15588, #30122, #18559, #17838, #24354, #19701, #13019, #12225 ) ) ;
#2905 = DIRECTION ( 'NONE',  ( -0.9868265225415261410, 0.1617819965527647341, -0.000000000000000000 ) ) ;
#2906 = FACE_OUTER_BOUND ( 'NONE', #15377, .T. ) ;
#2907 = ADVANCED_FACE ( 'NONE', ( #26592 ), #20740, .T. ) ;
#2908 = PLANE ( 'NONE',  #26679 ) ;
#2909 = CARTESIAN_POINT ( 'NONE',  ( 2.789999999999999147, 7.489092610871091793, 29.53582882395389930 ) ) ;
#2910 = ORIENTED_EDGE ( 'NONE', *, *, #16125, .F. ) ;
#2911 = EDGE_CURVE ( 'NONE', #1214, #23491, #10589, .T. ) ;
#2912 = CARTESIAN_POINT ( 'NONE',  ( 7.699999999999998401, 0.000000000000000000, 0.000000000000000000 ) ) ;
#2913 = ADVANCED_FACE ( 'NONE', ( #15941 ), #8952, .T. ) ;
#2914 = AXIS2_PLACEMENT_3D ( 'NONE', #6195, #27746, #21882 ) ;
#2915 = CARTESIAN_POINT ( 'NONE',  ( 1.039999999999999369, -1.891117961020236216, 34.36292081097831641 ) ) ;
#2916 = ORIENTED_EDGE ( 'NONE', *, *, #2762, .T. ) ;
#2917 = AXIS2_PLACEMENT_3D ( 'NONE', #19073, #32391, #13546 ) ;
#2918 = VECTOR ( 'NONE', #10255, 1000.000000000000114 ) ;
#2919 = EDGE_CURVE ( 'NONE', #2856, #3550, #16287, .T. ) ;
#2920 = CARTESIAN_POINT ( 'NONE',  ( 31.73435513276359643, 7.220462394039754095, 49.43553178847298568 ) ) ;
#2921 = CARTESIAN_POINT ( 'NONE',  ( 1.256659300721212479E-17, 4.060282914029830437, -30.39157201494045779 ) ) ;
#2922 = CARTESIAN_POINT ( 'NONE',  ( -35.00000000000000000, 42.49491490430484220, 36.69637551990492597 ) ) ;
#2923 = CARTESIAN_POINT ( 'NONE',  ( -12.00000000000001066, 108.9999999999999858, -155.0000000000000000 ) ) ;
#2924 = VERTEX_POINT ( 'NONE', #1857 ) ;
#2925 = CYLINDRICAL_SURFACE ( 'NONE', #29753, 4.750000000000004441 ) ;
#2926 = ORIENTED_EDGE ( 'NONE', *, *, #34135, .F. ) ;
#2928 = CARTESIAN_POINT ( 'NONE',  ( 2.606461819198067520, -27.67670874042536511, -16.59602520068896325 ) ) ;
#2927 = CARTESIAN_POINT ( 'NONE',  ( 0.000000000000000000, -32.54542015209051442, -87.50000000000000000 ) ) ;
#2929 = CARTESIAN_POINT ( 'NONE',  ( 0.000000000000000000, 0.000000000000000000, 0.000000000000000000 ) ) ;
#2930 = AXIS2_PLACEMENT_3D ( 'NONE', #4126, #18048, #4472 ) ;
#2931 = ORIENTED_EDGE ( 'NONE', *, *, #19549, .F. ) ;
#2932 = DIRECTION ( 'NONE',  ( 0.000000000000000000, 6.123233995736766036E-17, 1.000000000000000000 ) ) ;
#2933 = PRODUCT ( 'MAT-054', 'MAT-054', '', ( #34560 ) ) ;
#2934 = DIRECTION ( 'NONE',  ( -0.000000000000000000, 1.000000000000000000, -0.000000000000000000 ) ) ;
#2935 = ORIENTED_EDGE ( 'NONE', *, *, #22794, .F. ) ;
#2936 = CIRCLE ( 'NONE', #21693, 2.525000000000003020 ) ;
#2937 = CIRCLE ( 'NONE', #18870, 4.750000000000004441 ) ;
#2938 = CIRCLE ( 'NONE', #11474, 4.306175033202026547 ) ;
#2940 = ORIENTED_EDGE ( 'NONE', *, *, #28958, .T. ) ;
#2939 = AXIS2_PLACEMENT_3D ( 'NONE', #15458, #15637, #17973 ) ;
#2941 = LINE ( 'NONE', #33197, #22039 ) ;
#2942 = CARTESIAN_POINT ( 'NONE',  ( -110.1150203881707910, -1.604996202923496961E-20, 7.500000000000000000 ) ) ;
#2943 = ORIENTED_EDGE ( 'NONE', *, *, #23576, .F. ) ;
#2944 = ORIENTED_EDGE ( 'NONE', *, *, #3910, .F. ) ;
#2945 = DIRECTION ( 'NONE',  ( 0.000000000000000000, 1.000000000000000000, 1.224646799147353207E-16 ) ) ;
#2946 = DIRECTION ( 'NONE',  ( 1.000000000000000000, 0.000000000000000000, 0.000000000000000000 ) ) ;
#2947 = CARTESIAN_POINT ( 'NONE',  ( 0.006892384605615998854, -17.88431215799113971, -25.16139613958922894 ) ) ;
#2948 = DIRECTION ( 'NONE',  ( 0.000000000000000000, -1.000000000000000000, 0.000000000000000000 ) ) ;
#2949 = ORIENTED_EDGE ( 'NONE', *, *, #10436, .T. ) ;
#2950 = VERTEX_POINT ( 'NONE', #12734 ) ;
#2951 = EDGE_CURVE ( 'NONE', #28825, #11793, #26768, .T. ) ;
#2952 = CARTESIAN_POINT ( 'NONE',  ( -12.00000000000001066, 134.9999999999999432, -194.9999999999999432 ) ) ;
#2953 = DIRECTION ( 'NONE',  ( -0.000000000000000000, -0.000000000000000000, -1.000000000000000000 ) ) ;
#2954 = CARTESIAN_POINT ( 'NONE',  ( 6.857172176539690689, 37.23415287044793587, 68.31122994652405112 ) ) ;
#2955 = EDGE_CURVE ( 'NONE', #1469, #26315, #11742, .T. ) ;
#2956 = LINE ( 'NONE', #13830, #688 ) ;
#2957 = CARTESIAN_POINT ( 'NONE',  ( -499.9999999999999432, -145.0000000000000000, -162.9999999999999716 ) ) ;
#2958 = DIRECTION ( 'NONE',  ( 0.000000000000000000, 1.836970198721029441E-16, -1.000000000000000000 ) ) ;
#2959 = CARTESIAN_POINT ( 'NONE',  ( -2.791255079241054649, -37.75727539589166071, 68.31122994652405112 ) ) ;
#2960 = ORIENTED_EDGE ( 'NONE', *, *, #5762, .T. ) ;
#2961 = EDGE_CURVE ( 'NONE', #22052, #26665, #20817, .T. ) ;
#2962 = CARTESIAN_POINT ( 'NONE',  ( -9.978866888775527855, 4.168562732279005090, -67.50000000000000000 ) ) ;
#2963 = CARTESIAN_POINT ( 'NONE',  ( 0.7561992021476438008, -17.72251720152558008, 28.91628452940440752 ) ) ;
#2964 = VECTOR ( 'NONE', #7710, 1000.000000000000000 ) ;
#2965 = CARTESIAN_POINT ( 'NONE',  ( -418.0000000000000000, 105.0000000000000142, 190.9999999999999716 ) ) ;
#2966 = ORIENTED_EDGE ( 'NONE', *, *, #32440, .F. ) ;
#2967 = AXIS2_PLACEMENT_3D ( 'NONE', #13018, #15203, #23850 ) ;
#2968 = EDGE_CURVE ( 'NONE', #8710, #18246, #11277, .T. ) ;
#2969 = COLOUR_RGB ( '',0.7921568627450980005, 0.8196078431372548767, 0.9333333333333333481 ) ;
#2970 = LINE ( 'NONE', #22737, #10981 ) ;
#2971 = VERTEX_POINT ( 'NONE', #11456 ) ;
#2972 = DIRECTION ( 'NONE',  ( 0.000000000000000000, 0.000000000000000000, -1.000000000000000000 ) ) ;
#2973 = CARTESIAN_POINT ( 'NONE',  ( 2.765921099433442443, 30.61125888652961891, 5.439165181699118889 ) ) ;
#2974 = ADVANCED_FACE ( 'NONE', ( #21610 ), #5736, .T. ) ;
#2975 = ADVANCED_FACE ( 'NONE', ( #8776 ), #30138, .F. ) ;
#2976 = ORIENTED_EDGE ( 'NONE', *, *, #34307, .T. ) ;
#2977 = FACE_OUTER_BOUND ( 'NONE', #33721, .T. ) ;
#2978 = CARTESIAN_POINT ( 'NONE',  ( 23.93847777447631131, 22.04889236939138186, 68.31122994652405112 ) ) ;
#2979 = DIRECTION ( 'NONE',  ( 0.000000000000000000, 1.000000000000000000, 1.224646799147353207E-16 ) ) ;
#2980 = ORIENTED_EDGE ( 'NONE', *, *, #16202, .F. ) ;
#2981 = ORIENTED_EDGE ( 'NONE', *, *, #26787, .T. ) ;
#2982 = DIRECTION ( 'NONE',  ( 2.631201909438060585E-14, -5.396010391056496978E-16, 1.000000000000000000 ) ) ;
#2983 = DIRECTION ( 'NONE',  ( 0.000000000000000000, 1.000000000000000000, -3.374343856708137958E-53 ) ) ;
#2984 = ORIENTED_EDGE ( 'NONE', *, *, #6255, .F. ) ;
#2985 = CARTESIAN_POINT ( 'NONE',  ( 0.07094832897469352528, -24.04001846604995762, 20.65402650742307955 ) ) ;
#2986 = AXIS2_PLACEMENT_3D ( 'NONE', #33105, #546, #13899 ) ;
#2987 = DIRECTION ( 'NONE',  ( 1.000000000000000000, 0.000000000000000000, 0.000000000000000000 ) ) ;
#2988 = AXIS2_PLACEMENT_3D ( 'NONE', #20111, #28631, #4236 ) ;
#2989 = DIRECTION ( 'NONE',  ( 0.000000000000000000, -5.145227585319922065E-49, -1.000000000000000000 ) ) ;
#2990 = FACE_OUTER_BOUND ( 'NONE', #284, .T. ) ;
#2991 = CONTEXT_DEPENDENT_SHAPE_REPRESENTATION ( #29441, #33612 ) ;
#2992 = ORIENTED_EDGE ( 'NONE', *, *, #10272, .F. ) ;
#2993 = ORIENTED_EDGE ( 'NONE', *, *, #30891, .F. ) ;
#2994 = ORIENTED_EDGE ( 'NONE', *, *, #20017, .F. ) ;
#2995 = CARTESIAN_POINT ( 'NONE',  ( -18.38714294329533416, -33.09555747561021377, 68.31122994652405112 ) ) ;
#2996 = DIRECTION ( 'NONE',  ( -1.000000000000000000, -0.000000000000000000, -0.000000000000000000 ) ) ;
#2997 = DIRECTION ( 'NONE',  ( 0.000000000000000000, -0.8443279255020161855, 0.5358267949789948803 ) ) ;
#2998 = ORIENTED_EDGE ( 'NONE', *, *, #22626, .F. ) ;
#2999 = VERTEX_POINT ( 'NONE', #8075 ) ;
#3000 = LINE ( 'NONE', #33080, #33940 ) ;
#3001 = VERTEX_POINT ( 'NONE', #32627 ) ;
#3002 = DIRECTION ( 'NONE',  ( 0.000000000000000000, -0.5288966977476834419, -0.8486862100397269959 ) ) ;
#3003 = ADVANCED_FACE ( 'NONE', ( #8599 ), #16463, .F. ) ;
#3004 = DIRECTION ( 'NONE',  ( 0.000000000000000000, 1.000000000000000000, 5.145227585319922065E-49 ) ) ;
#3005 = ORIENTED_EDGE ( 'NONE', *, *, #26043, .F. ) ;
#3006 = ORIENTED_EDGE ( 'NONE', *, *, #30583, .F. ) ;
#3007 = FACE_OUTER_BOUND ( 'NONE', #7328, .T. ) ;
#3008 = VECTOR ( 'NONE', #8091, 1000.000000000000000 ) ;
#3009 = EDGE_CURVE ( 'NONE', #27667, #1340, #19302, .T. ) ;
#3010 = EDGE_CURVE ( 'NONE', #5255, #939, #27647, .T. ) ;
#3011 = CARTESIAN_POINT ( 'NONE',  ( 14.70109753509668948, 34.88954974633765005, 68.31122994652405112 ) ) ;
#3012 = VERTEX_POINT ( 'NONE', #595 ) ;
#3013 = DIRECTION ( 'NONE',  ( 0.000000000000000000, 0.000000000000000000, -1.000000000000000000 ) ) ;
#3014 = LINE ( 'NONE', #5151, #27952 ) ;
#3015 = CARTESIAN_POINT ( 'NONE',  ( 0.02407890056655651728, 7.350529080603541487, 30.20932655202940254 ) ) ;
#3017 = PRESENTATION_STYLE_ASSIGNMENT (( #33453 ) ) ;
#3016 = AXIS2_PLACEMENT_3D ( 'NONE', #10489, #10299, #29528 ) ;
#3018 = AXIS2_PLACEMENT_3D ( 'NONE', #5628, #8319, #9907 ) ;
#3019 = CIRCLE ( 'NONE', #26322, 3.999999999999976019 ) ;
#3020 = CARTESIAN_POINT ( 'NONE',  ( 9.199999999999999289, -7.794228634059937377, 13.50000000000000000 ) ) ;
#3021 = DIRECTION ( 'NONE',  ( 1.000000000000000000, -0.000000000000000000, -0.000000000000000000 ) ) ;
#3022 = DIRECTION ( 'NONE',  ( 0.000000000000000000, 0.000000000000000000, -1.000000000000000000 ) ) ;
#3023 = EDGE_CURVE ( 'NONE', #1296, #15995, #27724, .T. ) ;
#3024 = EDGE_LOOP ( 'NONE', ( #7604, #23300, #11770, #18423 ) ) ;
#3025 = CYLINDRICAL_SURFACE ( 'NONE', #26247, 16.19999999999999574 ) ;
#3026 = DIRECTION ( 'NONE',  ( 2.631201909438060269E-14, -5.396010391056495992E-16, 0.9999999999999998890 ) ) ;
#3027 = EDGE_LOOP ( 'NONE', ( #24950, #28921 ) ) ;
#3029 = VERTEX_POINT ( 'NONE', #5215 ) ;
#3028 = EDGE_CURVE ( 'NONE', #24189, #20636, #1586, .T. ) ;
#3030 = EDGE_CURVE ( 'NONE', #18432, #23654, #16637, .T. ) ;
#3031 = CIRCLE ( 'NONE', #17300, 2.524999999999999467 ) ;
#3032 = EDGE_CURVE ( 'NONE', #11066, #32798, #27159, .T. ) ;
#3033 = DIRECTION ( 'NONE',  ( -1.000000000000000000, 0.000000000000000000, -0.000000000000000000 ) ) ;
#3034 = ITEM_DEFINED_TRANSFORMATION ( 'NONE', 'NONE', #151,  #28566 ) ;
#3035 = VERTEX_POINT ( 'NONE', #30315 ) ;
#3036 = CARTESIAN_POINT ( 'NONE',  ( -9.978866888775426602, 18.16264470403145381, -87.50000000000000000 ) ) ;
#3037 = FACE_OUTER_BOUND ( 'NONE', #19799, .T. ) ;
#3038 = ADVANCED_FACE ( 'NONE', ( #21963 ), #16109, .T. ) ;
#3039 = AXIS2_PLACEMENT_3D ( 'NONE', #29747, #12684, #33848 ) ;
#3041 = LINE ( 'NONE', #24925, #28895 ) ;
#3040 = CARTESIAN_POINT ( 'NONE',  ( 2.789999999999999147, -30.41598411195409923, 1.821977758773558165 ) ) ;
#3042 = VECTOR ( 'NONE', #25346, 1000.000000000000000 ) ;
#3043 = ORIENTED_EDGE ( 'NONE', *, *, #1161, .T. ) ;
#3044 = ORIENTED_EDGE ( 'NONE', *, *, #16790, .F. ) ;
#3045 = CIRCLE ( 'NONE', #4736, 2.000000000000001776 ) ;
#3046 = CARTESIAN_POINT ( 'NONE',  ( 3.235562306570555532E-30, -11.61907005722761177, -87.50000000000000000 ) ) ;
#3047 = PLANE ( 'NONE',  #8427 ) ;
#3048 = CARTESIAN_POINT ( 'NONE',  ( 0.000000000000000000, 2.281310696040539424E-14, -36.68877005347592757 ) ) ;
#3049 = PLANE ( 'NONE',  #34766 ) ;
#3050 = DIRECTION ( 'NONE',  ( 3.697785493223492838E-32, 1.934419779023891545E-16, -1.000000000000000000 ) ) ;
#3051 = ORIENTED_EDGE ( 'NONE', *, *, #31324, .T. ) ;
#3052 = LINE ( 'NONE', #16966, #8400 ) ;
#3053 = CARTESIAN_POINT ( 'NONE',  ( -1.307386931792819285, 37.83772838912469894, 68.31122994652405112 ) ) ;
#3054 = PLANE ( 'NONE',  #7835 ) ;
#3055 = ADVANCED_FACE ( 'NONE', ( #27118 ), #24654, .F. ) ;
#3056 = EDGE_CURVE ( 'NONE', #15311, #11473, #13431, .T. ) ;
#3057 = FACE_OUTER_BOUND ( 'NONE', #15149, .T. ) ;
#3058 = FILL_AREA_STYLE ('',( #27450 ) ) ;
#3059 = LINE ( 'NONE', #2354, #15537 ) ;
#3061 = CARTESIAN_POINT ( 'NONE',  ( -100.5621347894176836, 2.632420417224713649, -7.052679658646594518 ) ) ;
#3060 = CARTESIAN_POINT ( 'NONE',  ( -365.0000000000000000, -125.0000000000000284, 113.9999999999999858 ) ) ;
#3062 = VECTOR ( 'NONE', #25003, 1000.000000000000114 ) ;
#3063 = DIRECTION ( 'NONE',  ( 0.000000000000000000, -3.374343856708137958E-53, 1.000000000000000000 ) ) ;
#3064 = ORIENTED_EDGE ( 'NONE', *, *, #17544, .T. ) ;
#3065 = LINE ( 'NONE', #29956, #7640 ) ;
#3066 = DIRECTION ( 'NONE',  ( 0.000000000000000000, 0.000000000000000000, 1.000000000000000000 ) ) ;
#3067 = CARTESIAN_POINT ( 'NONE',  ( 2.789999999999999147, 27.98916443103621177, -15.38717335695007904 ) ) ;
#3069 = ORIENTED_EDGE ( 'NONE', *, *, #16942, .T. ) ;
#3068 = CIRCLE ( 'NONE', #18995, 7.999999999999979572 ) ;
#3070 = VECTOR ( 'NONE', #20545, 999.9999999999998863 ) ;
#3071 = CIRCLE ( 'NONE', #3660, 10.00000000000000000 ) ;
#3072 = ORIENTED_EDGE ( 'NONE', *, *, #9962, .F. ) ;
#3073 = EDGE_CURVE ( 'NONE', #16921, #18651, #10761, .T. ) ;
#3074 = ADVANCED_FACE ( 'NONE', ( #5920 ), #7827, .T. ) ;
#3075 =( REPRESENTATION_RELATIONSHIP ('NONE','NONE', #23037, #28231 ) REPRESENTATION_RELATIONSHIP_WITH_TRANSFORMATION ( #14841 )SHAPE_REPRESENTATION_RELATIONSHIP( ) );
#3076 = ORIENTED_EDGE ( 'NONE', *, *, #5235, .F. ) ;
#3077 = DIRECTION ( 'NONE',  ( 0.000000000000000000, 0.000000000000000000, 1.000000000000000000 ) ) ;
#3078 = VERTEX_POINT ( 'NONE', #2901 ) ;
#3079 = ORIENTED_EDGE ( 'NONE', *, *, #16775, .T. ) ;
#3080 = CARTESIAN_POINT ( 'NONE',  ( 2.789999999999999147, 30.61125888652969707, -5.439165181698684570 ) ) ;
#3081 = EDGE_CURVE ( 'NONE', #20828, #6161, #16397, .T. ) ;
#3082 = AXIS2_PLACEMENT_3D ( 'NONE', #22310, #2899, #30499 ) ;
#3083 = CARTESIAN_POINT ( 'NONE',  ( 8.000000000000000000, 0.000000000000000000, 0.000000000000000000 ) ) ;
#3084 = DIRECTION ( 'NONE',  ( 1.000000000000000000, 0.000000000000000000, 0.000000000000000000 ) ) ;
#3085 = ORIENTED_EDGE ( 'NONE', *, *, #6533, .T. ) ;
#3086 = EDGE_LOOP ( 'NONE', ( #32462, #24424, #33087, #4205 ) ) ;
#3087 = LINE ( 'NONE', #22682, #24196 ) ;
#3088 = EDGE_CURVE ( 'NONE', #21431, #20048, #33512, .T. ) ;
#3089 = DIRECTION ( 'NONE',  ( 0.000000000000000000, 1.000000000000000000, 1.836970198721029688E-16 ) ) ;
#3090 = VECTOR ( 'NONE', #31667, 1000.000000000000000 ) ;
#3091 = CARTESIAN_POINT ( 'NONE',  ( 109.1840482152002210, -3.931125184197653333, -11.86656790805995243 ) ) ;
#3092 = CARTESIAN_POINT ( 'NONE',  ( -262.5000000000000000, 0.000000000000000000, 10.00000000000000000 ) ) ;
#3093 = VERTEX_POINT ( 'NONE', #6448 ) ;
#3094 = EDGE_CURVE ( 'NONE', #22708, #14860, #23994, .T. ) ;
#3095 = CARTESIAN_POINT ( 'NONE',  ( -499.9999999999999432, 140.9999999999999716, -187.0000000000000000 ) ) ;
#3096 = CONICAL_SURFACE ( 'NONE', #23006, 13.50000000000000000, 1.047197551196600296 ) ;
#3097 = VECTOR ( 'NONE', #30299, 1000.000000000000000 ) ;
#3098 = DIRECTION ( 'NONE',  ( 1.000000000000000000, 0.000000000000000000, 0.000000000000000000 ) ) ;
#3099 = ORIENTED_EDGE ( 'NONE', *, *, #33722, .T. ) ;
#3100 = DIRECTION ( 'NONE',  ( -0.000000000000000000, -0.000000000000000000, -1.000000000000000000 ) ) ;
#3101 = CARTESIAN_POINT ( 'NONE',  ( 2.789999999999999147, -21.56796757982795043, -22.39322359481629476 ) ) ;
#3102 = DIRECTION ( 'NONE',  ( 0.000000000000000000, -1.000000000000000000, 0.000000000000000000 ) ) ;
#3103 = CARTESIAN_POINT ( 'NONE',  ( 0.07094834073506586791, -30.32005755872678776, -9.230678093032972598 ) ) ;
#3104 = VERTEX_POINT ( 'NONE', #25675 ) ;
#3105 = CYLINDRICAL_SURFACE ( 'NONE', #30906, 8.000000000000007105 ) ;
#3106 = VERTEX_POINT ( 'NONE', #1302 ) ;
#3107 = EDGE_CURVE ( 'NONE', #22599, #24075, #33688, .T. ) ;
#3109 = CARTESIAN_POINT ( 'NONE',  ( 1.749999999999999778, 31.89769921722987434, 12.91988538846969803 ) ) ;
#3108 = DIRECTION ( 'NONE',  ( 1.000000000000000000, 3.469446951953834515E-18, 0.000000000000000000 ) ) ;
#3110 = AXIS2_PLACEMENT_3D ( 'NONE', #24223, #10182, #23528 ) ;
#3111 = VERTEX_POINT ( 'NONE', #3952 ) ;
#3112 = DIRECTION ( 'NONE',  ( 0.000000000000000000, 0.000000000000000000, 1.000000000000000000 ) ) ;
#3113 = FACE_OUTER_BOUND ( 'NONE', #16213, .T. ) ;
#3114 = VECTOR ( 'NONE', #34487, 1000.000000000000000 ) ;
#3115 = ADVANCED_FACE ( 'NONE', ( #1131 ), #31031, .T. ) ;
#3116 = ORIENTED_EDGE ( 'NONE', *, *, #9237, .F. ) ;
#3117 = ORIENTED_EDGE ( 'NONE', *, *, #20580, .T. ) ;
#3118 = ADVANCED_FACE ( 'NONE', ( #22678 ), #28181, .T. ) ;
#3119 = EDGE_CURVE ( 'NONE', #890, #14045, #22494, .T. ) ;
#3120 = AXIS2_PLACEMENT_3D ( 'NONE', #7840, #2495, #18722 ) ;
#3121 = ORIENTED_EDGE ( 'NONE', *, *, #25985, .F. ) ;
#3122 = DIRECTION ( 'NONE',  ( 0.000000000000000000, 1.836970198721029688E-16, -1.000000000000000000 ) ) ;
#3123 = DIRECTION ( 'NONE',  ( 0.000000000000000000, -0.000000000000000000, -1.000000000000000000 ) ) ;
#3124 = ORIENTED_EDGE ( 'NONE', *, *, #4524, .F. ) ;
#3125 = EDGE_LOOP ( 'NONE', ( #3616, #32924, #1986, #12687 ) ) ;
#3126 = CARTESIAN_POINT ( 'NONE',  ( 26.04754872656010889, -19.51229300245305964, 68.31122994652405112 ) ) ;
#3127 = AXIS2_PLACEMENT_3D ( 'NONE', #25343, #17192, #28023 ) ;
#3128 = CARTESIAN_POINT ( 'NONE',  ( -442.0000000000000000, 105.0000000000000142, -109.9999999999999574 ) ) ;
#3129 = PLANE ( 'NONE',  #15213 ) ;
#3130 = CARTESIAN_POINT ( 'NONE',  ( -20.02113311122488781, 4.168562732279004202, -67.50000000000000000 ) ) ;
#3131 = ORIENTED_EDGE ( 'NONE', *, *, #28641, .F. ) ;
#3132 = ORIENTED_EDGE ( 'NONE', *, *, #16191, .F. ) ;
#3133 = CARTESIAN_POINT ( 'NONE',  ( 0.000000000000000000, 30.40449935640661039, 2.004522720844265304 ) ) ;
#3134 = FACE_OUTER_BOUND ( 'NONE', #25988, .T. ) ;
#3135 = CARTESIAN_POINT ( 'NONE',  ( -410.0000000000000568, -125.0000000000000000, -101.9999999999999858 ) ) ;
#3136 = DIRECTION ( 'NONE',  ( 0.000000000000000000, 0.000000000000000000, 1.000000000000000000 ) ) ;
#3137 = AXIS2_PLACEMENT_3D ( 'NONE', #9823, #34037, #11824 ) ;
#3138 = CARTESIAN_POINT ( 'NONE',  ( 1.039999999999999813, 14.89726405156260114, -31.02351007835961383 ) ) ;
#3139 = PLANE ( 'NONE',  #17507 ) ;
#3140 = FACE_OUTER_BOUND ( 'NONE', #12161, .T. ) ;
#3141 = ORIENTED_EDGE ( 'NONE', *, *, #25780, .T. ) ;
#3142 = TOROIDAL_SURFACE ( 'NONE', #7680, 30.47050528711511674, 8.000000000000000000 ) ;
#3143 = AXIS2_PLACEMENT_3D ( 'NONE', #3833, #12401, #9707 ) ;
#3144 = DIRECTION ( 'NONE',  ( 0.000000000000000000, 1.836970198721029441E-16, -1.000000000000000000 ) ) ;
#3145 = DIRECTION ( 'NONE',  ( -0.000000000000000000, -0.000000000000000000, -1.000000000000000000 ) ) ;
#3146 = DIRECTION ( 'NONE',  ( 0.000000000000000000, 1.836970198721029441E-16, -1.000000000000000000 ) ) ;
#3147 = ORIENTED_EDGE ( 'NONE', *, *, #25539, .T. ) ;
#3148 = VECTOR ( 'NONE', #24505, 1000.000000000000000 ) ;
#3149 = CYLINDRICAL_SURFACE ( 'NONE', #3018, 4.750000000000004441 ) ;
#3150 = VERTEX_POINT ( 'NONE', #20353 ) ;
#3151 = DIRECTION ( 'NONE',  ( 0.000000000000000000, 0.000000000000000000, 1.000000000000000000 ) ) ;
#3153 = CIRCLE ( 'NONE', #15676, 4.000000000000003553 ) ;
#3152 = DIRECTION ( 'NONE',  ( 0.000000000000000000, -1.000000000000000000, 0.000000000000000000 ) ) ;
#3154 = ORIENTED_EDGE ( 'NONE', *, *, #12208, .F. ) ;
#3155 = EDGE_CURVE ( 'NONE', #29056, #20661, #14844, .T. ) ;
#3156 = DIRECTION ( 'NONE',  ( -1.000000000000000000, -0.000000000000000000, -0.000000000000000000 ) ) ;
#3157 = CARTESIAN_POINT ( 'NONE',  ( 18.19419936998243870, -33.21164777187627237, 68.31122994652405112 ) ) ;
#3158 = CARTESIAN_POINT ( 'NONE',  ( -9.410814080250917257, 36.67205378194064735, 68.31122994652405112 ) ) ;
#3159 = EDGE_CURVE ( 'NONE', #16454, #2208, #775, .T. ) ;
#3160 = ORIENTED_EDGE ( 'NONE', *, *, #8197, .F. ) ;
#3161 = AXIS2_PLACEMENT_3D ( 'NONE', #30807, #3907, #14799 ) ;
#3162 = EDGE_CURVE ( 'NONE', #11635, #11447, #12343, .T. ) ;
#3163 = DIRECTION ( 'NONE',  ( 0.1063910735369155841, -0.9943243633099125844, -3.335902418025060287E-15 ) ) ;
#3164 = DIRECTION ( 'NONE',  ( 0.000000000000000000, 6.123233995736766036E-17, 1.000000000000000000 ) ) ;
#3165 = EDGE_CURVE ( 'NONE', #24095, #11612, #9550, .T. ) ;
#3166 = ORIENTED_EDGE ( 'NONE', *, *, #32162, .F. ) ;
#3167 = AXIS2_PLACEMENT_3D ( 'NONE', #28712, #31212, #3796 ) ;
#3168 = CARTESIAN_POINT ( 'NONE',  ( 0.000000000000000000, 3.524919873834583163E-15, 68.31122994652405112 ) ) ;
#3169 = LINE ( 'NONE', #19382, #26083 ) ;
#3170 = DIRECTION ( 'NONE',  ( 0.000000000000000000, 0.000000000000000000, -1.000000000000000000 ) ) ;
#3171 = CARTESIAN_POINT ( 'NONE',  ( -104.8237380854588707, -5.114955647091109725, 5.485182652933519698 ) ) ;
#3172 = ITEM_DEFINED_TRANSFORMATION ( 'NONE', 'NONE', #14431,  #28566 ) ;
#3173 = VERTEX_POINT ( 'NONE', #3606 ) ;
#3174 = ORIENTED_EDGE ( 'NONE', *, *, #4000, .T. ) ;
#3175 = VERTEX_POINT ( 'NONE', #17168 ) ;
#3176 = CARTESIAN_POINT ( 'NONE',  ( 26.97014235612466493, -26.57093094961043889, 68.31122994652405112 ) ) ;
#3177 = VECTOR ( 'NONE', #23782, 1000.000000000000000 ) ;
#3178 = ADVANCED_FACE ( 'NONE', ( #30503 ), #6098, .F. ) ;
#3179 = PLANE ( 'NONE',  #9751 ) ;
#3180 = CARTESIAN_POINT ( 'NONE',  ( -19.99999999999998934, 134.9999999999999432, -186.9999999999999716 ) ) ;
#3181 = ORIENTED_EDGE ( 'NONE', *, *, #13503, .T. ) ;
#3182 = AXIS2_PLACEMENT_3D ( 'NONE', #21257, #29272, #29085 ) ;
#3183 = ORIENTED_EDGE ( 'NONE', *, *, #29865, .T. ) ;
#3184 = CARTESIAN_POINT ( 'NONE',  ( -7.700000000000000178, 0.000000000000000000, -16.00000000000000000 ) ) ;
#3185 = ORIENTED_EDGE ( 'NONE', *, *, #4085, .T. ) ;
#3186 = DIRECTION ( 'NONE',  ( 0.000000000000000000, 1.000000000000000000, 5.053935297177146739E-49 ) ) ;
#3187 = FACE_OUTER_BOUND ( 'NONE', #22845, .T. ) ;
#3188 = ORIENTED_EDGE ( 'NONE', *, *, #16496, .F. ) ;
#3189 = ORIENTED_EDGE ( 'NONE', *, *, #11960, .T. ) ;
#3190 = VECTOR ( 'NONE', #5924, 1000.000000000000000 ) ;
#3191 = CARTESIAN_POINT ( 'NONE',  ( -7.176301005103106867, -1.505030548027689319, -0.7520000000000004459 ) ) ;
#3192 = EDGE_LOOP ( 'NONE', ( #16759, #10547, #21688, #33457, #35003, #10147 ) ) ;
#3193 = VECTOR ( 'NONE', #12968, 1000.000000000000000 ) ;
#3194 = CARTESIAN_POINT ( 'NONE',  ( 7.699999999999998401, 1.959434878635765131E-15, 16.00000000000000000 ) ) ;
#3195 = CARTESIAN_POINT ( 'NONE',  ( -12.00000000000001066, -24.99999999999999289, -154.9999999999999716 ) ) ;
#3196 = CARTESIAN_POINT ( 'NONE',  ( 2.789999999999999147, -0.3931553186915530129, 31.08824725498900321 ) ) ;
#3197 = DIRECTION ( 'NONE',  ( 0.000000000000000000, -1.224646799147353454E-16, 1.000000000000000000 ) ) ;
#3198 = CARTESIAN_POINT ( 'NONE',  ( 19.99999999999996092, -134.9999999999999716, 187.0000000000000000 ) ) ;
#3199 = DIRECTION ( 'NONE',  ( 1.000000000000000000, 0.000000000000000000, 0.000000000000000000 ) ) ;
#3200 = DIRECTION ( 'NONE',  ( -0.000000000000000000, 1.000000000000000000, -0.000000000000000000 ) ) ;
#3201 = VECTOR ( 'NONE', #14521, 1000.000000000000000 ) ;
#3202 = EDGE_CURVE ( 'NONE', #20895, #30258, #14676, .T. ) ;
#3203 = ORIENTED_EDGE ( 'NONE', *, *, #26828, .T. ) ;
#3204 = DIRECTION ( 'NONE',  ( 0.1063910735368947813, -0.9943243633099144718, -3.335902418024520312E-15 ) ) ;
#3205 = EDGE_CURVE ( 'NONE', #3784, #32269, #3859, .T. ) ;
#3206 = ORIENTED_EDGE ( 'NONE', *, *, #4973, .T. ) ;
#3207 = VERTEX_POINT ( 'NONE', #8962 ) ;
#3208 = EDGE_CURVE ( 'NONE', #13474, #14034, #10695, .T. ) ;
#3209 = CARTESIAN_POINT ( 'NONE',  ( -36.04853892210773836, 11.59936550071286376, 68.31122994652405112 ) ) ;
#3210 = VECTOR ( 'NONE', #25103, 1000.000000000000000 ) ;
#3211 = EDGE_CURVE ( 'NONE', #27122, #27900, #17528, .T. ) ;
#3212 = CARTESIAN_POINT ( 'NONE',  ( -410.0000000000000568, 104.9999999999999858, -162.9999999999999716 ) ) ;
#3213 = EDGE_CURVE ( 'NONE', #5389, #22114, #19236, .T. ) ;
#3214 = SHAPE_DEFINITION_REPRESENTATION ( #3232, #11185 ) ;
#3215 = ORIENTED_EDGE ( 'NONE', *, *, #32034, .F. ) ;
#3216 = DIRECTION ( 'NONE',  ( 0.000000000000000000, 0.000000000000000000, 1.000000000000000000 ) ) ;
#3217 = CONTEXT_DEPENDENT_SHAPE_REPRESENTATION ( #15366, #10453 ) ;
#3219 = DIRECTION ( 'NONE',  ( -1.000000000000000000, -3.040835319149746090E-31, -1.232595164407830946E-32 ) ) ;
#3218 = DIRECTION ( 'NONE',  ( 0.000000000000000000, -0.5000000000000008882, 0.8660254037844382635 ) ) ;
#3220 = VERTEX_POINT ( 'NONE', #28360 ) ;
#3221 = ORIENTED_EDGE ( 'NONE', *, *, #29312, .F. ) ;
#3222 = CARTESIAN_POINT ( 'NONE',  ( 2.789999999999999147, 24.98605633783575897, -17.38589710834512658 ) ) ;
#3223 = CARTESIAN_POINT ( 'NONE',  ( -1.030735741678193262, 1.713938105891546382, 3.180000000000000160 ) ) ;
#3225 = EDGE_CURVE ( 'NONE', #32722, #29816, #4124, .T. ) ;
#3224 = CARTESIAN_POINT ( 'NONE',  ( 129.3530333899765594, 6.000000000000000000, 57.49999999999999289 ) ) ;
#3226 = CARTESIAN_POINT ( 'NONE',  ( 11.99999999999999645, -145.0000000000000000, 162.9999999999999716 ) ) ;
#3227 = EDGE_LOOP ( 'NONE', ( #10350, #22448, #6055, #15690 ) ) ;
#3228 = DIRECTION ( 'NONE',  ( 0.000000000000000000, 1.000000000000000000, 0.000000000000000000 ) ) ;
#3229 = DIRECTION ( 'NONE',  ( -1.000000000000000000, 0.000000000000000000, 0.000000000000000000 ) ) ;
#3230 = PLANE ( 'NONE',  #15173 ) ;
#3231 = B_SPLINE_CURVE_WITH_KNOTS ( 'NONE', 3,
 ( #20756, #7206, #12930, #4528 ),
 .UNSPECIFIED., .F., .F.,
 ( 4, 4 ),
 ( 3.668583969174124871E-07, 0.0006881039678812997601 ),
 .UNSPECIFIED. ) ;
#3232 = PRODUCT_DEFINITION_SHAPE ( 'NONE', 'NONE',  #30332 ) ;
#3233 = ORIENTED_EDGE ( 'NONE', *, *, #10411, .F. ) ;
#3234 = CARTESIAN_POINT ( 'NONE',  ( -449.9999999999999432, -124.9999999999999858, -77.99999999999997158 ) ) ;
#3235 = AXIS2_PLACEMENT_3D ( 'NONE', #2573, #32990, #3102 ) ;
#3236 = FACE_OUTER_BOUND ( 'NONE', #2160, .T. ) ;
#3237 = FACE_OUTER_BOUND ( 'NONE', #2895, .T. ) ;
#3239 = CARTESIAN_POINT ( 'NONE',  ( 0.02815752724700520265, 1.322857909621847350, 13.50000000000000000 ) ) ;
#3238 = CARTESIAN_POINT ( 'NONE',  ( 12.00000000000001066, -32.99999999999997158, -154.9999999999999716 ) ) ;
#3240 = EDGE_CURVE ( 'NONE', #8469, #14037, #25142, .T. ) ;
#3241 = VECTOR ( 'NONE', #28099, 1000.000000000000000 ) ;
#3242 = VECTOR ( 'NONE', #18530, 1000.000000000000000 ) ;
#3243 = EDGE_CURVE ( 'NONE', #29665, #2517, #28645, .T. ) ;
#3244 = CARTESIAN_POINT ( 'NONE',  ( -418.0000000000000568, -109.0000000000000142, 155.0000000000000000 ) ) ;
#3245 = VERTEX_POINT ( 'NONE', #15362 ) ;
#3246 = CARTESIAN_POINT ( 'NONE',  ( -355.0000000000000000, -131.0000000000000000, 113.9999999999999858 ) ) ;
#3247 = PRESENTATION_STYLE_ASSIGNMENT (( #16625 ) ) ;
#3248 = ORIENTED_EDGE ( 'NONE', *, *, #16108, .F. ) ;
#3249 = VECTOR ( 'NONE', #31970, 1000.000000000000000 ) ;
#3250 = EDGE_LOOP ( 'NONE', ( #12103, #32729, #8584, #24155 ) ) ;
#3251 = VECTOR ( 'NONE', #10058, 1000.000000000000000 ) ;
#3252 = EDGE_CURVE ( 'NONE', #20130, #8592, #31876, .T. ) ;
#3253 = ADVANCED_FACE ( 'NONE', ( #31540 ), #2162, .T. ) ;
#3254 = ORIENTED_EDGE ( 'NONE', *, *, #5133, .T. ) ;
#3255 = FACE_OUTER_BOUND ( 'NONE', #18591, .T. ) ;
#3256 = ORIENTED_EDGE ( 'NONE', *, *, #24538, .F. ) ;
#3257 = ORIENTED_EDGE ( 'NONE', *, *, #5123, .T. ) ;
#3258 = DIRECTION ( 'NONE',  ( 1.000000000000000000, 0.000000000000000000, 0.000000000000000000 ) ) ;
#3259 = CIRCLE ( 'NONE', #16353, 7.999999999999979572 ) ;
#3260 = VECTOR ( 'NONE', #24940, 1000.000000000000000 ) ;
#3261 = ORIENTED_EDGE ( 'NONE', *, *, #20133, .F. ) ;
#3262 = DIRECTION ( 'NONE',  ( 0.000000000000000000, 0.000000000000000000, -1.000000000000000000 ) ) ;
#3263 = FACE_OUTER_BOUND ( 'NONE', #6795, .T. ) ;
#3264 = ORIENTED_EDGE ( 'NONE', *, *, #15668, .T. ) ;
#3265 = ORIENTED_EDGE ( 'NONE', *, *, #21739, .F. ) ;
#3266 = CARTESIAN_POINT ( 'NONE',  ( -499.9999999999999432, 136.9999999999999432, -162.9999999999999716 ) ) ;
#3267 = DIRECTION ( 'NONE',  ( -0.000000000000000000, -0.000000000000000000, -1.000000000000000000 ) ) ;
#3268 = FACE_OUTER_BOUND ( 'NONE', #26016, .T. ) ;
#3269 = DIRECTION ( 'NONE',  ( -1.000000000000000000, 0.000000000000000000, 0.000000000000000000 ) ) ;
#3270 = DIRECTION ( 'NONE',  ( 1.000000000000000000, 0.000000000000000000, 0.000000000000000000 ) ) ;
#3271 = ORIENTED_EDGE ( 'NONE', *, *, #18711, .F. ) ;
#3272 = AXIS2_PLACEMENT_3D ( 'NONE', #33391, #32855, #16686 ) ;
#3273 = CARTESIAN_POINT ( 'NONE',  ( -29.68486519896224962, 23.49918569563710946, 68.31122994652405112 ) ) ;
#3274 = LINE ( 'NONE', #11658, #4499 ) ;
#3275 = ORIENTED_EDGE ( 'NONE', *, *, #1947, .F. ) ;
#3276 = DIRECTION ( 'NONE',  ( 0.8568571761675893850, 0.5155538571770214018, -0.000000000000000000 ) ) ;
#3278 = EDGE_CURVE ( 'NONE', #10268, #4330, #12402, .T. ) ;
#3277 = FACE_OUTER_BOUND ( 'NONE', #12265, .T. ) ;
#3279 = CARTESIAN_POINT ( 'NONE',  ( -445.9999999999999432, 124.9999999999999432, -162.9999999999999716 ) ) ;
#3280 = ADVANCED_FACE ( 'NONE', ( #23875 ), #18571, .T. ) ;
#3281 = CARTESIAN_POINT ( 'NONE',  ( 1.040000000000001590, -33.26546734453813059, -8.820166447042128155 ) ) ;
#3282 = CARTESIAN_POINT ( 'NONE',  ( 212.5000000000000000, 9.184850993605147944E-16, -7.500000000000000000 ) ) ;
#3283 = ADVANCED_FACE ( 'NONE', ( #26193 ), #15720, .F. ) ;
#3284 = AXIS2_PLACEMENT_3D ( 'NONE', #11994, #17350, #6801 ) ;
#3285 = DIRECTION ( 'NONE',  ( 1.000000000000000000, 0.000000000000000000, -1.848892746611746966E-32 ) ) ;
#3286 = EDGE_LOOP ( 'NONE', ( #31431, #5977, #13422 ) ) ;
#3288 = CARTESIAN_POINT ( 'NONE',  ( -449.9999999999999432, 113.0000000000000000, -155.0000000000000000 ) ) ;
#3287 = DIRECTION ( 'NONE',  ( 0.000000000000000000, 1.000000000000000000, 5.145227585319922065E-49 ) ) ;
#3289 = EDGE_CURVE ( 'NONE', #14902, #13276, #32848, .T. ) ;
#3290 = VECTOR ( 'NONE', #2707, 1000.000000000000000 ) ;
#3291 = VECTOR ( 'NONE', #25073, 1000.000000000000000 ) ;
#3292 = ORIENTED_EDGE ( 'NONE', *, *, #10438, .T. ) ;
#3293 =( REPRESENTATION_RELATIONSHIP ('NONE','NONE', #23037, #15767 ) REPRESENTATION_RELATIONSHIP_WITH_TRANSFORMATION ( #34122 )SHAPE_REPRESENTATION_RELATIONSHIP( ) );
#3294 = CARTESIAN_POINT ( 'NONE',  ( -29.72561944762171393, -13.25111019240557475, -36.68877005347593467 ) ) ;
#3295 = ORIENTED_EDGE ( 'NONE', *, *, #23823, .F. ) ;
#3296 = ORIENTED_EDGE ( 'NONE', *, *, #5264, .F. ) ;
#3297 = VECTOR ( 'NONE', #31084, 1000.000000000000000 ) ;
#3298 = ORIENTED_EDGE ( 'NONE', *, *, #31333, .T. ) ;
#3299 = DIRECTION ( 'NONE',  ( 0.000000000000000000, 0.000000000000000000, -1.000000000000000000 ) ) ;
#3300 = DIRECTION ( 'NONE',  ( -1.000000000000000000, -0.000000000000000000, 0.000000000000000000 ) ) ;
#3301 = ORIENTED_EDGE ( 'NONE', *, *, #13740, .F. ) ;
#3302 = ORIENTED_EDGE ( 'NONE', *, *, #15393, .F. ) ;
#3303 = DIRECTION ( 'NONE',  ( -5.546364386991661285E-52, 0.000000000000000000, -1.000000000000000000 ) ) ;
#3304 = DIRECTION ( 'NONE',  ( 0.000000000000000000, 1.000000000000000000, 1.310824597558155437E-49 ) ) ;
#3305 = CIRCLE ( 'NONE', #9008, 2.036051781435517682 ) ;
#3306 = LINE ( 'NONE', #8116, #419 ) ;
#3307 = DIRECTION ( 'NONE',  ( 1.000000000000000000, 0.000000000000000000, 0.000000000000000000 ) ) ;
#3308 = ORIENTED_EDGE ( 'NONE', *, *, #19543, .T. ) ;
#3309 = ORIENTED_EDGE ( 'NONE', *, *, #25659, .F. ) ;
#3310 = PLANE ( 'NONE',  #31019 ) ;
#3311 = CARTESIAN_POINT ( 'NONE',  ( -500.0000000000000000, -145.0000000000000000, 155.0000000000000000 ) ) ;
#3312 = CARTESIAN_POINT ( 'NONE',  ( 0.000000000000000000, -27.53147453683416757, -13.05640081644872197 ) ) ;
#3313 = DIRECTION ( 'NONE',  ( 1.000000000000000000, 0.000000000000000000, 0.000000000000000000 ) ) ;
#3314 = CARTESIAN_POINT ( 'NONE',  ( 32.40067729534749219, 3.066020821660472517, 68.31122994652405112 ) ) ;
#3315 = VECTOR ( 'NONE', #11339, 1000.000000000000000 ) ;
#3316 = CARTESIAN_POINT ( 'NONE',  ( -442.0000000000000000, 104.9999999999999858, -155.0000000000000000 ) ) ;
#3317 = PLANE ( 'NONE',  #28821 ) ;
#3319 = VECTOR ( 'NONE', #11736, 1000.000000000000000 ) ;
#3318 = CARTESIAN_POINT ( 'NONE',  ( -7.654999999999999361, 0.000000000000000000, 3.930000000000000160 ) ) ;
#3320 = ORIENTED_EDGE ( 'NONE', *, *, #3030, .F. ) ;
#3321 = CARTESIAN_POINT ( 'NONE',  ( 1.749999999999999778, -33.26546734453825849, 8.820166447041632551 ) ) ;
#3322 = DIRECTION ( 'NONE',  ( -1.000000000000000000, -0.000000000000000000, -0.000000000000000000 ) ) ;
#3323 = VECTOR ( 'NONE', #28186, 1000.000000000000000 ) ;
#3324 = EDGE_CURVE ( 'NONE', #3609, #8625, #6118, .T. ) ;
#3325 = DIRECTION ( 'NONE',  ( -1.000000000000000000, -0.000000000000000000, -0.000000000000000000 ) ) ;
#3326 = ORIENTED_EDGE ( 'NONE', *, *, #21570, .F. ) ;
#3327 = EDGE_CURVE ( 'NONE', #3779, #6940, #4412, .T. ) ;
#3328 = LINE ( 'NONE', #22377, #8717 ) ;
#3329 = EDGE_LOOP ( 'NONE', ( #28799, #16866, #1609, #5261 ) ) ;
#3330 = DIRECTION ( 'NONE',  ( 1.000000000000000000, 0.000000000000000000, 0.000000000000000000 ) ) ;
#3331 = CYLINDRICAL_SURFACE ( 'NONE', #18823, 1.999999999999999556 ) ;
#3332 = VECTOR ( 'NONE', #25017, 1000.000000000000000 ) ;
#3333 = ORIENTED_EDGE ( 'NONE', *, *, #18846, .F. ) ;
#3334 = CARTESIAN_POINT ( 'NONE',  ( 0.000000000000000000, -7.666252171205713672, 29.49034198003804974 ) ) ;
#3335 = CARTESIAN_POINT ( 'NONE',  ( 11.62236370382047745, -30.39942490923500884, 68.31122994652405112 ) ) ;
#3336 = CARTESIAN_POINT ( 'NONE',  ( 9.199999999999999289, 15.58845726811990495, 0.000000000000000000 ) ) ;
#3337 = ORIENTED_EDGE ( 'NONE', *, *, #21203, .F. ) ;
#3338 = AXIS2_PLACEMENT_3D ( 'NONE', #17255, #14580, #5824 ) ;
#3339 = DIRECTION ( 'NONE',  ( 2.631201909438060585E-14, -5.396010391056496978E-16, 1.000000000000000000 ) ) ;
#3340 = FACE_OUTER_BOUND ( 'NONE', #18173, .T. ) ;
#3341 = ORIENTED_EDGE ( 'NONE', *, *, #14771, .T. ) ;
#3342 = CARTESIAN_POINT ( 'NONE',  ( 0.5288002468691824776, -9.581412748858038952, -31.98555481955064295 ) ) ;
#3343 = AXIS2_PLACEMENT_3D ( 'NONE', #4745, #18314, #26127 ) ;
#3344 = DIRECTION ( 'NONE',  ( 0.000000000000000000, 0.000000000000000000, 1.000000000000000000 ) ) ;
#3345 = LINE ( 'NONE', #11014, #7083 ) ;
#3346 = CARTESIAN_POINT ( 'NONE',  ( 2.789999999999999147, 27.60935207499552035, 12.89090262359662731 ) ) ;
#3347 = ITEM_DEFINED_TRANSFORMATION ( 'NONE', 'NONE', #1897,  #28566 ) ;
#3348 = VERTEX_POINT ( 'NONE', #34569 ) ;
#3349 = ORIENTED_EDGE ( 'NONE', *, *, #32285, .F. ) ;
#3350 = ORIENTED_EDGE ( 'NONE', *, *, #9971, .F. ) ;
#3351 = FILL_AREA_STYLE_COLOUR ( '', #34573 ) ;
#3352 = CARTESIAN_POINT ( 'NONE',  ( -499.9999999999999432, 140.9999999999999716, 187.0000000000000000 ) ) ;
#3353 = DIRECTION ( 'NONE',  ( 0.000000000000000000, 1.000000000000000000, 1.836970198721029688E-16 ) ) ;
#3354 = VECTOR ( 'NONE', #21223, 1000.000000000000000 ) ;
#3355 = EDGE_LOOP ( 'NONE', ( #19479, #17384, #22883, #25319 ) ) ;
#3356 = ORIENTED_EDGE ( 'NONE', *, *, #32473, .F. ) ;
#3357 = DIRECTION ( 'NONE',  ( 0.000000000000000000, 1.000000000000000000, 0.000000000000000000 ) ) ;
#3358 = ORIENTED_EDGE ( 'NONE', *, *, #8908, .T. ) ;
#3359 = EDGE_CURVE ( 'NONE', #26117, #13296, #26604, .T. ) ;
#3360 = CARTESIAN_POINT ( 'NONE',  ( -499.9999999999999432, 108.9999999999999858, 187.0000000000000000 ) ) ;
#3361 = CARTESIAN_POINT ( 'NONE',  ( 11.99999999999999645, -124.9999999999999432, -154.9999999999999716 ) ) ;
#3362 = ORIENTED_EDGE ( 'NONE', *, *, #17017, .F. ) ;
#3363 = VECTOR ( 'NONE', #22538, 1000.000000000000000 ) ;
#3364 = ORIENTED_EDGE ( 'NONE', *, *, #28648, .F. ) ;
#3365 = CARTESIAN_POINT ( 'NONE',  ( 0.000000000000000000, -44.99999999999997868, 87.49999999999998579 ) ) ;
#3366 = EDGE_CURVE ( 'NONE', #25284, #27727, #29228, .T. ) ;
#3367 = DIRECTION ( 'NONE',  ( 0.000000000000000000, 1.224646799147346305E-16, 1.000000000000000000 ) ) ;
#3368 = ORIENTED_EDGE ( 'NONE', *, *, #1367, .T. ) ;
#3369 = EDGE_CURVE ( 'NONE', #22969, #31238, #2170, .T. ) ;
#3370 = CARTESIAN_POINT ( 'NONE',  ( 0.000000000000000000, 2.281310696040539424E-14, -36.68877005347592757 ) ) ;
#3371 =( NAMED_UNIT ( * ) SI_UNIT ( $, .STERADIAN. ) SOLID_ANGLE_UNIT ( ) );
#3372 = CARTESIAN_POINT ( 'NONE',  ( -20.00000000000007461, 108.9999999999999858, -187.0000000000000000 ) ) ;
#3373 = CIRCLE ( 'NONE', #11906, 15.69999999999999929 ) ;
#3374 = LINE ( 'NONE', #714, #27619 ) ;
#3375 = CARTESIAN_POINT ( 'NONE',  ( -99.88497961182923746, -0.3417625387765687028, 12.50000000000000178 ) ) ;
#3376 = CARTESIAN_POINT ( 'NONE',  ( -499.9999999999999432, -137.0000000000000000, -194.9999999999999716 ) ) ;
#3377 = CARTESIAN_POINT ( 'NONE',  ( -361.0000000000000000, -125.0000000000000284, 164.9999999999999716 ) ) ;
#3378 = EDGE_LOOP ( 'NONE', ( #14733, #5601, #22053, #17205 ) ) ;
#3379 = VECTOR ( 'NONE', #4134, 1000.000000000000000 ) ;
#3380 = ORIENTED_EDGE ( 'NONE', *, *, #16494, .T. ) ;
#3381 = DIRECTION ( 'NONE',  ( 2.631201909438060269E-14, -5.396010391056495992E-16, 0.9999999999999998890 ) ) ;
#3382 = ORIENTED_EDGE ( 'NONE', *, *, #12489, .F. ) ;
#3383 = VERTEX_POINT ( 'NONE', #7675 ) ;
#3384 = CARTESIAN_POINT ( 'NONE',  ( 2.606462031291651993, 12.63602821951805133, 29.69442701139049134 ) ) ;
#3385 = LINE ( 'NONE', #16238, #19929 ) ;
#3386 = APPLICATION_PROTOCOL_DEFINITION ( 'draft international standard', 'automotive_design', 1998, #29647 ) ;
#3387 = ORIENTED_EDGE ( 'NONE', *, *, #10175, .T. ) ;
#3388 = DIRECTION ( 'NONE',  ( -0.000000000000000000, 1.000000000000000000, -0.000000000000000000 ) ) ;
#3389 = CARTESIAN_POINT ( 'NONE',  ( -100.4172690689928373, -2.278159677709879816, -12.29156386665007439 ) ) ;
#3390 = VECTOR ( 'NONE', #6877, 1000.000000000000000 ) ;
#3391 = ITEM_DEFINED_TRANSFORMATION ( 'NONE', 'NONE', #17305,  #28566 ) ;
#3393 = FACE_OUTER_BOUND ( 'NONE', #18212, .T. ) ;
#3392 = DIRECTION ( 'NONE',  ( -1.000000000000000000, -0.000000000000000000, -0.000000000000000000 ) ) ;
#3394 = ORIENTED_EDGE ( 'NONE', *, *, #20566, .T. ) ;
#3395 = ORIENTED_EDGE ( 'NONE', *, *, #7047, .F. ) ;
#3396 = CARTESIAN_POINT ( 'NONE',  ( 27.64943126350854286, -17.16721653852534146, 68.31122994652405112 ) ) ;
#3397 = EDGE_CURVE ( 'NONE', #7267, #34651, #12693, .T. ) ;
#3398 = FACE_OUTER_BOUND ( 'NONE', #19137, .T. ) ;
#3399 = CARTESIAN_POINT ( 'NONE',  ( 2.783107613148426029, -27.79373726981387449, 13.43326644626213806 ) ) ;
#3400 = ORIENTED_EDGE ( 'NONE', *, *, #10997, .F. ) ;
#3401 = LINE ( 'NONE', #16434, #15225 ) ;
#3402 = DIRECTION ( 'NONE',  ( 0.000000000000000000, -1.000000000000000000, -1.836970198721029934E-16 ) ) ;
#3403 = DIRECTION ( 'NONE',  ( 0.000000000000000000, 0.000000000000000000, -1.000000000000000000 ) ) ;
#3404 = VERTEX_POINT ( 'NONE', #1815 ) ;
#3405 = EDGE_CURVE ( 'NONE', #5775, #19234, #13557, .T. ) ;
#3406 = FACE_OUTER_BOUND ( 'NONE', #2479, .T. ) ;
#3407 = FACE_OUTER_BOUND ( 'NONE', #30676, .T. ) ;
#3408 = EDGE_CURVE ( 'NONE', #17794, #20784, #18679, .T. ) ;
#3409 = CARTESIAN_POINT ( 'NONE',  ( -37.12776225901827587, -7.411627343331159246, 68.31122994652405112 ) ) ;
#3411 = CARTESIAN_POINT ( 'NONE',  ( 0.5390048853414316499, 5.257018938344287129, 13.49999999999999822 ) ) ;
#3410 = LINE ( 'NONE', #5716, #12773 ) ;
#3412 = EDGE_CURVE ( 'NONE', #2971, #25849, #34931, .T. ) ;
#3413 = CARTESIAN_POINT ( 'NONE',  ( -5.021133111224886036, 6.201984591278717041, -67.50000000000000000 ) ) ;
#3414 = ORIENTED_EDGE ( 'NONE', *, *, #34154, .F. ) ;
#3415 = DIRECTION ( 'NONE',  ( 1.000000000000000000, 0.000000000000000000, -1.848892746611746966E-32 ) ) ;
#3416 = DIRECTION ( 'NONE',  ( 0.000000000000000000, 0.000000000000000000, -1.000000000000000000 ) ) ;
#3417 = ADVANCED_FACE ( 'NONE', ( #1645 ), #23356, .T. ) ;
#3418 = AXIS2_PLACEMENT_3D ( 'NONE', #16063, #32404, #23869 ) ;
#3419 = EDGE_LOOP ( 'NONE', ( #34031, #18703, #22977, #1042 ) ) ;
#3420 = ORIENTED_EDGE ( 'NONE', *, *, #4352, .F. ) ;
#3421 = EDGE_LOOP ( 'NONE', ( #14691, #9777, #5394, #24495 ) ) ;
#3422 = CARTESIAN_POINT ( 'NONE',  ( 2.790000000000000924, 0.000000000000000000, 0.000000000000000000 ) ) ;
#3423 = ORIENTED_EDGE ( 'NONE', *, *, #24255, .T. ) ;
#3424 = ORIENTED_EDGE ( 'NONE', *, *, #34181, .T. ) ;
#3425 = DIRECTION ( 'NONE',  ( 1.000000000000000000, 0.000000000000000000, -1.232595164407831220E-32 ) ) ;
#3426 = CONTEXT_DEPENDENT_SHAPE_REPRESENTATION ( #6718, #12492 ) ;
#3427 = ORIENTED_EDGE ( 'NONE', *, *, #26103, .F. ) ;
#3428 = CARTESIAN_POINT ( 'NONE',  ( 32.81769769215652133, 18.87860345536237006, 68.31122994652405112 ) ) ;
#3429 = LINE ( 'NONE', #27821, #6305 ) ;
#3430 = VERTEX_POINT ( 'NONE', #2693 ) ;
#3431 = ORIENTED_EDGE ( 'NONE', *, *, #482, .F. ) ;
#3432 = DIRECTION ( 'NONE',  ( 0.5155538571770215128, -0.8568571761675892740, 0.000000000000000000 ) ) ;
#3434 = CYLINDRICAL_SURFACE ( 'NONE', #15232, 7.999999999999979572 ) ;
#3433 = VECTOR ( 'NONE', #34847, 1000.000000000000000 ) ;
#3435 = DIRECTION ( 'NONE',  ( 0.9868265225415266961, 0.1617819965527614590, 2.971887063570111902E-17 ) ) ;
#3436 = DIRECTION ( 'NONE',  ( 0.000000000000000000, 1.836970198721029934E-16, -1.000000000000000000 ) ) ;
#3437 = LINE ( 'NONE', #31041, #31881 ) ;
#3438 = ORIENTED_EDGE ( 'NONE', *, *, #28604, .T. ) ;
#3439 = VECTOR ( 'NONE', #34121, 1000.000000000000000 ) ;
#3440 = CARTESIAN_POINT ( 'NONE',  ( -361.0000000000000000, 134.9999999999999716, 113.9999999999999858 ) ) ;
#3441 = CARTESIAN_POINT ( 'NONE',  ( 0.5248942630475922355, -2.869810969760784314, -33.25620129461683661 ) ) ;
#3442 = ORIENTED_EDGE ( 'NONE', *, *, #32221, .T. ) ;
#3443 = CARTESIAN_POINT ( 'NONE',  ( 110.7380848894536598, 7.027127293105233764E-16, 60.00000000000000000 ) ) ;
#3444 = CARTESIAN_POINT ( 'NONE',  ( 0.000000000000000000, -55.00000000000000711, -154.9999999999999716 ) ) ;
#3445 = DIRECTION ( 'NONE',  ( 0.6473862847818279143, -0.7621620551276363509, -1.400068981865442877E-16 ) ) ;
#3446 = EDGE_CURVE ( 'NONE', #27961, #23165, #3041, .T. ) ;
#3447 = CARTESIAN_POINT ( 'NONE',  ( 100.4805201888165982, 3.554679846740550264, -6.612701241491620863 ) ) ;
#3448 =( LENGTH_UNIT ( ) NAMED_UNIT ( * ) SI_UNIT ( .MILLI., .METRE. ) );
#3449 = VECTOR ( 'NONE', #34223, 1000.000000000000000 ) ;
#3450 = EDGE_CURVE ( 'NONE', #1565, #1194, #1607, .T. ) ;
#3451 = EDGE_CURVE ( 'NONE', #6854, #18398, #14229, .T. ) ;
#3452 = DIRECTION ( 'NONE',  ( 0.000000000000000000, -1.000000000000000000, 3.421138828918010427E-49 ) ) ;
#3454 = EDGE_LOOP ( 'NONE', ( #14838, #22488, #7870, #3427 ) ) ;
#3453 = AXIS2_PLACEMENT_3D ( 'NONE', #18456, #10784, #24285 ) ;
#3455 = DIRECTION ( 'NONE',  ( 0.000000000000000000, 1.836970198721029688E-16, -1.000000000000000000 ) ) ;
#3457 = CARTESIAN_POINT ( 'NONE',  ( 12.00000000000001066, 144.9999999999999716, -155.0000000000000000 ) ) ;
#3456 = DIRECTION ( 'NONE',  ( 1.000000000000000000, 0.000000000000000000, 0.000000000000000000 ) ) ;
#3458 = ORIENTED_EDGE ( 'NONE', *, *, #1462, .F. ) ;
#3459 = LINE ( 'NONE', #33191, #30237 ) ;
#3460 = CARTESIAN_POINT ( 'NONE',  ( 0.000000000000000000, 3.524919873834583163E-15, 68.31122994652405112 ) ) ;
#3461 = AXIS2_PLACEMENT_3D ( 'NONE', #12744, #34444, #26425 ) ;
#3462 = ORIENTED_EDGE ( 'NONE', *, *, #32045, .T. ) ;
#3463 = EDGE_CURVE ( 'NONE', #9737, #34245, #25, .T. ) ;
#3464 = CIRCLE ( 'NONE', #27913, 1.154999999999999805 ) ;
#3465 = ORIENTED_EDGE ( 'NONE', *, *, #10528, .F. ) ;
#3466 = PLANE ( 'NONE',  #28161 ) ;
#3467 = ORIENTED_EDGE ( 'NONE', *, *, #9872, .T. ) ;
#3468 = VERTEX_POINT ( 'NONE', #10890 ) ;
#3469 = FACE_OUTER_BOUND ( 'NONE', #30331, .T. ) ;
#3470 = PRODUCT_DEFINITION_SHAPE ( 'NONE', 'NONE',  #35140 ) ;
#3471 = EDGE_CURVE ( 'NONE', #17629, #7314, #13735, .T. ) ;
#3472 = CARTESIAN_POINT ( 'NONE',  ( -6.637260778198712075, 37.28255902965928215, 68.31122994652405112 ) ) ;
#3473 = ADVANCED_FACE ( 'NONE', ( #204 ), #21735, .T. ) ;
#3474 = DIRECTION ( 'NONE',  ( -1.000000000000000000, 0.000000000000000000, -0.000000000000000000 ) ) ;
#3475 = AXIS2_PLACEMENT_3D ( 'NONE', #25994, #12657, #33480 ) ;
#3476 = CARTESIAN_POINT ( 'NONE',  ( 32.40067729534750640, 3.066020821660472961, 68.31122994652405112 ) ) ;
#3477 = VERTEX_POINT ( 'NONE', #16068 ) ;
#3478 = ORIENTED_EDGE ( 'NONE', *, *, #32543, .F. ) ;
#3479 = AXIS2_PLACEMENT_3D ( 'NONE', #31481, #7085, #23468 ) ;
#3480 = CARTESIAN_POINT ( 'NONE',  ( -349.0000000000000000, -125.0000000000000284, 185.0000000000000000 ) ) ;
#3481 = CARTESIAN_POINT ( 'NONE',  ( 11.99999999999999645, 112.9999999999999574, 155.0000000000000000 ) ) ;
#3482 = VECTOR ( 'NONE', #7845, 1000.000000000000000 ) ;
#3483 = CIRCLE ( 'NONE', #31905, 32.54542015209057126 ) ;
#3484 = LINE ( 'NONE', #14370, #15207 ) ;
#3485 = EDGE_CURVE ( 'NONE', #16627, #22969, #8207, .T. ) ;
#3486 = DIRECTION ( 'NONE',  ( 0.000000000000000000, 0.000000000000000000, -1.000000000000000000 ) ) ;
#3487 = DIRECTION ( 'NONE',  ( 0.000000000000000000, 0.000000000000000000, -1.000000000000000000 ) ) ;
#3488 = DIRECTION ( 'NONE',  ( -0.000000000000000000, -0.000000000000000000, 1.000000000000000000 ) ) ;
#3489 = LINE ( 'NONE', #33031, #24934 ) ;
#3490 = VERTEX_POINT ( 'NONE', #14094 ) ;
#3491 = LINE ( 'NONE', #28061, #32689 ) ;
#3492 = CARTESIAN_POINT ( 'NONE',  ( -20.00000000000007461, 108.9999999999999858, -162.9999999999999716 ) ) ;
#3493 = CIRCLE ( 'NONE', #12033, 30.47050528711512030 ) ;
#3494 = DIRECTION ( 'NONE',  ( 1.000000000000000000, -0.000000000000000000, -0.000000000000000000 ) ) ;
#3495 = ORIENTED_EDGE ( 'NONE', *, *, #18707, .F. ) ;
#3496 = ADVANCED_FACE ( 'NONE', ( #26899 ), #11071, .T. ) ;
#3497 =( REPRESENTATION_RELATIONSHIP ('NONE','NONE', #23037, #11185 ) REPRESENTATION_RELATIONSHIP_WITH_TRANSFORMATION ( #2689 )SHAPE_REPRESENTATION_RELATIONSHIP( ) );
#3498 = CARTESIAN_POINT ( 'NONE',  ( 0.000000000000000000, 0.000000000000000000, 0.000000000000000000 ) ) ;
#3499 = VERTEX_POINT ( 'NONE', #29933 ) ;
#3500 = LINE ( 'NONE', #6697, #30980 ) ;
#3501 = CARTESIAN_POINT ( 'NONE',  ( -99.88497961182922324, 0.3420146137956281973, 12.50000000000000178 ) ) ;
#3503 = VERTEX_POINT ( 'NONE', #24569 ) ;
#3502 = AXIS2_PLACEMENT_3D ( 'NONE', #10283, #12969, #7958 ) ;
#3504 = CIRCLE ( 'NONE', #103, 3.999999999999976019 ) ;
#3505 = CARTESIAN_POINT ( 'NONE',  ( 1.749999999999999778, 31.89769921722987434, 12.91988538846969803 ) ) ;
#3506 = AXIS2_PLACEMENT_3D ( 'NONE', #27240, #10710, #21560 ) ;
#3507 = CARTESIAN_POINT ( 'NONE',  ( -19.99999999999998934, -137.0000000000000000, 174.9999999999999432 ) ) ;
#3508 = CARTESIAN_POINT ( 'NONE',  ( -363.0000000000000000, -125.0000000000000284, 181.0000000000000000 ) ) ;
#3509 = ORIENTED_EDGE ( 'NONE', *, *, #12209, .T. ) ;
#3510 = CARTESIAN_POINT ( 'NONE',  ( 850.5759694929395209, 1035.130795166948019, 1753.598338701304101 ) ) ;
#3511 = PLANE ( 'NONE',  #20460 ) ;
#3512 = ORIENTED_EDGE ( 'NONE', *, *, #30901, .T. ) ;
#3513 = CARTESIAN_POINT ( 'NONE',  ( 2.789999999999999591, 0.000000000000000000, -3.000000000000000000 ) ) ;
#3514 = AXIS2_PLACEMENT_3D ( 'NONE', #12608, #23450, #15455 ) ;
#3515 = ADVANCED_FACE ( 'NONE', ( #13394, #24227, #21920 ), #27431, .F. ) ;
#3516 = EDGE_CURVE ( 'NONE', #949, #4047, #24333, .T. ) ;
#3517 = FACE_OUTER_BOUND ( 'NONE', #29201, .T. ) ;
#3518 = LINE ( 'NONE', #22580, #5134 ) ;
#3519 = CONTEXT_DEPENDENT_SHAPE_REPRESENTATION ( #2819, #12331 ) ;
#3520 = ORIENTED_EDGE ( 'NONE', *, *, #1136, .F. ) ;
#3521 = ORIENTED_EDGE ( 'NONE', *, *, #16292, .F. ) ;
#3522 = ORIENTED_EDGE ( 'NONE', *, *, #30033, .F. ) ;
#3523 = FILL_AREA_STYLE_COLOUR ( '', #23226 ) ;
#3524 = LINE ( 'NONE', #15110, #21685 ) ;
#3525 = AXIS2_PLACEMENT_3D ( 'NONE', #28640, #17290, #20463 ) ;
#3526 = CARTESIAN_POINT ( 'NONE',  ( 2.789999999999999147, 17.11426446101199161, 26.96776559937732642 ) ) ;
#3527 = LINE ( 'NONE', #14766, #9119 ) ;
#3529 = ORIENTED_EDGE ( 'NONE', *, *, #2873, .T. ) ;
#3528 = CIRCLE ( 'NONE', #27979, 4.750000000000004441 ) ;
#3530 = ORIENTED_EDGE ( 'NONE', *, *, #9151, .T. ) ;
#3531 = DIRECTION ( 'NONE',  ( 0.000000000000000000, -1.000000000000000000, -1.131431318426415506E-52 ) ) ;
#3532 = AXIS2_PLACEMENT_3D ( 'NONE', #27531, #3325, #27349 ) ;
#3533 = ORIENTED_EDGE ( 'NONE', *, *, #26277, .F. ) ;
#3534 = ADVANCED_FACE ( 'NONE', ( #30275 ), #30103, .T. ) ;
#3535 = CARTESIAN_POINT ( 'NONE',  ( 4.815661544189684840, -32.18716788982705168, 68.31122994652405112 ) ) ;
#3536 = DIRECTION ( 'NONE',  ( 1.000000000000000000, 0.000000000000000000, 0.000000000000000000 ) ) ;
#3537 = ORIENTED_EDGE ( 'NONE', *, *, #17476, .T. ) ;
#3538 = ORIENTED_EDGE ( 'NONE', *, *, #5675, .T. ) ;
#3539 = DIRECTION ( 'NONE',  ( 0.000000000000000000, 2.465190328815661892E-32, 1.000000000000000000 ) ) ;
#3540 = FACE_OUTER_BOUND ( 'NONE', #25135, .T. ) ;
#3541 = ORIENTED_EDGE ( 'NONE', *, *, #32779, .T. ) ;
#3542 = LINE ( 'NONE', #20288, #1593 ) ;
#3543 = DIRECTION ( 'NONE',  ( -0.000000000000000000, 1.836970198721029934E-16, -1.000000000000000000 ) ) ;
#3544 = CARTESIAN_POINT ( 'NONE',  ( 143.0000000000000568, -78.33668825982573480, -63.00000000000000000 ) ) ;
#3545 = DIRECTION ( 'NONE',  ( 1.000000000000000000, 0.000000000000000000, 0.000000000000000000 ) ) ;
#3546 = CYLINDRICAL_SURFACE ( 'NONE', #27335, 3.999999999999976019 ) ;
#3547 = CARTESIAN_POINT ( 'NONE',  ( -499.9999999999999432, -137.0000000000000000, -187.0000000000000000 ) ) ;
#3548 = EDGE_CURVE ( 'NONE', #18398, #25712, #33233, .T. ) ;
#3549 = CARTESIAN_POINT ( 'NONE',  ( 5.021133111224576062, 16.12922284503173742, -67.50000000000000000 ) ) ;
#3550 = VERTEX_POINT ( 'NONE', #32241 ) ;
#3551 = ORIENTED_EDGE ( 'NONE', *, *, #14484, .F. ) ;
#3552 = DIRECTION ( 'NONE',  ( 0.1063910735368947813, -0.9943243633099144718, -3.335902418024520312E-15 ) ) ;
#3553 = VECTOR ( 'NONE', #4364, 1000.000000000000000 ) ;
#3554 = ORIENTED_EDGE ( 'NONE', *, *, #25628, .F. ) ;
#3555 = VERTEX_POINT ( 'NONE', #5173 ) ;
#3556 = EDGE_CURVE ( 'NONE', #3555, #32705, #3305, .T. ) ;
#3557 = EDGE_CURVE ( 'NONE', #19034, #11831, #23790, .T. ) ;
#3558 = CARTESIAN_POINT ( 'NONE',  ( -20.00000000000004619, -134.9999999999999716, -162.9999999999999432 ) ) ;
#3559 = ADVANCED_FACE ( 'NONE', ( #11414 ), #500, .T. ) ;
#3560 = FACE_OUTER_BOUND ( 'NONE', #4914, .T. ) ;
#3561 = ITEM_DEFINED_TRANSFORMATION ( 'NONE', 'NONE', #11545,  #28566 ) ;
#3562 = ORIENTED_EDGE ( 'NONE', *, *, #9483, .F. ) ;
#3563 = DIRECTION ( 'NONE',  ( -1.000000000000000000, 0.000000000000000000, -0.000000000000000000 ) ) ;
#3564 =( LENGTH_UNIT ( ) NAMED_UNIT ( * ) SI_UNIT ( .MILLI., .METRE. ) );
#3566 = CARTESIAN_POINT ( 'NONE',  ( -110.1150203881707910, 0.000000000000000000, 60.00000000000000000 ) ) ;
#3565 = FACE_OUTER_BOUND ( 'NONE', #34074, .T. ) ;
#3567 = ORIENTED_EDGE ( 'NONE', *, *, #33673, .F. ) ;
#3568 = ORIENTED_EDGE ( 'NONE', *, *, #13544, .F. ) ;
#3569 = LINE ( 'NONE', #918, #32756 ) ;
#3570 = CARTESIAN_POINT ( 'NONE',  ( -449.9999999999999432, -112.9999999999999858, 155.0000000000000000 ) ) ;
#3571 = FACE_OUTER_BOUND ( 'NONE', #24598, .T. ) ;
#3572 = DIRECTION ( 'NONE',  ( -1.000000000000000000, -0.000000000000000000, -0.000000000000000000 ) ) ;
#3573 = ORIENTED_EDGE ( 'NONE', *, *, #14589, .F. ) ;
#3574 = CARTESIAN_POINT ( 'NONE',  ( 2.789999999999999147, -23.70329957282599764, 20.11932597908820242 ) ) ;
#3575 = DIRECTION ( 'NONE',  ( -0.000000000000000000, -0.000000000000000000, 1.000000000000000000 ) ) ;
#3576 = PRESENTATION_LAYER_ASSIGNMENT (  '', '', ( #9832 ) ) ;
#3577 = CIRCLE ( 'NONE', #25767, 3.999999999999976019 ) ;
#3578 = ORIENTED_EDGE ( 'NONE', *, *, #902, .F. ) ;
#3579 = CARTESIAN_POINT ( 'NONE',  ( -3.250000000000000000, -5.838643359331793015, 0.000000000000000000 ) ) ;
#3580 = DIRECTION ( 'NONE',  ( 0.000000000000000000, 0.000000000000000000, 1.000000000000000000 ) ) ;
#3581 = CARTESIAN_POINT ( 'NONE',  ( 17.88561705399011714, -27.19023860642122514, 68.31122994652405112 ) ) ;
#3583 = CARTESIAN_POINT ( 'NONE',  ( 11.99999999999999645, -145.0000000000000000, 194.9999999999999716 ) ) ;
#3582 = CYLINDRICAL_SURFACE ( 'NONE', #21847, 2.524999999999999467 ) ;
#3584 = UNCERTAINTY_MEASURE_WITH_UNIT (LENGTH_MEASURE( 1.000000000000000082E-05 ), #34719, 'distance_accuracy_value', 'NONE');
#3585 = CARTESIAN_POINT ( 'NONE',  ( 0.02407890056655738464, -11.07880054387200985, -29.04985141099774637 ) ) ;
#3586 = CARTESIAN_POINT ( 'NONE',  ( -6.500000000000000000, 0.000000000000000000, 5.429999999999999716 ) ) ;
#3587 = ORIENTED_EDGE ( 'NONE', *, *, #22055, .T. ) ;
#3588 = CARTESIAN_POINT ( 'NONE',  ( -442.0000000000000000, 105.0000000000000142, 104.0000000000000142 ) ) ;
#3589 = CARTESIAN_POINT ( 'NONE',  ( -36.94452915644502866, -7.381587800927575493, 17.40055616961943485 ) ) ;
#3590 = VERTEX_POINT ( 'NONE', #17656 ) ;
#3591 = EDGE_CURVE ( 'NONE', #25806, #32541, #4082, .T. ) ;
#3592 = VERTEX_POINT ( 'NONE', #1264 ) ;
#3593 = EDGE_CURVE ( 'NONE', #13790, #9326, #20313, .T. ) ;
#3594 = AXIS2_PLACEMENT_3D ( 'NONE', #32884, #8859, #19729 ) ;
#3596 = ADVANCED_FACE ( 'NONE', ( #3393 ), #31164, .T. ) ;
#3595 = B_SPLINE_CURVE_WITH_KNOTS ( 'NONE', 3,
 ( #30959, #6564, #34142, #28808, #17980, #15299 ),
 .UNSPECIFIED., .F., .F.,
 ( 4, 2, 4 ),
 ( 2.333473478908865889E-07, 0.001873431678079538970, 0.003746630008811186949 ),
 .UNSPECIFIED. ) ;
#3597 = TOROIDAL_SURFACE ( 'NONE', #22389, 10.30000000000000071, 0.3000000000000025424 ) ;
#3598 = VECTOR ( 'NONE', #16576, 1000.000000000000000 ) ;
#3599 = ORIENTED_EDGE ( 'NONE', *, *, #15508, .F. ) ;
#3600 = DIRECTION ( 'NONE',  ( 0.000000000000000000, 0.000000000000000000, -1.000000000000000000 ) ) ;
#3601 = EDGE_LOOP ( 'NONE', ( #10568, #22999, #7765, #906 ) ) ;
#3602 = ORIENTED_EDGE ( 'NONE', *, *, #11901, .T. ) ;
#3603 = EDGE_CURVE ( 'NONE', #10950, #22914, #30987, .T. ) ;
#3604 = CYLINDRICAL_SURFACE ( 'NONE', #32656, 3.999999999999976019 ) ;
#3605 = ORIENTED_EDGE ( 'NONE', *, *, #21510, .T. ) ;
#3606 = CARTESIAN_POINT ( 'NONE',  ( 11.99999999999995559, -145.0000000000000000, 155.0000000000000000 ) ) ;
#3607 = DIRECTION ( 'NONE',  ( 1.000000000000000000, 0.000000000000000000, 0.000000000000000000 ) ) ;
#3608 = ORIENTED_EDGE ( 'NONE', *, *, #33137, .T. ) ;
#3609 = VERTEX_POINT ( 'NONE', #14453 ) ;
#3610 = CARTESIAN_POINT ( 'NONE',  ( 0.000000000000000000, 6.992329373473909019E-15, 49.43553178847298568 ) ) ;
#3611 = CARTESIAN_POINT ( 'NONE',  ( 2.033800777031441243, -1.599833918847377801, -33.87742110695038633 ) ) ;
#3612 = ADVANCED_FACE ( 'NONE', ( #14273 ), #6589, .T. ) ;
#3613 = DIRECTION ( 'NONE',  ( 0.4198891015602652099, -0.9075754196709567845, 0.000000000000000000 ) ) ;
#3614 = CARTESIAN_POINT ( 'NONE',  ( -9.978866888775527855, 4.168562732279004202, -67.50000000000000000 ) ) ;
#3615 = FACE_OUTER_BOUND ( 'NONE', #22346, .T. ) ;
#3616 = ORIENTED_EDGE ( 'NONE', *, *, #26274, .F. ) ;
#3617 = DIRECTION ( 'NONE',  ( 0.000000000000000000, -0.7071067811865489050, -0.7071067811865462405 ) ) ;
#3618 = AXIS2_PLACEMENT_3D ( 'NONE', #3168, #11544, #30404 ) ;
#3619 = LINE ( 'NONE', #14152, #31231 ) ;
#3620 = ORIENTED_EDGE ( 'NONE', *, *, #30632, .T. ) ;
#3621 = DIRECTION ( 'NONE',  ( 1.000000000000000000, 0.000000000000000000, -1.232595164407831220E-32 ) ) ;
#3622 = CARTESIAN_POINT ( 'NONE',  ( 7.700000000000001954, 1.243016501134563095E-15, 9.999999999999994671 ) ) ;
#3623 = CARTESIAN_POINT ( 'NONE',  ( -20.02113311122488781, 6.201984591278717041, -67.50000000000000000 ) ) ;
#3624 = AXIS2_PLACEMENT_3D ( 'NONE', #6708, #12079, #17604 ) ;
#3625 = FACE_OUTER_BOUND ( 'NONE', #11815, .T. ) ;
#3626 = DIRECTION ( 'NONE',  ( 0.000000000000000000, -1.000000000000000000, 6.123233995736766036E-17 ) ) ;
#3627 = VECTOR ( 'NONE', #28725, 1000.000000000000000 ) ;
#3628 = AXIS2_PLACEMENT_3D ( 'NONE', #4941, #24162, #10654 ) ;
#3629 = CARTESIAN_POINT ( 'NONE',  ( -143.0000000000000568, -12.50000000000001066, 15.00000000000001243 ) ) ;
#3630 = VERTEX_POINT ( 'NONE', #22632 ) ;
#3631 = CARTESIAN_POINT ( 'NONE',  ( 15.99999999999998579, 136.9999999999999716, -175.0000000000000284 ) ) ;
#3633 = CARTESIAN_POINT ( 'NONE',  ( 0.02407890056655695096, 30.61125888652961891, 5.439165181699118889 ) ) ;
#3632 = DIRECTION ( 'NONE',  ( 0.000000000000000000, 1.836970198721029441E-16, -1.000000000000000000 ) ) ;
#3634 = ORIENTED_EDGE ( 'NONE', *, *, #24897, .T. ) ;
#3635 = PLANE ( 'NONE',  #13728 ) ;
#3636 = ORIENTED_EDGE ( 'NONE', *, *, #27071, .F. ) ;
#3637 = EDGE_LOOP ( 'NONE', ( #26902, #13289, #29468, #6440 ) ) ;
#3638 = VECTOR ( 'NONE', #28264, 1000.000000000000000 ) ;
#3639 = ORIENTED_EDGE ( 'NONE', *, *, #34607, .T. ) ;
#3640 = CARTESIAN_POINT ( 'NONE',  ( 105.1945178213486116, -5.738162003225207641, -4.829440634198706839 ) ) ;
#3641 = ORIENTED_EDGE ( 'NONE', *, *, #1684, .F. ) ;
#3642 = ORIENTED_EDGE ( 'NONE', *, *, #32787, .T. ) ;
#3643 = ADVANCED_FACE ( 'NONE', ( #28139 ), #17124, .F. ) ;
#3644 = CARTESIAN_POINT ( 'NONE',  ( -15.99999999999998579, 4.559999999999908127, -172.9900000000000091 ) ) ;
#3645 = AXIS2_PLACEMENT_3D ( 'NONE', #27958, #9269, #24755 ) ;
#3646 = EDGE_CURVE ( 'NONE', #17680, #27112, #22974, .T. ) ;
#3647 = CARTESIAN_POINT ( 'NONE',  ( -442.0000000000000000, -104.9999999999999574, -155.0000000000000000 ) ) ;
#3648 = LINE ( 'NONE', #11158, #1667 ) ;
#3649 = AXIS2_PLACEMENT_3D ( 'NONE', #10378, #4660, #26919 ) ;
#3650 = CARTESIAN_POINT ( 'NONE',  ( 2.789999999999999147, -25.77598557799260703, 16.24962337825793313 ) ) ;
#3651 = CARTESIAN_POINT ( 'NONE',  ( 0.1835381989597825725, 31.84255742294098113, -5.242117949250411080 ) ) ;
#3652 = EDGE_CURVE ( 'NONE', #18208, #7089, #8442, .T. ) ;
#3653 = ORIENTED_EDGE ( 'NONE', *, *, #32935, .T. ) ;
#3654 = EDGE_CURVE ( 'NONE', #34419, #7314, #17489, .T. ) ;
#3655 = EDGE_LOOP ( 'NONE', ( #19290, #9366, #26074, #21593 ) ) ;
#3656 = AXIS2_PLACEMENT_3D ( 'NONE', #9476, #6248, #33672 ) ;
#3657 = CARTESIAN_POINT ( 'NONE',  ( 0.7564103407256241862, -32.97789401874111093, 7.919772684712727440 ) ) ;
#3658 = CARTESIAN_POINT ( 'NONE',  ( 30.45781707305797070, -22.50252913745434924, 68.31122994652405112 ) ) ;
#3659 = DIRECTION ( 'NONE',  ( 1.000000000000000000, 0.000000000000000000, 5.546364386991661285E-52 ) ) ;
#3660 = AXIS2_PLACEMENT_3D ( 'NONE', #3422, #6260, #19651 ) ;
#3661 = DIRECTION ( 'NONE',  ( 0.000000000000000000, 0.000000000000000000, -1.000000000000000000 ) ) ;
#3662 = CARTESIAN_POINT ( 'NONE',  ( 19.99999999999998934, 136.9999999999999716, -155.0000000000000000 ) ) ;
#3663 = DIRECTION ( 'NONE',  ( 1.000000000000000000, 0.000000000000000000, -1.848892746611746966E-32 ) ) ;
#3664 = DIRECTION ( 'NONE',  ( 0.000000000000000000, 0.000000000000000000, 1.000000000000000000 ) ) ;
#3665 = ORIENTED_EDGE ( 'NONE', *, *, #25088, .T. ) ;
#3666 = LINE ( 'NONE', #11172, #30491 ) ;
#3667 = DIRECTION ( 'NONE',  ( 0.000000000000000000, 1.000000000000000000, 5.053935297177146739E-49 ) ) ;
#3668 = ADVANCED_FACE ( 'NONE', ( #30810 ), #25458, .T. ) ;
#3669 = DIRECTION ( 'NONE',  ( -0.9941379571543595972, 0.1081190184239420177, 1.986114147597514287E-17 ) ) ;
#3670 = ORIENTED_EDGE ( 'NONE', *, *, #2432, .F. ) ;
#3671 = AXIS2_PLACEMENT_3D ( 'NONE', #4170, #31411, #6491 ) ;
#3672 = CARTESIAN_POINT ( 'NONE',  ( 19.99999999999990763, -134.9999999999999716, -186.9999999999999716 ) ) ;
#3673 = EDGE_LOOP ( 'NONE', ( #24652, #23698 ) ) ;
#3674 = CARTESIAN_POINT ( 'NONE',  ( 8.000000000000000000, 0.000000000000000000, 0.000000000000000000 ) ) ;
#3675 = VECTOR ( 'NONE', #27004, 1000.000000000000000 ) ;
#3676 = CARTESIAN_POINT ( 'NONE',  ( -100.9388899323377586, 3.127595108844668292, 12.10573782681415267 ) ) ;
#3677 = ORIENTED_EDGE ( 'NONE', *, *, #21645, .F. ) ;
#3678 = EDGE_CURVE ( 'NONE', #21237, #12316, #12133, .T. ) ;
#3679 = VECTOR ( 'NONE', #10160, 1000.000000000000000 ) ;
#3680 = EDGE_CURVE ( 'NONE', #29286, #8432, #26053, .T. ) ;
#3681 = ORIENTED_EDGE ( 'NONE', *, *, #11147, .F. ) ;
#3682 = CIRCLE ( 'NONE', #1429, 2.036051781435510577 ) ;
#3683 = CARTESIAN_POINT ( 'NONE',  ( -31.68358972719163091, 7.440061483287550459, -36.68877005347593467 ) ) ;
#3684 = CARTESIAN_POINT ( 'NONE',  ( -15.99999999999998579, 112.9999999999999574, -175.0000000000000284 ) ) ;
#3685 = CARTESIAN_POINT ( 'NONE',  ( 0.000000000000000000, 0.000000000000000000, 87.50000000000000000 ) ) ;
#3686 = PRODUCT_DEFINITION_SHAPE ( 'NONE', 'NONE',  #35218 ) ;
#3687 = ORIENTED_EDGE ( 'NONE', *, *, #6923, .T. ) ;
#3688 = DIRECTION ( 'NONE',  ( -7.893605728314051750E-14, 1.618803117314786530E-15, 1.000000000000000000 ) ) ;
#3689 = CARTESIAN_POINT ( 'NONE',  ( 2.783128731155445124, -30.26101440722778335, -6.099076262612814325 ) ) ;
#3690 = ORIENTED_EDGE ( 'NONE', *, *, #18711, .T. ) ;
#3691 = FACE_OUTER_BOUND ( 'NONE', #5204, .T. ) ;
#3692 =( NAMED_UNIT ( * ) SI_UNIT ( $, .STERADIAN. ) SOLID_ANGLE_UNIT ( ) );
#3693 = AXIS2_PLACEMENT_3D ( 'NONE', #17303, #22449, #25453 ) ;
#3694 = CARTESIAN_POINT ( 'NONE',  ( 11.99999999999999645, -137.0000000000000000, -155.0000000000000284 ) ) ;
#3695 = DIRECTION ( 'NONE',  ( -1.000000000000000000, -0.000000000000000000, -0.000000000000000000 ) ) ;
#3696 = EDGE_CURVE ( 'NONE', #33799, #13964, #14978, .T. ) ;
#3697 = ORIENTED_EDGE ( 'NONE', *, *, #19548, .F. ) ;
#3698 = EDGE_CURVE ( 'NONE', #20721, #16671, #31190, .T. ) ;
#3699 = ORIENTED_EDGE ( 'NONE', *, *, #29984, .T. ) ;
#3700 = ORIENTED_EDGE ( 'NONE', *, *, #30328, .F. ) ;
#3701 = AXIS2_PLACEMENT_3D ( 'NONE', #6331, #24852, #16879 ) ;
#3702 = CARTESIAN_POINT ( 'NONE',  ( -5.021133111224989953, -1.691831803474588058, -87.50000000000000000 ) ) ;
#3703 = VECTOR ( 'NONE', #5056, 1000.000000000000000 ) ;
#3704 = EDGE_CURVE ( 'NONE', #549, #17916, #30462, .T. ) ;
#3705 = LINE ( 'NONE', #7589, #34756 ) ;
#3706 = FACE_OUTER_BOUND ( 'NONE', #29667, .T. ) ;
#3707 = LINE ( 'NONE', #11740, #27308 ) ;
#3708 = ORIENTED_EDGE ( 'NONE', *, *, #1599, .F. ) ;
#3709 = VECTOR ( 'NONE', #2632, 1000.000000000000000 ) ;
#3710 = CARTESIAN_POINT ( 'NONE',  ( 0.02407890056655781832, 18.59128259035472297, 24.91982945642928016 ) ) ;
#3711 = FACE_OUTER_BOUND ( 'NONE', #5844, .T. ) ;
#3712 = ORIENTED_EDGE ( 'NONE', *, *, #14723, .T. ) ;
#3713 = VECTOR ( 'NONE', #34609, 1000.000000000000114 ) ;
#3714 = CLOSED_SHELL ( 'NONE', ( #22016, #20429, #24539, #11919, #12502, #26875, #2975, #26753, #28834, #30494, #27955, #27899, #23485, #34594, #21993, #30627, #17140, #15035 ) ) ;
#3715 = DIRECTION ( 'NONE',  ( 1.232595164407830946E-32, 3.421138828918010427E-49, -1.000000000000000000 ) ) ;
#3716 = DIRECTION ( 'NONE',  ( 1.000000000000000000, 0.000000000000000000, 0.000000000000000000 ) ) ;
#3717 = ORIENTED_EDGE ( 'NONE', *, *, #34677, .T. ) ;
#3718 = VERTEX_POINT ( 'NONE', #25283 ) ;
#3719 = DIRECTION ( 'NONE',  ( -1.000000000000000000, 0.000000000000000000, 1.232595164407831220E-32 ) ) ;
#3720 = LINE ( 'NONE', #4407, #4675 ) ;
#3721 = EDGE_LOOP ( 'NONE', ( #22976, #9582, #32549, #4228, #33066, #13179, #15785, #9486 ) ) ;
#3722 = CARTESIAN_POINT ( 'NONE',  ( -365.0000000000000000, 114.9999999999999716, 126.0000000000000000 ) ) ;
#3723 = LINE ( 'NONE', #30786, #22860 ) ;
#3724 = DIRECTION ( 'NONE',  ( 0.6473862847818285804, -0.7621620551276356847, 0.000000000000000000 ) ) ;
#3725 = ADVANCED_FACE ( 'NONE', ( #16956 ), #33999, .F. ) ;
#3726 = EDGE_CURVE ( 'NONE', #14044, #25632, #1951, .T. ) ;
#3727 = AXIS2_PLACEMENT_3D ( 'NONE', #11338, #12738, #4349 ) ;
#3728 = B_SPLINE_CURVE_WITH_KNOTS ( 'NONE', 3,
 ( #25457, #1088, #8556, #11956, #19436, #30274 ),
 .UNSPECIFIED., .F., .F.,
 ( 4, 2, 4 ),
 ( 2.073839991540172406E-07, 0.001873405686414694694, 0.003746603988830235401 ),
 .UNSPECIFIED. ) ;
#3729 = CARTESIAN_POINT ( 'NONE',  ( -101.2675397030902928, -3.501388609494501036, 12.00022069954821013 ) ) ;
#3730 = FACE_OUTER_BOUND ( 'NONE', #9143, .T. ) ;
#3731 = VECTOR ( 'NONE', #32637, 1000.000000000000000 ) ;
#3732 = EDGE_CURVE ( 'NONE', #11647, #1683, #27190, .T. ) ;
#3733 = ORIENTED_EDGE ( 'NONE', *, *, #5463, .T. ) ;
#3734 = ADVANCED_FACE ( 'NONE', ( #18532 ), #18349, .T. ) ;
#3735 = ORIENTED_EDGE ( 'NONE', *, *, #7983, .T. ) ;
#3736 = DIRECTION ( 'NONE',  ( 2.631201909438060269E-14, -5.396010391056495992E-16, 0.9999999999999998890 ) ) ;
#3737 = ADVANCED_FACE ( 'NONE', ( #29368 ), #23669, .F. ) ;
#3738 = ORIENTED_EDGE ( 'NONE', *, *, #12637, .T. ) ;
#3739 = VECTOR ( 'NONE', #16799, 1000.000000000000000 ) ;
#3740 = ORIENTED_EDGE ( 'NONE', *, *, #1599, .T. ) ;
#3741 = CARTESIAN_POINT ( 'NONE',  ( 0.000000000000000000, 0.000000000000000000, 13.50000000000000178 ) ) ;
#3742 = CARTESIAN_POINT ( 'NONE',  ( 19.99999999999998934, 4.559999999999908127, 168.2400000000000091 ) ) ;
#3743 = ITEM_DEFINED_TRANSFORMATION ( 'NONE', 'NONE', #1874,  #28566 ) ;
#3744 = ORIENTED_EDGE ( 'NONE', *, *, #17853, .T. ) ;
#3745 = FACE_OUTER_BOUND ( 'NONE', #3935, .T. ) ;
#3746 = VECTOR ( 'NONE', #18434, 1000.000000000000000 ) ;
#3748 = CARTESIAN_POINT ( 'NONE',  ( 2.789999999999999147, 0.000000000000000000, 0.000000000000000000 ) ) ;
#3747 = CARTESIAN_POINT ( 'NONE',  ( 11.62236370382048101, -30.39942490923501950, 68.31122994652405112 ) ) ;
#3749 = ORIENTED_EDGE ( 'NONE', *, *, #34705, .F. ) ;
#3750 = ORIENTED_EDGE ( 'NONE', *, *, #16051, .T. ) ;
#3751 = DIRECTION ( 'NONE',  ( 0.1081190184239419622, -0.9941379571543595972, 0.000000000000000000 ) ) ;
#3752 = AXIS2_PLACEMENT_3D ( 'NONE', #13925, #19628, #2706 ) ;
#3753 = CARTESIAN_POINT ( 'NONE',  ( 2.789999999999999147, 24.25608676733002156, -18.39061402768334119 ) ) ;
#3754 = CARTESIAN_POINT ( 'NONE',  ( 0.000000000000000000, 27.98916443103621177, -15.38717335695007904 ) ) ;
#3755 = DIRECTION ( 'NONE',  ( 0.000000000000000000, 0.000000000000000000, -1.000000000000000000 ) ) ;
#3756 = ORIENTED_EDGE ( 'NONE', *, *, #29048, .T. ) ;
#3757 = DIRECTION ( 'NONE',  ( 0.000000000000000000, 1.000000000000000000, 1.224646799147353207E-16 ) ) ;
#3758 = DIRECTION ( 'NONE',  ( 0.000000000000000000, 0.000000000000000000, 1.000000000000000000 ) ) ;
#3759 =( REPRESENTATION_RELATIONSHIP ('NONE','NONE', #23037, #28231 ) REPRESENTATION_RELATIONSHIP_WITH_TRANSFORMATION ( #6626 )SHAPE_REPRESENTATION_RELATIONSHIP( ) );
#3760 = EDGE_LOOP ( 'NONE', ( #23980, #2746, #26761, #10875 ) ) ;
#3761 = VECTOR ( 'NONE', #27406, 1000.000000000000000 ) ;
#3762 = CARTESIAN_POINT ( 'NONE',  ( 5.021133111224369117, -5.758675521474015291, -67.50000000000000000 ) ) ;
#3763 = CARTESIAN_POINT ( 'NONE',  ( -499.9999999999999432, 136.9999999999999432, 190.9999999999999716 ) ) ;
#3764 = CARTESIAN_POINT ( 'NONE',  ( 0.07098931461607634053, 31.58942871418359744, 2.579295332369118565 ) ) ;
#3765 = ADVANCED_FACE ( 'NONE', ( #26333 ), #7108, .F. ) ;
#3767 = LINE ( 'NONE', #22120, #5990 ) ;
#3766 = CARTESIAN_POINT ( 'NONE',  ( 2.765921099433440666, -8.112136323388726922, -30.01377904834218668 ) ) ;
#3768 = ADVANCED_FACE ( 'NONE', ( #9624 ), #4433, .F. ) ;
#3769 = CARTESIAN_POINT ( 'NONE',  ( -442.0000000000000000, -124.9999999999999716, 132.0000000000000000 ) ) ;
#3770 = LINE ( 'NONE', #17511, #16540 ) ;
#3771 = ORIENTED_EDGE ( 'NONE', *, *, #209, .T. ) ;
#3772 = CARTESIAN_POINT ( 'NONE',  ( -499.9999999999999432, -137.0000000000000000, -187.0000000000000000 ) ) ;
#3773 = PRODUCT_DEFINITION_SHAPE ( 'NONE', 'NONE',  #35132 ) ;
#3774 = CIRCLE ( 'NONE', #26508, 4.309328216469825001 ) ;
#3775 = EDGE_LOOP ( 'NONE', ( #3699, #28391 ) ) ;
#3776 =( LENGTH_UNIT ( ) NAMED_UNIT ( * ) SI_UNIT ( .MILLI., .METRE. ) );
#3777 = VECTOR ( 'NONE', #3621, 1000.000000000000000 ) ;
#3778 = ORIENTED_EDGE ( 'NONE', *, *, #3839, .T. ) ;
#3779 = VERTEX_POINT ( 'NONE', #26154 ) ;
#3780 = FACE_OUTER_BOUND ( 'NONE', #21252, .T. ) ;
#3781 = ORIENTED_EDGE ( 'NONE', *, *, #28415, .F. ) ;
#3782 = EDGE_LOOP ( 'NONE', ( #23329, #34940, #22038, #30078 ) ) ;
#3783 = FACE_OUTER_BOUND ( 'NONE', #33989, .T. ) ;
#3784 = VERTEX_POINT ( 'NONE', #20826 ) ;
#3785 = DIRECTION ( 'NONE',  ( -0.000000000000000000, 0.000000000000000000, 1.000000000000000000 ) ) ;
#3786 = PLANE ( 'NONE',  #22840 ) ;
#3787 = ORIENTED_EDGE ( 'NONE', *, *, #4872, .F. ) ;
#3788 = ORIENTED_EDGE ( 'NONE', *, *, #14682, .F. ) ;
#3789 = DIRECTION ( 'NONE',  ( 1.000000000000000000, 0.000000000000000000, 0.000000000000000000 ) ) ;
#3790 = FACE_OUTER_BOUND ( 'NONE', #5666, .T. ) ;
#3791 = CARTESIAN_POINT ( 'NONE',  ( 0.006871051096725699914, -29.45617853245860118, -9.233693611950151592 ) ) ;
#3792 = CARTESIAN_POINT ( 'NONE',  ( -12.00000000000001066, -137.0000000000000000, -155.0000000000000284 ) ) ;
#3793 = FACE_OUTER_BOUND ( 'NONE', #613, .T. ) ;
#3794 = ORIENTED_EDGE ( 'NONE', *, *, #4288, .F. ) ;
#3795 = TOROIDAL_SURFACE ( 'NONE', #27678, 15.69999999999999929, 0.3000000000000007661 ) ;
#3796 = DIRECTION ( 'NONE',  ( 0.000000000000000000, 0.000000000000000000, 1.000000000000000000 ) ) ;
#3797 = CARTESIAN_POINT ( 'NONE',  ( -361.0000000000000000, 124.9999999999999432, 168.9999999999999716 ) ) ;
#3798 = EDGE_LOOP ( 'NONE', ( #3814, #27015, #28184, #20013 ) ) ;
#3799 = CARTESIAN_POINT ( 'NONE',  ( 0.5355294694855760040, 14.31130214556277735, 2.212097561415798719 ) ) ;
#3800 = CARTESIAN_POINT ( 'NONE',  ( -19.99999999999998934, -134.9999999999999716, 187.0000000000000000 ) ) ;
#3801 = ADVANCED_FACE ( 'NONE', ( #25811 ), #12308, .T. ) ;
#3802 = DIRECTION ( 'NONE',  ( 1.000000000000000000, -0.000000000000000000, -0.000000000000000000 ) ) ;
#3803 = CARTESIAN_POINT ( 'NONE',  ( -442.0000000000000000, -105.0000000000000142, -105.9999999999999574 ) ) ;
#3804 = LINE ( 'NONE', #31730, #14481 ) ;
#3805 = EDGE_CURVE ( 'NONE', #5316, #12202, #4264, .T. ) ;
#3806 = DIRECTION ( 'NONE',  ( 0.000000000000000000, 0.000000000000000000, 1.000000000000000000 ) ) ;
#3807 = ORIENTED_EDGE ( 'NONE', *, *, #30479, .F. ) ;
#3808 = ADVANCED_FACE ( 'NONE', ( #12478 ), #23489, .T. ) ;
#3809 = DIRECTION ( 'NONE',  ( 1.000000000000000000, 0.000000000000000000, 0.000000000000000000 ) ) ;
#3811 = DIRECTION ( 'NONE',  ( -1.000000000000000000, 0.000000000000000000, -0.000000000000000000 ) ) ;
#3810 = CYLINDRICAL_SURFACE ( 'NONE', #22806, 2.033421858999711951 ) ;
#3812 = ORIENTED_EDGE ( 'NONE', *, *, #482, .T. ) ;
#3813 = LINE ( 'NONE', #18895, #17158 ) ;
#3814 = ORIENTED_EDGE ( 'NONE', *, *, #7486, .T. ) ;
#3815 = CIRCLE ( 'NONE', #23724, 4.750000000000004441 ) ;
#3816 = CIRCLE ( 'NONE', #4954, 3.999999999999976019 ) ;
#3817 = ORIENTED_EDGE ( 'NONE', *, *, #31883, .F. ) ;
#3818 = CARTESIAN_POINT ( 'NONE',  ( 104.0188950037896660, -5.656875047978680904, -4.924762495648698390 ) ) ;
#3819 = ORIENTED_EDGE ( 'NONE', *, *, #15759, .F. ) ;
#3820 = ORIENTED_EDGE ( 'NONE', *, *, #5576, .T. ) ;
#3821 = CARTESIAN_POINT ( 'NONE',  ( -349.0000000000000000, -125.0000000000000284, 181.0000000000000000 ) ) ;
#3823 = DIRECTION ( 'NONE',  ( 0.000000000000000000, 1.000000000000000000, 0.000000000000000000 ) ) ;
#3822 = CIRCLE ( 'NONE', #997, 2.033421858999711951 ) ;
#3824 = CARTESIAN_POINT ( 'NONE',  ( -9.978866888775426602, 14.09580098603202458, -67.50000000000000000 ) ) ;
#3825 = FACE_OUTER_BOUND ( 'NONE', #4403, .T. ) ;
#3826 = ORIENTED_EDGE ( 'NONE', *, *, #121, .F. ) ;
#3827 = ORIENTED_EDGE ( 'NONE', *, *, #20467, .T. ) ;
#3828 = LINE ( 'NONE', #9878, #4854 ) ;
#3829 = FACE_OUTER_BOUND ( 'NONE', #21839, .T. ) ;
#3830 = DIRECTION ( 'NONE',  ( -1.000000000000000000, 0.000000000000000000, -0.000000000000000000 ) ) ;
#3831 = LINE ( 'NONE', #33743, #30069 ) ;
#3832 = CARTESIAN_POINT ( 'NONE',  ( -418.0000000000000000, -105.0000000000000142, 162.9999999999999716 ) ) ;
#3833 = CARTESIAN_POINT ( 'NONE',  ( -6.500000000000000000, 0.000000000000000000, 0.000000000000000000 ) ) ;
#3834 = CIRCLE ( 'NONE', #33395, 4.309328216469825001 ) ;
#3835 = CARTESIAN_POINT ( 'NONE',  ( -70.00000000000000000, 75.55999999999990280, 168.2400000000000091 ) ) ;
#3836 = VERTEX_POINT ( 'NONE', #9792 ) ;
#3837 = CARTESIAN_POINT ( 'NONE',  ( 15.99999999999997868, 136.9999999999999716, -155.0000000000000000 ) ) ;
#3838 = DIRECTION ( 'NONE',  ( -0.7960930657056428661, 0.6051742151937663516, 0.000000000000000000 ) ) ;
#3839 = EDGE_CURVE ( 'NONE', #33582, #693, #18890, .T. ) ;
#3840 = DIRECTION ( 'NONE',  ( 0.000000000000000000, 1.836970198721029441E-16, -1.000000000000000000 ) ) ;
#3841 = ORIENTED_EDGE ( 'NONE', *, *, #34221, .F. ) ;
#3842 = AXIS2_PLACEMENT_3D ( 'NONE', #32775, #27614, #14104 ) ;
#3843 = AXIS2_PLACEMENT_3D ( 'NONE', #15336, #2307, #2143 ) ;
#3844 = DIRECTION ( 'NONE',  ( -1.000000000000000000, -0.000000000000000000, -0.000000000000000000 ) ) ;
#3845 = ORIENTED_EDGE ( 'NONE', *, *, #21690, .F. ) ;
#3846 = EDGE_CURVE ( 'NONE', #21178, #21158, #17569, .T. ) ;
#3847 = DIRECTION ( 'NONE',  ( 0.000000000000000000, 0.000000000000000000, 1.000000000000000000 ) ) ;
#3848 = CARTESIAN_POINT ( 'NONE',  ( -102.4305550605362214, 4.435438170924840939, 11.68828588916098887 ) ) ;
#3849 = EDGE_CURVE ( 'NONE', #23988, #5983, #18007, .T. ) ;
#3850 = CIRCLE ( 'NONE', #32837, 12.50000000000000000 ) ;
#3851 = ORIENTED_EDGE ( 'NONE', *, *, #16696, .T. ) ;
#3852 = ADVANCED_FACE ( 'NONE', ( #1774 ), #18178, .F. ) ;
#3853 = EDGE_CURVE ( 'NONE', #12566, #3150, #14744, .T. ) ;
#3854 = FACE_OUTER_BOUND ( 'NONE', #17500, .T. ) ;
#3855 = DIRECTION ( 'NONE',  ( 0.000000000000000000, 0.000000000000000000, -1.000000000000000000 ) ) ;
#3856 = CARTESIAN_POINT ( 'NONE',  ( 2.789999999999999147, -25.77598557799260703, 16.24962337825793313 ) ) ;
#3857 = EDGE_CURVE ( 'NONE', #10848, #29430, #653, .T. ) ;
#3858 = ORIENTED_EDGE ( 'NONE', *, *, #3032, .F. ) ;
#3859 = CIRCLE ( 'NONE', #23186, 32.54542015209056416 ) ;
#3860 = CARTESIAN_POINT ( 'NONE',  ( 785.7374708698217773, 1068.305460764686131, 1753.598338701303192 ) ) ;
#3861 = DIRECTION ( 'NONE',  ( 1.000000000000000000, 0.000000000000000000, 0.000000000000000000 ) ) ;
#3862 = ORIENTED_EDGE ( 'NONE', *, *, #13178, .T. ) ;
#3863 = DIRECTION ( 'NONE',  ( 0.3701381553399133995, -0.9289767198167917517, -0.000000000000000000 ) ) ;
#3864 = CARTESIAN_POINT ( 'NONE',  ( -12.00000000000003908, -134.9999999999999716, -186.9999999999999716 ) ) ;
#3865 = CARTESIAN_POINT ( 'NONE',  ( 8.000000000000000000, 0.000000000000000000, 0.000000000000000000 ) ) ;
#3866 = LINE ( 'NONE', #14758, #22204 ) ;
#3867 = ORIENTED_EDGE ( 'NONE', *, *, #34646, .T. ) ;
#3868 = ORIENTED_EDGE ( 'NONE', *, *, #28445, .F. ) ;
#3869 = CIRCLE ( 'NONE', #9585, 7.999999999999979572 ) ;
#3870 = VERTEX_POINT ( 'NONE', #16207 ) ;
#3871 = CARTESIAN_POINT ( 'NONE',  ( -349.0000000000000000, -135.0000000000000000, 111.9999999999999858 ) ) ;
#3872 = CARTESIAN_POINT ( 'NONE',  ( 2.789999999999999147, -5.984944020945660803, -28.84917528048448787 ) ) ;
#3873 = AXIS2_PLACEMENT_3D ( 'NONE', #5358, #13399, #18913 ) ;
#3874 = CARTESIAN_POINT ( 'NONE',  ( 11.99999999999999645, 144.9999999999999716, -175.0000000000000284 ) ) ;
#3875 = DIRECTION ( 'NONE',  ( 0.000000000000000000, -0.000000000000000000, 1.000000000000000000 ) ) ;
#3876 = ORIENTED_EDGE ( 'NONE', *, *, #6661, .T. ) ;
#3877 = CARTESIAN_POINT ( 'NONE',  ( 2.719010698802078796, -31.01706505092339228, 6.518161977769513449 ) ) ;
#3878 = CARTESIAN_POINT ( 'NONE',  ( -430.0000000000000000, -119.0000000000000000, 113.9999999999999858 ) ) ;
#3879 = EDGE_LOOP ( 'NONE', ( #30099, #2641, #11280, #34208 ) ) ;
#3880 = DIRECTION ( 'NONE',  ( 0.000000000000000000, 0.000000000000000000, -1.000000000000000000 ) ) ;
#3881 = CARTESIAN_POINT ( 'NONE',  ( 105.7609509841301190, 5.700015625666662089, 11.12505441474362655 ) ) ;
#3882 = AXIS2_PLACEMENT_3D ( 'NONE', #16215, #174, #11029 ) ;
#3883 = VERTEX_POINT ( 'NONE', #27041 ) ;
#3884 = SURFACE_STYLE_FILL_AREA ( #24723 ) ;
#3885 = AXIS2_PLACEMENT_3D ( 'NONE', #5525, #13565, #24398 ) ;
#3886 = CARTESIAN_POINT ( 'NONE',  ( 10.17231796313411429, 15.60017778382161424, -87.50000000000000000 ) ) ;
#3887 = ORIENTED_EDGE ( 'NONE', *, *, #3909, .T. ) ;
#3888 = CARTESIAN_POINT ( 'NONE',  ( 0.000000000000000000, -0.09145294252657359957, -30.47036804522409525 ) ) ;
#3889 = DIRECTION ( 'NONE',  ( -0.000000000000000000, -1.836970198721029688E-16, 1.000000000000000000 ) ) ;
#3890 = DIRECTION ( 'NONE',  ( -8.673617379884057166E-16, 0.000000000000000000, -1.000000000000000000 ) ) ;
#3891 = TOROIDAL_SURFACE ( 'NONE', #34624, 13.00000000000000000, 1.799999999999999822 ) ;
#3892 = ADVANCED_FACE ( 'NONE', ( #18700 ), #34052, .T. ) ;
#3893 = EDGE_CURVE ( 'NONE', #22752, #25215, #8164, .T. ) ;
#3894 = CARTESIAN_POINT ( 'NONE',  ( -109.6555751755425376, -2.125365432952319278, 12.31898464336051902 ) ) ;
#3895 = UNCERTAINTY_MEASURE_WITH_UNIT (LENGTH_MEASURE( 1.000000000000000082E-05 ), #25844, 'distance_accuracy_value', 'NONE');
#3896 = DIRECTION ( 'NONE',  ( -1.000000000000000000, 0.000000000000000000, 0.000000000000000000 ) ) ;
#3897 = PRESENTATION_STYLE_ASSIGNMENT (( #9774 ) ) ;
#3898 = ORIENTED_EDGE ( 'NONE', *, *, #28327, .F. ) ;
#3899 = VECTOR ( 'NONE', #5620, 1000.000000000000000 ) ;
#3900 = VERTEX_POINT ( 'NONE', #10682 ) ;
#3901 = DIRECTION ( 'NONE',  ( 2.152398694032528628E-14, -2.141878230451567343E-14, 0.9999999999999998890 ) ) ;
#3902 = ORIENTED_EDGE ( 'NONE', *, *, #4188, .F. ) ;
#3903 = EDGE_CURVE ( 'NONE', #26143, #25412, #25513, .T. ) ;
#3904 = CARTESIAN_POINT ( 'NONE',  ( -365.0000000000000000, 118.9999999999999716, 109.9999999999999858 ) ) ;
#3905 = FACE_OUTER_BOUND ( 'NONE', #14944, .T. ) ;
#3906 = ORIENTED_EDGE ( 'NONE', *, *, #9824, .T. ) ;
#3907 = DIRECTION ( 'NONE',  ( -0.000000000000000000, -0.000000000000000000, -1.000000000000000000 ) ) ;
#3908 = CARTESIAN_POINT ( 'NONE',  ( -108.8452008526440551, -3.377194313163045969, -12.03587146382073669 ) ) ;
#3909 = EDGE_CURVE ( 'NONE', #23491, #25411, #18156, .T. ) ;
#3910 = EDGE_CURVE ( 'NONE', #26361, #34601, #2534, .T. ) ;
#3911 = TOROIDAL_SURFACE ( 'NONE', #29521, 10.30000000000000071, 0.3000000000000025424 ) ;
#3912 = EDGE_CURVE ( 'NONE', #32615, #1165, #9030, .T. ) ;
#3914 = DIRECTION ( 'NONE',  ( -1.000000000000000000, 0.000000000000000000, 0.000000000000000000 ) ) ;
#3913 = DIRECTION ( 'NONE',  ( 1.000000000000000000, 0.000000000000000000, 5.546364386991661285E-52 ) ) ;
#3915 = ORIENTED_EDGE ( 'NONE', *, *, #22996, .T. ) ;
#3916 = ORIENTED_EDGE ( 'NONE', *, *, #7351, .T. ) ;
#3917 = CARTESIAN_POINT ( 'NONE',  ( 2.789999999999999147, 23.28319895603611300, -21.86437915510192909 ) ) ;
#3918 = EDGE_CURVE ( 'NONE', #23287, #15452, #10847, .T. ) ;
#3919 = CARTESIAN_POINT ( 'NONE',  ( -430.0000000000000000, 118.9999999999999716, 130.0000000000000000 ) ) ;
#3920 = CYLINDRICAL_SURFACE ( 'NONE', #10879, 2.036051781435508801 ) ;
#3921 = ORIENTED_EDGE ( 'NONE', *, *, #18983, .F. ) ;
#3922 = VECTOR ( 'NONE', #4359, 1000.000000000000000 ) ;
#3923 = CARTESIAN_POINT ( 'NONE',  ( -499.9999999999999432, 136.9999999999999432, -187.0000000000000000 ) ) ;
#3924 = CARTESIAN_POINT ( 'NONE',  ( 0.000000000000000000, 11.69134295108991495, 6.750000000000012434 ) ) ;
#3925 = VERTEX_POINT ( 'NONE', #13524 ) ;
#3926 = DIRECTION ( 'NONE',  ( -2.736911063134582149E-48, 7.888609052210118054E-31, 1.000000000000000000 ) ) ;
#3927 = FACE_OUTER_BOUND ( 'NONE', #5183, .T. ) ;
#3928 = CARTESIAN_POINT ( 'NONE',  ( -143.0000000000000568, -97.49999999999998579, 51.88904920397793319 ) ) ;
#3930 = DIRECTION ( 'NONE',  ( -1.000000000000000000, 0.000000000000000000, 0.000000000000000000 ) ) ;
#3929 = CARTESIAN_POINT ( 'NONE',  ( -445.9999999999999432, -105.0000000000000142, 162.9999999999999716 ) ) ;
#3931 = AXIS2_PLACEMENT_3D ( 'NONE', #31931, #24093, #7546 ) ;
#3932 = EDGE_CURVE ( 'NONE', #23023, #15358, #2765, .T. ) ;
#3933 = DIRECTION ( 'NONE',  ( 0.000000000000000000, 1.000000000000000000, 5.053935297177146739E-49 ) ) ;
#3934 = CARTESIAN_POINT ( 'NONE',  ( -5.021133111224989953, -5.758675521474012626, -87.50000000000000000 ) ) ;
#3935 = EDGE_LOOP ( 'NONE', ( #5498, #20270, #10714, #11543 ) ) ;
#3936 = CYLINDRICAL_SURFACE ( 'NONE', #13907, 7.999999999999979572 ) ;
#3937 = DIRECTION ( 'NONE',  ( 0.000000000000000000, 0.000000000000000000, -1.000000000000000000 ) ) ;
#3938 = VECTOR ( 'NONE', #10720, 1000.000000000000000 ) ;
#3939 = ORIENTED_EDGE ( 'NONE', *, *, #9917, .T. ) ;
#3940 = ORIENTED_EDGE ( 'NONE', *, *, #28690, .F. ) ;
#3941 = ORIENTED_EDGE ( 'NONE', *, *, #5755, .F. ) ;
#3942 = CARTESIAN_POINT ( 'NONE',  ( -32.54223829851967764, 0.4550817492056100644, 68.31122994652405112 ) ) ;
#3943 = EDGE_LOOP ( 'NONE', ( #16572, #34885, #28217, #16509, #8418, #26069 ) ) ;
#3944 = ORIENTED_EDGE ( 'NONE', *, *, #30322, .F. ) ;
#3945 = EDGE_LOOP ( 'NONE', ( #13217, #1920, #12817, #16106 ) ) ;
#3946 = EDGE_CURVE ( 'NONE', #14788, #10055, #12454, .T. ) ;
#3947 = DIRECTION ( 'NONE',  ( 0.000000000000000000, 0.000000000000000000, -1.000000000000000000 ) ) ;
#3948 = EDGE_CURVE ( 'NONE', #21689, #3592, #32313, .T. ) ;
#3949 = ITEM_DEFINED_TRANSFORMATION ( 'NONE', 'NONE', #16689,  #28566 ) ;
#3950 = EDGE_CURVE ( 'NONE', #25284, #21475, #26063, .T. ) ;
#3951 = ORIENTED_EDGE ( 'NONE', *, *, #4235, .F. ) ;
#3952 = CARTESIAN_POINT ( 'NONE',  ( 0.000000000000000000, -11.13185981125856294, -28.36429779836965182 ) ) ;
#3953 = PLANE ( 'NONE',  #26798 ) ;
#3954 = ORIENTED_EDGE ( 'NONE', *, *, #6812, .F. ) ;
#3955 = ORIENTED_EDGE ( 'NONE', *, *, #12742, .F. ) ;
#3956 =( REPRESENTATION_RELATIONSHIP ('NONE','NONE', #23037, #15767 ) REPRESENTATION_RELATIONSHIP_WITH_TRANSFORMATION ( #32366 )SHAPE_REPRESENTATION_RELATIONSHIP( ) );
#3957 = CARTESIAN_POINT ( 'NONE',  ( -32.37866696771086339, 3.290334066652099043, -36.68877005347593467 ) ) ;
#3958 = FACE_OUTER_BOUND ( 'NONE', #9532, .T. ) ;
#3959 = DIRECTION ( 'NONE',  ( 1.000000000000000000, 0.000000000000000000, -1.848892746611746966E-32 ) ) ;
#3960 = LINE ( 'NONE', #9502, #32993 ) ;
#3961 = DIRECTION ( 'NONE',  ( -1.000000000000000000, 0.000000000000000000, 0.000000000000000000 ) ) ;
#3962 = ORIENTED_EDGE ( 'NONE', *, *, #25842, .T. ) ;
#3963 = CARTESIAN_POINT ( 'NONE',  ( -442.0000000000000000, -125.0000000000000000, -109.9999999999999574 ) ) ;
#3964 = LINE ( 'NONE', #6280, #15132 ) ;
#3965 = DIRECTION ( 'NONE',  ( 0.000000000000000000, 0.000000000000000000, -1.000000000000000000 ) ) ;
#3966 = EDGE_LOOP ( 'NONE', ( #9619, #10632, #14603, #27494 ) ) ;
#3967 = B_SPLINE_CURVE_WITH_KNOTS ( 'NONE', 3,
 ( #15599, #31136, #26609, #5061, #26435, #1231 ),
 .UNSPECIFIED., .F., .F.,
 ( 4, 2, 4 ),
 ( 2.699892340800535851E-07, 0.001873468359918846558, 0.003746666730603612824 ),
 .UNSPECIFIED. ) ;
#3968 = LINE ( 'NONE', #12364, #30439 ) ;
#3969 = LINE ( 'NONE', #14155, #34822 ) ;
#3970 = CARTESIAN_POINT ( 'NONE',  ( -500.0000000000000000, -109.0000000000000142, 187.0000000000000000 ) ) ;
#3971 = VECTOR ( 'NONE', #30981, 1000.000000000000000 ) ;
#3972 = DIRECTION ( 'NONE',  ( -0.000000000000000000, -0.000000000000000000, -1.000000000000000000 ) ) ;
#3974 = FACE_OUTER_BOUND ( 'NONE', #16629, .T. ) ;
#3973 = DIRECTION ( 'NONE',  ( -1.000000000000000000, 0.000000000000000000, 0.000000000000000000 ) ) ;
#3975 = CARTESIAN_POINT ( 'NONE',  ( 2.719051662671754244, -0.5905164915259186742, 31.68852467239034709 ) ) ;
#3976 = ORIENTED_EDGE ( 'NONE', *, *, #17509, .F. ) ;
#3977 = CARTESIAN_POINT ( 'NONE',  ( 2.789999999999999147, 29.44518845714779332, -9.980709654879110104 ) ) ;
#3979 = DIRECTION ( 'NONE',  ( 0.000000000000000000, 0.000000000000000000, -1.000000000000000000 ) ) ;
#3978 = CYLINDRICAL_SURFACE ( 'NONE', #16082, 2.524999999999999467 ) ;
#3980 = ORIENTED_EDGE ( 'NONE', *, *, #32786, .F. ) ;
#3981 = DIRECTION ( 'NONE',  ( -1.000000000000000000, -0.000000000000000000, -0.000000000000000000 ) ) ;
#3982 = EDGE_CURVE ( 'NONE', #28753, #32553, #7816, .T. ) ;
#3983 = VERTEX_POINT ( 'NONE', #26861 ) ;
#3984 = EDGE_LOOP ( 'NONE', ( #5832, #24451, #13414, #26486 ) ) ;
#3985 = CARTESIAN_POINT ( 'NONE',  ( 105.9791845165408546, -5.657186516187210579, -4.924400946180165661 ) ) ;
#3986 = ORIENTED_EDGE ( 'NONE', *, *, #14193, .T. ) ;
#3987 = ORIENTED_EDGE ( 'NONE', *, *, #33054, .F. ) ;
#3988 = LINE ( 'NONE', #23396, #20731 ) ;
#3989 = EDGE_CURVE ( 'NONE', #3035, #2043, #33392, .T. ) ;
#3990 = CIRCLE ( 'NONE', #21637, 1.799999999999999600 ) ;
#3991 = LINE ( 'NONE', #25902, #4493 ) ;
#3992 = EDGE_CURVE ( 'NONE', #35091, #6717, #2211, .T. ) ;
#3993 = EDGE_CURVE ( 'NONE', #32063, #26390, #6167, .T. ) ;
#3994 = DIRECTION ( 'NONE',  ( -1.000000000000000000, 0.000000000000000000, 0.000000000000000000 ) ) ;
#3995 = CARTESIAN_POINT ( 'NONE',  ( 0.5248942691478599709, 33.01038087096675611, -4.952322205614974493 ) ) ;
#3996 = EDGE_LOOP ( 'NONE', ( #3117, #19286, #33918, #24462 ) ) ;
#3997 = VERTEX_POINT ( 'NONE', #33215 ) ;
#3998 = CARTESIAN_POINT ( 'NONE',  ( -5.491809612354312975, 32.07872192057773475, 68.31122994652405112 ) ) ;
#3999 = CARTESIAN_POINT ( 'NONE',  ( 30.98406361983693103, 9.959526819984921175, 68.31122994652405112 ) ) ;
#4000 = EDGE_CURVE ( 'NONE', #14760, #32651, #14371, .T. ) ;
#4001 = DIRECTION ( 'NONE',  ( 0.000000000000000000, -1.000000000000000000, -1.836970198721029934E-16 ) ) ;
#4002 = CARTESIAN_POINT ( 'NONE',  ( -418.0000000000000000, -105.0000000000000142, -77.99999999999997158 ) ) ;
#4003 = DIRECTION ( 'NONE',  ( -1.000000000000000000, 0.000000000000000000, 0.000000000000000000 ) ) ;
#4004 = FACE_OUTER_BOUND ( 'NONE', #29965, .T. ) ;
#4005 = AXIS2_PLACEMENT_3D ( 'NONE', #8397, #16430, #22457 ) ;
#4006 = CARTESIAN_POINT ( 'NONE',  ( -442.0000000000000000, 105.0000000000000142, 104.0000000000000142 ) ) ;
#4007 = ORIENTED_EDGE ( 'NONE', *, *, #15393, .T. ) ;
#4008 = CIRCLE ( 'NONE', #57, 1.154999999999999805 ) ;
#4009 = CARTESIAN_POINT ( 'NONE',  ( -25.07182831876307105, -28.36910952062234870, 68.31122994652405112 ) ) ;
#4010 = CARTESIAN_POINT ( 'NONE',  ( 2.789999999999999147, -11.13185981125896795, 28.36429779836946352 ) ) ;
#4011 = DIRECTION ( 'NONE',  ( 0.000000000000000000, -5.053935297177146739E-49, -1.000000000000000000 ) ) ;
#4012 = EDGE_LOOP ( 'NONE', ( #17001, #28215, #12911, #33865 ) ) ;
#4013 = CARTESIAN_POINT ( 'NONE',  ( -349.0000000000000000, -125.0000000000000284, 168.9999999999999716 ) ) ;
#4014 = VERTEX_POINT ( 'NONE', #14549 ) ;
#4015 = CIRCLE ( 'NONE', #22786, 2.525000000000000799 ) ;
#4016 = DIRECTION ( 'NONE',  ( 0.000000000000000000, -1.000000000000000000, -1.836970198721029688E-16 ) ) ;
#4017 = FACE_BOUND ( 'NONE', #34001, .T. ) ;
#4018 = AXIS2_PLACEMENT_3D ( 'NONE', #34084, #31922, #2213 ) ;
#4019 = ORIENTED_EDGE ( 'NONE', *, *, #10405, .F. ) ;
#4020 = DIRECTION ( 'NONE',  ( 0.000000000000000000, 0.000000000000000000, 1.000000000000000000 ) ) ;
#4021 = CARTESIAN_POINT ( 'NONE',  ( 105.0000000000000000, 0.000000000000000000, 57.49999999999999289 ) ) ;
#4022 = EDGE_LOOP ( 'NONE', ( #17268, #15743, #11741, #8505 ) ) ;
#4023 = AXIS2_PLACEMENT_3D ( 'NONE', #5496, #30242, #24893 ) ;
#4024 = CARTESIAN_POINT ( 'NONE',  ( 788.5036372753030491, 1042.453041398084679, 1753.598338701303419 ) ) ;
#4025 = VECTOR ( 'NONE', #7127, 1000.000000000000000 ) ;
#4026 = ADVANCED_FACE ( 'NONE', ( #12053 ), #25376, .T. ) ;
#4027 = CARTESIAN_POINT ( 'NONE',  ( 2.789999999999999147, -25.83993731729781729, -16.24881338200996694 ) ) ;
#4028 = ORIENTED_EDGE ( 'NONE', *, *, #22404, .T. ) ;
#4029 = CARTESIAN_POINT ( 'NONE',  ( -442.0000000000000000, 105.0000000000000142, -105.9999999999999574 ) ) ;
#4030 = EDGE_CURVE ( 'NONE', #26496, #1125, #12563, .T. ) ;
#4031 = LINE ( 'NONE', #24305, #19265 ) ;
#4032 = FACE_OUTER_BOUND ( 'NONE', #7499, .T. ) ;
#4033 = FACE_OUTER_BOUND ( 'NONE', #29172, .T. ) ;
#4034 = EDGE_LOOP ( 'NONE', ( #29464, #29518, #34962, #1124, #31204, #11890, #26411, #30818, #32095, #20216, #1648, #14061 ) ) ;
#4035 = ORIENTED_EDGE ( 'NONE', *, *, #33177, .T. ) ;
#4036 = ORIENTED_EDGE ( 'NONE', *, *, #2377, .F. ) ;
#4037 = VECTOR ( 'NONE', #15730, 1000.000000000000000 ) ;
#4038 = EDGE_CURVE ( 'NONE', #32731, #5950, #1177, .T. ) ;
#4039 = LINE ( 'NONE', #21654, #4959 ) ;
#4041 = AXIS2_PLACEMENT_3D ( 'NONE', #23533, #1304, #18214 ) ;
#4040 = CARTESIAN_POINT ( 'NONE',  ( -6.500000000000000000, 0.000000000000000000, 5.429999999999999716 ) ) ;
#4042 = CARTESIAN_POINT ( 'NONE',  ( 37.71145559917817280, 3.353962854566119756, 68.31122994652405112 ) ) ;
#4043 = DIRECTION ( 'NONE',  ( -0.000000000000000000, -0.000000000000000000, 1.000000000000000000 ) ) ;
#4044 = EDGE_CURVE ( 'NONE', #31622, #9953, #27215, .T. ) ;
#4045 = CARTESIAN_POINT ( 'NONE',  ( 27.99209646187092559, 25.49206711720156093, 68.31122994652405112 ) ) ;
#4046 = DIRECTION ( 'NONE',  ( 1.000000000000000000, 0.000000000000000000, 5.546364386991661285E-52 ) ) ;
#4047 = VERTEX_POINT ( 'NONE', #1008 ) ;
#4048 = PRODUCT_DEFINITION_SHAPE ( 'NONE', 'NONE',  #35136 ) ;
#4049 = EDGE_CURVE ( 'NONE', #30605, #28861, #33464, .T. ) ;
#4050 = CARTESIAN_POINT ( 'NONE',  ( 109.9700946220824278, 2.891935069322400853, 12.16509469334829774 ) ) ;
#4051 = EDGE_CURVE ( 'NONE', #527, #5845, #21767, .T. ) ;
#4052 = ORIENTED_EDGE ( 'NONE', *, *, #24210, .T. ) ;
#4053 = CARTESIAN_POINT ( 'NONE',  ( -11.83261234297099662, -30.31820670846267873, 68.31122994652405112 ) ) ;
#4054 = VECTOR ( 'NONE', #1058, 1000.000000000000000 ) ;
#4055 = AXIS2_PLACEMENT_3D ( 'NONE', #24335, #10829, #18681 ) ;
#4057 = VECTOR ( 'NONE', #1378, 1000.000000000000000 ) ;
#4056 = DIRECTION ( 'NONE',  ( -1.000000000000000000, 0.000000000000000000, 0.000000000000000000 ) ) ;
#4058 = ORIENTED_EDGE ( 'NONE', *, *, #2636, .F. ) ;
#4059 = AXIS2_PLACEMENT_3D ( 'NONE', #34539, #31851, #1450 ) ;
#4060 = DIRECTION ( 'NONE',  ( -1.000000000000000000, 0.000000000000000000, 0.000000000000000000 ) ) ;
#4061 = FACE_OUTER_BOUND ( 'NONE', #34468, .T. ) ;
#4062 = CARTESIAN_POINT ( 'NONE',  ( -12.00000000000001243, 134.9999999999998863, 194.9999999999999716 ) ) ;
#4063 = CARTESIAN_POINT ( 'NONE',  ( -104.6638623058952078, -5.115085776248456284, 11.40552048381710115 ) ) ;
#4064 = PLANE ( 'NONE',  #33823 ) ;
#4065 = DIRECTION ( 'NONE',  ( 0.000000000000000000, 1.131431318426415506E-52, 1.000000000000000000 ) ) ;
#4066 = ORIENTED_EDGE ( 'NONE', *, *, #21663, .F. ) ;
#4067 = AXIS2_PLACEMENT_3D ( 'NONE', #17048, #33924, #17578 ) ;
#4068 = ORIENTED_EDGE ( 'NONE', *, *, #2083, .F. ) ;
#4069 = DIRECTION ( 'NONE',  ( -7.893605728314050488E-14, 1.618803117314786135E-15, 0.9999999999999998890 ) ) ;
#4070 = ORIENTED_EDGE ( 'NONE', *, *, #16062, .T. ) ;
#4071=STYLED_ITEM('',(#35254),#34697);
#4072 = CARTESIAN_POINT ( 'NONE',  ( 2.789999999999999147, -29.00730259674831757, -9.328884633909261481 ) ) ;
#4073 = CIRCLE ( 'NONE', #6902, 7.500000000000000000 ) ;
#4074 = DIRECTION ( 'NONE',  ( 0.000000000000000000, 0.000000000000000000, 1.000000000000000000 ) ) ;
#4075 = CONTEXT_DEPENDENT_SHAPE_REPRESENTATION ( #25533, #25413 ) ;
#4076 = ORIENTED_EDGE ( 'NONE', *, *, #19368, .T. ) ;
#4077=STYLED_ITEM('',(#35254),#22940);
#4078 = FACE_OUTER_BOUND ( 'NONE', #8648, .T. ) ;
#4079 = PRESENTATION_STYLE_ASSIGNMENT (( #16954 ) ) ;
#4080 = EDGE_CURVE ( 'NONE', #4999, #28476, #4180, .T. ) ;
#4082 = LINE ( 'NONE', #22800, #25487 ) ;
#4081 = DIRECTION ( 'NONE',  ( 0.000000000000000000, 0.000000000000000000, 1.000000000000000000 ) ) ;
#4083 = ORIENTED_EDGE ( 'NONE', *, *, #5194, .T. ) ;
#4084 = ORIENTED_EDGE ( 'NONE', *, *, #2562, .F. ) ;
#4085 = EDGE_CURVE ( 'NONE', #31849, #24798, #25731, .T. ) ;
#4086 = EDGE_CURVE ( 'NONE', #18640, #26094, #6324, .T. ) ;
#4087 = LINE ( 'NONE', #31506, #28226 ) ;
#4088 = CARTESIAN_POINT ( 'NONE',  ( -15.99999999999998579, 112.9999999999999574, 155.0000000000000000 ) ) ;
#4089 = DIRECTION ( 'NONE',  ( -0.000000000000000000, -0.000000000000000000, -1.000000000000000000 ) ) ;
#4090 = ORIENTED_EDGE ( 'NONE', *, *, #26835, .T. ) ;
#4091 = FACE_OUTER_BOUND ( 'NONE', #26156, .T. ) ;
#4092 = PRODUCT_DEFINITION_SHAPE ( 'NONE', 'NONE',  #35109 ) ;
#4093 = ORIENTED_EDGE ( 'NONE', *, *, #19106, .F. ) ;
#4094 = CARTESIAN_POINT ( 'NONE',  ( 11.99999999999999645, -55.00000000000002132, 162.9999999999999716 ) ) ;
#4095 = LINE ( 'NONE', #575, #30784 ) ;
#4096 = EDGE_CURVE ( 'NONE', #25358, #9066, #28584, .T. ) ;
#4097 = CARTESIAN_POINT ( 'NONE',  ( 0.02407890056655651728, 18.59128259035506758, -24.91982945642901726 ) ) ;
#4100 = DIRECTION ( 'NONE',  ( 1.000000000000000000, 0.000000000000000000, 0.000000000000000000 ) ) ;
#4099 = CARTESIAN_POINT ( 'NONE',  ( -42.55956070192386420, -17.65143121711728469, 20.00000000000000000 ) ) ;
#4098 =( GEOMETRIC_REPRESENTATION_CONTEXT ( 3 ) GLOBAL_UNCERTAINTY_ASSIGNED_CONTEXT ( ( #25613 ) ) GLOBAL_UNIT_ASSIGNED_CONTEXT ( ( #8063, #29960, #10386 ) ) REPRESENTATION_CONTEXT ( 'NONE', 'WORKASPACE' ) );
#4101 = AXIS2_PLACEMENT_3D ( 'NONE', #27486, #32467, #87 ) ;
#4102 = PRESENTATION_LAYER_ASSIGNMENT (  '', '', ( #4676 ) ) ;
#4103 = VECTOR ( 'NONE', #24815, 1000.000000000000000 ) ;
#4104 = CYLINDRICAL_SURFACE ( 'NONE', #28079, 7.999999999999979572 ) ;
#4105 = DIRECTION ( 'NONE',  ( -0.000000000000000000, -0.000000000000000000, -1.000000000000000000 ) ) ;
#4106 = EDGE_LOOP ( 'NONE', ( #34387, #8961, #21574, #7753 ) ) ;
#4107 = CARTESIAN_POINT ( 'NONE',  ( -20.72055270933793736, 25.09707290294331017, -36.68877005347593467 ) ) ;
#4108 = CARTESIAN_POINT ( 'NONE',  ( -414.0000000000000568, -104.9999999999999716, -187.0000000000000000 ) ) ;
#4109 = EDGE_CURVE ( 'NONE', #2043, #30447, #5597, .T. ) ;
#4110 = EDGE_CURVE ( 'NONE', #19142, #3983, #9704, .T. ) ;
#4111 = ORIENTED_EDGE ( 'NONE', *, *, #29540, .T. ) ;
#4112 = EDGE_CURVE ( 'NONE', #3404, #26014, #31422, .T. ) ;
#4113 = SHAPE_REPRESENTATION_RELATIONSHIP ( 'NONE' , 'NONE' ,  #28231, #21564 ) ;
#4114 = ORIENTED_EDGE ( 'NONE', *, *, #26760, .T. ) ;
#4115 = EDGE_CURVE ( 'NONE', #12833, #20076, #34266, .T. ) ;
#4116 = ORIENTED_EDGE ( 'NONE', *, *, #926, .T. ) ;
#4117 = PLANE ( 'NONE',  #17652 ) ;
#4118 = ORIENTED_EDGE ( 'NONE', *, *, #15716, .F. ) ;
#4119 = VERTEX_POINT ( 'NONE', #20234 ) ;
#4120 = ORIENTED_EDGE ( 'NONE', *, *, #30868, .F. ) ;
#4121 = DIRECTION ( 'NONE',  ( -1.000000000000000000, -0.000000000000000000, -0.000000000000000000 ) ) ;
#4122 = AXIS2_PLACEMENT_3D ( 'NONE', #21905, #17293, #25085 ) ;
#4123 = ORIENTED_EDGE ( 'NONE', *, *, #8999, .F. ) ;
#4124 = LINE ( 'NONE', #3428, #5550 ) ;
#4125 = CIRCLE ( 'NONE', #30289, 7.999999999999979572 ) ;
#4126 = CARTESIAN_POINT ( 'NONE',  ( 0.000000000000000000, 0.000000000000000000, 0.000000000000000000 ) ) ;
#4127 = EDGE_LOOP ( 'NONE', ( #32481, #23594, #22478, #16867, #7810, #26595, #31123, #34648, #27327, #23765, #12078, #4724, #5224, #25178, #13103, #22141, #24551, #15238, #7465, #29829, #5738, #32556, #19334, #18094, #9765, #3350, #16939, #30858, #29724, #3826, #25721, #1216, #25840, #12950, #6136, #26942, #22900, #1806, #30887, #27683, #26779, #32432, #27506, #10943, #412, #7981, #18433, #5744, #28230, #33496, #14248, #28777, #26789, #12760, #33737, #7662, #33550, #22826, #33219, #34049, #4114, #34964, #19370 ) ) ;
#4128 = ORIENTED_EDGE ( 'NONE', *, *, #32403, .T. ) ;
#4129 = EDGE_CURVE ( 'NONE', #13694, #12785, #17746, .T. ) ;
#4130 = EDGE_CURVE ( 'NONE', #5771, #34350, #20406, .T. ) ;
#4131 = CIRCLE ( 'NONE', #9283, 3.999999999999976019 ) ;
#4132 = CARTESIAN_POINT ( 'NONE',  ( -110.1150203881707910, 0.000000000000000000, 60.00000000000000000 ) ) ;
#4133 = PLANE ( 'NONE',  #32867 ) ;
#4134 = DIRECTION ( 'NONE',  ( -2.154935995002245207E-17, -0.000000000000000000, -1.000000000000000000 ) ) ;
#4135 = EDGE_CURVE ( 'NONE', #26110, #27224, #20058, .T. ) ;
#4136 = CARTESIAN_POINT ( 'NONE',  ( -20.02113311122498729, -5.758675521474015291, -67.50000000000000000 ) ) ;
#4137 = DIRECTION ( 'NONE',  ( 0.000000000000000000, 1.310824597558155437E-49, 1.000000000000000000 ) ) ;
#4138 = ORIENTED_EDGE ( 'NONE', *, *, #18585, .T. ) ;
#4139 = FACE_OUTER_BOUND ( 'NONE', #385, .T. ) ;
#4140 = DIRECTION ( 'NONE',  ( 0.6876994588534225405, -0.7259954919231316195, 0.000000000000000000 ) ) ;
#4141 = LINE ( 'NONE', #1318, #6224 ) ;
#4142 = EDGE_LOOP ( 'NONE', ( #16622, #6608, #22354, #24302 ) ) ;
#4143 = CARTESIAN_POINT ( 'NONE',  ( 0.1387913946425727574, 13.01149508916974895, 4.463429423125059969 ) ) ;
#4144 = CARTESIAN_POINT ( 'NONE',  ( -37.12776225901827587, -7.411627343331159246, 68.31122994652405112 ) ) ;
#4145 = CARTESIAN_POINT ( 'NONE',  ( 23.93847777447631131, 22.04889236939138186, 68.31122994652405112 ) ) ;
#4146 = FACE_OUTER_BOUND ( 'NONE', #31362, .T. ) ;
#4148 = CARTESIAN_POINT ( 'NONE',  ( -109.5740446912284938, 2.313922778582933493, -7.141321738367096827 ) ) ;
#4147 = CARTESIAN_POINT ( 'NONE',  ( 0.000000000000000000, 14.59907093257217170, 26.74544485249471393 ) ) ;
#4149 = VECTOR ( 'NONE', #15379, 999.9999999999998863 ) ;
#4150 = LINE ( 'NONE', #28203, #25789 ) ;
#4151 = VERTEX_POINT ( 'NONE', #12398 ) ;
#4152 = DIRECTION ( 'NONE',  ( -0.000000000000000000, -1.836970198721029688E-16, 1.000000000000000000 ) ) ;
#4154 = DIRECTION ( 'NONE',  ( -1.000000000000000000, -0.000000000000000000, -0.000000000000000000 ) ) ;
#4153 = DIRECTION ( 'NONE',  ( -0.000000000000000000, -0.000000000000000000, 1.000000000000000000 ) ) ;
#4155 = EDGE_CURVE ( 'NONE', #27008, #20630, #525, .T. ) ;
#4156 = AXIS2_PLACEMENT_3D ( 'NONE', #27199, #27547, #3163 ) ;
#4157 = EDGE_CURVE ( 'NONE', #9482, #31417, #3831, .T. ) ;
#4159 = EDGE_LOOP ( 'NONE', ( #13622, #22176, #15776, #27684 ) ) ;
#4158 = VECTOR ( 'NONE', #14740, 1000.000000000000000 ) ;
#4160 = AXIS2_PLACEMENT_3D ( 'NONE', #11042, #5674, #30084 ) ;
#4161 = CARTESIAN_POINT ( 'NONE',  ( 0.000000000000000000, 0.000000000000000000, 20.00000000000000000 ) ) ;
#4162 = EDGE_CURVE ( 'NONE', #15683, #21641, #4456, .T. ) ;
#4163 = ORIENTED_EDGE ( 'NONE', *, *, #1578, .F. ) ;
#4164 = APPLICATION_CONTEXT ( 'automotive_design' ) ;
#4165 = ADVANCED_FACE ( 'NONE', ( #34621 ), #13029, .T. ) ;
#4166 = ORIENTED_EDGE ( 'NONE', *, *, #30180, .F. ) ;
#4167 = LINE ( 'NONE', #33376, #20218 ) ;
#4168 = ORIENTED_EDGE ( 'NONE', *, *, #2322, .F. ) ;
#4169 = ORIENTED_EDGE ( 'NONE', *, *, #30950, .F. ) ;
#4170 = CARTESIAN_POINT ( 'NONE',  ( -355.0000000000000000, -131.0000000000000000, 126.0000000000000000 ) ) ;
#4171 = FACE_OUTER_BOUND ( 'NONE', #27782, .T. ) ;
#4172 = AXIS2_PLACEMENT_3D ( 'NONE', #31624, #1209, #20777 ) ;
#4173 = LINE ( 'NONE', #15062, #12299 ) ;
#4174 = DIRECTION ( 'NONE',  ( 0.000000000000000000, 0.000000000000000000, 1.000000000000000000 ) ) ;
#4175 = ORIENTED_EDGE ( 'NONE', *, *, #27568, .F. ) ;
#4176 = ORIENTED_EDGE ( 'NONE', *, *, #27559, .T. ) ;
#4177 = FACE_OUTER_BOUND ( 'NONE', #4106, .T. ) ;
#4178 = PLANE ( 'NONE',  #15808 ) ;
#4179 = DIRECTION ( 'NONE',  ( 0.000000000000000000, 1.836970198721029934E-16, -1.000000000000000000 ) ) ;
#4180 = LINE ( 'NONE', #7024, #24359 ) ;
#4181 = CARTESIAN_POINT ( 'NONE',  ( 0.000000000000000000, 3.524919873834583163E-15, 68.31122994652405112 ) ) ;
#4182 = VERTEX_POINT ( 'NONE', #15946 ) ;
#4183 = AXIS2_PLACEMENT_3D ( 'NONE', #23437, #12255, #9399 ) ;
#4184 = DIRECTION ( 'NONE',  ( -1.000000000000000000, 0.000000000000000000, 0.000000000000000000 ) ) ;
#4185 = CIRCLE ( 'NONE', #13304, 3.999999999999976019 ) ;
#4186 = AXIS2_PLACEMENT_3D ( 'NONE', #26311, #31818, #1923 ) ;
#4187 = ORIENTED_EDGE ( 'NONE', *, *, #11783, .T. ) ;
#4188 = EDGE_CURVE ( 'NONE', #16780, #1364, #23588, .T. ) ;
#4189 = CARTESIAN_POINT ( 'NONE',  ( 9.736651044630752594, -33.69708579775585378, -36.68877005347594178 ) ) ;
#4190 = FACE_OUTER_BOUND ( 'NONE', #9934, .T. ) ;
#4191 = CARTESIAN_POINT ( 'NONE',  ( -499.9999999999999432, -145.0000000000000000, -187.0000000000000000 ) ) ;
#4192 = ORIENTED_EDGE ( 'NONE', *, *, #7606, .F. ) ;
#4193 = DIRECTION ( 'NONE',  ( -1.000000000000000000, -0.000000000000000000, -0.000000000000000000 ) ) ;
#4194 = ORIENTED_EDGE ( 'NONE', *, *, #13037, .T. ) ;
#4196 = LINE ( 'NONE', #28599, #17996 ) ;
#4195 = CARTESIAN_POINT ( 'NONE',  ( -20.00000000000001776, -113.0000000000000000, 162.9999999999999716 ) ) ;
#4197 = CARTESIAN_POINT ( 'NONE',  ( -418.0000000000000000, 105.0000000000000142, 187.0000000000000000 ) ) ;
#4198 = EDGE_CURVE ( 'NONE', #3093, #27516, #4691, .T. ) ;
#4199 = EDGE_CURVE ( 'NONE', #23325, #5785, #6757, .T. ) ;
#4200 = EDGE_CURVE ( 'NONE', #14739, #28456, #6512, .T. ) ;
#4201 = VERTEX_POINT ( 'NONE', #10061 ) ;
#4202 = DIRECTION ( 'NONE',  ( -0.9289767198167914186, -0.3701381553399144542, 0.000000000000000000 ) ) ;
#4203 = DIRECTION ( 'NONE',  ( -0.000000000000000000, -1.000000000000000000, -0.000000000000000000 ) ) ;
#4204 = EDGE_LOOP ( 'NONE', ( #19728, #10031, #465, #31777, #8470, #32755, #90, #28432 ) ) ;
#4205 = ORIENTED_EDGE ( 'NONE', *, *, #27074, .T. ) ;
#4206 = AXIS2_PLACEMENT_3D ( 'NONE', #29210, #1456, #4280 ) ;
#4207 = CARTESIAN_POINT ( 'NONE',  ( 803.7752902071640619, 967.3227185528392056, 1753.598338701303419 ) ) ;
#4208 = CONICAL_SURFACE ( 'NONE', #15591, 13.50000000000000000, 1.047197551196600296 ) ;
#4209 = CARTESIAN_POINT ( 'NONE',  ( 100.0393311773591023, -2.890043774996763570, 12.16248655421354385 ) ) ;
#4210 = ORIENTED_EDGE ( 'NONE', *, *, #12447, .T. ) ;
#4211 = CARTESIAN_POINT ( 'NONE',  ( -12.00000000000001066, 144.9999999999999716, -162.9999999999999432 ) ) ;
#4212 = CIRCLE ( 'NONE', #27523, 30.47050528711511674 ) ;
#4213 = DIRECTION ( 'NONE',  ( 0.000000000000000000, 0.000000000000000000, -1.000000000000000000 ) ) ;
#4214 = DIRECTION ( 'NONE',  ( 1.000000000000000000, 0.000000000000000000, 0.000000000000000000 ) ) ;
#4215 = PLANE ( 'NONE',  #18808 ) ;
#4216 = CONTEXT_DEPENDENT_SHAPE_REPRESENTATION ( #26471, #9757 ) ;
#4217 = EDGE_LOOP ( 'NONE', ( #20947, #3687, #25310, #12057 ) ) ;
#4219 = ORIENTED_EDGE ( 'NONE', *, *, #31323, .T. ) ;
#4218 =( REPRESENTATION_RELATIONSHIP ('NONE','NONE', #23037, #8672 ) REPRESENTATION_RELATIONSHIP_WITH_TRANSFORMATION ( #33648 )SHAPE_REPRESENTATION_RELATIONSHIP( ) );
#4220 = VERTEX_POINT ( 'NONE', #5052 ) ;
#4221 = CARTESIAN_POINT ( 'NONE',  ( 5.510910596163086400E-15, 44.99999999999997868, 87.50000000000001421 ) ) ;
#4222 = DIRECTION ( 'NONE',  ( -0.000000000000000000, 1.000000000000000000, -0.000000000000000000 ) ) ;
#4223 = AXIS2_PLACEMENT_3D ( 'NONE', #32623, #19130, #13775 ) ;
#4224 = DIRECTION ( 'NONE',  ( 0.000000000000000000, -1.836970198721029688E-16, 1.000000000000000000 ) ) ;
#4225 = CARTESIAN_POINT ( 'NONE',  ( 3.235562306570555532E-30, 28.08988295778447508, -67.50000000000000000 ) ) ;
#4226 = CARTESIAN_POINT ( 'NONE',  ( -20.00000000000007461, 136.9999999999999432, -162.9999999999999716 ) ) ;
#4227 = DIRECTION ( 'NONE',  ( 0.7259954919231307313, -0.6876994588534234287, -0.000000000000000000 ) ) ;
#4228 = ORIENTED_EDGE ( 'NONE', *, *, #15554, .T. ) ;
#4229 = AXIS2_PLACEMENT_3D ( 'NONE', #21360, #7815, #16024 ) ;
#4230 = CARTESIAN_POINT ( 'NONE',  ( 105.3850032505120424, 5.737785766176326518, 11.10530569653546706 ) ) ;
#4231 = ITEM_DEFINED_TRANSFORMATION ( 'NONE', 'NONE', #21214,  #28566 ) ;
#4232 = VERTEX_POINT ( 'NONE', #31760 ) ;
#4233 = VECTOR ( 'NONE', #16266, 1000.000000000000000 ) ;
#4234 = AXIS2_PLACEMENT_3D ( 'NONE', #32610, #13415, #8580 ) ;
#4235 = EDGE_CURVE ( 'NONE', #29254, #3503, #20422, .T. ) ;
#4236 = DIRECTION ( 'NONE',  ( -1.000000000000000000, 0.000000000000000000, 0.000000000000000000 ) ) ;
#4237 = ORIENTED_EDGE ( 'NONE', *, *, #2585, .F. ) ;
#4238 = CARTESIAN_POINT ( 'NONE',  ( -110.1150203881707910, -7.176976838982289656E-16, -12.50000000000000000 ) ) ;
#4239 = ADVANCED_FACE ( 'NONE', ( #26599 ), #13266, .F. ) ;
#4240 = CARTESIAN_POINT ( 'NONE',  ( -430.0000000000000000, 130.9999999999999716, 113.9999999999999858 ) ) ;
#4241 = ADVANCED_FACE ( 'NONE', ( #2563, #31592 ), #7197, .T. ) ;
#4242 = CARTESIAN_POINT ( 'NONE',  ( 0.02407890056655695096, -26.45933846664205902, 16.32596387352436551 ) ) ;
#4243 = LINE ( 'NONE', #10295, #22447 ) ;
#4245 = ADVANCED_FACE ( 'NONE', ( #32286 ), #21267, .T. ) ;
#4244 = CARTESIAN_POINT ( 'NONE',  ( 0.000000000000000000, -13.59935610937951900, -28.90010281771846223 ) ) ;
#4246 = ORIENTED_EDGE ( 'NONE', *, *, #31612, .F. ) ;
#4247 = AXIS2_PLACEMENT_3D ( 'NONE', #25281, #25807, #6584 ) ;
#4248 = EDGE_LOOP ( 'NONE', ( #3740, #27735, #10056, #18991 ) ) ;
#4249 = DIRECTION ( 'NONE',  ( -0.1063910735369017202, 0.9943243633099136947, -1.000770725407181676E-14 ) ) ;
#4250 = EDGE_LOOP ( 'NONE', ( #16563, #28610, #3845, #11351 ) ) ;
#4251 = TOROIDAL_SURFACE ( 'NONE', #11678, 30.47050528711512030, 8.000000000000000000 ) ;
#4252 = EDGE_CURVE ( 'NONE', #20322, #28753, #7368, .T. ) ;
#4253 = CARTESIAN_POINT ( 'NONE',  ( -109.0426547331720855, -3.150844840328208996, 6.812360382669037762 ) ) ;
#4254 = DIRECTION ( 'NONE',  ( 0.000000000000000000, 0.000000000000000000, -1.000000000000000000 ) ) ;
#4255 = AXIS2_PLACEMENT_3D ( 'NONE', #24678, #22031, #3151 ) ;
#4256 = FACE_OUTER_BOUND ( 'NONE', #1982, .T. ) ;
#4257 = ITEM_DEFINED_TRANSFORMATION ( 'NONE', 'NONE', #17254,  #28566 ) ;
#4258 = TOROIDAL_SURFACE ( 'NONE', #29276, 10.30000000000000071, 0.3000000000000025424 ) ;
#4259 = VERTEX_POINT ( 'NONE', #18258 ) ;
#4260 = CARTESIAN_POINT ( 'NONE',  ( -32.17792593279633451, -19.96555837188923022, 68.31122994652405112 ) ) ;
#4261 = CARTESIAN_POINT ( 'NONE',  ( -9.978866888775527855, 8.235406450278430768, -87.50000000000000000 ) ) ;
#4262 = CIRCLE ( 'NONE', #8820, 32.54542015209054995 ) ;
#4264 = LINE ( 'NONE', #25987, #4434 ) ;
#4263 = LINE ( 'NONE', #4432, #18465 ) ;
#4265 = ORIENTED_EDGE ( 'NONE', *, *, #2309, .F. ) ;
#4266 = ORIENTED_EDGE ( 'NONE', *, *, #16350, .T. ) ;
#4267 = CARTESIAN_POINT ( 'NONE',  ( -12.00000000000001243, 134.9999999999999432, -154.9999999999999716 ) ) ;
#4268 = CARTESIAN_POINT ( 'NONE',  ( 0.000000000000000000, 30.40449935640661039, 2.004522720844265304 ) ) ;
#4269 = CARTESIAN_POINT ( 'NONE',  ( 8.986540508143578521, 33.69708579775584667, 49.43553178847298568 ) ) ;
#4270 = ORIENTED_EDGE ( 'NONE', *, *, #32781, .T. ) ;
#4271 = VECTOR ( 'NONE', #19526, 1000.000000000000000 ) ;
#4272 = PLANE ( 'NONE',  #13542 ) ;
#4273 = ORIENTED_EDGE ( 'NONE', *, *, #4986, .F. ) ;
#4274 = DIRECTION ( 'NONE',  ( 0.000000000000000000, 0.000000000000000000, 1.000000000000000000 ) ) ;
#4275 = CARTESIAN_POINT ( 'NONE',  ( 0.000000000000000000, 0.000000000000000000, 20.00000000000000000 ) ) ;
#4276 = ADVANCED_FACE ( 'NONE', ( #26250 ), #10595, .F. ) ;
#4277 = LINE ( 'NONE', #4613, #1905 ) ;
#4279 = PLANE ( 'NONE',  #11712 ) ;
#4278 = CARTESIAN_POINT ( 'NONE',  ( -35.00000000000000000, -4.831299144296466785, -15.81122994652406355 ) ) ;
#4280 = DIRECTION ( 'NONE',  ( 0.000000000000000000, 0.000000000000000000, -1.000000000000000000 ) ) ;
#4281 = CARTESIAN_POINT ( 'NONE',  ( -355.0000000000000000, -135.0000000000000000, 126.0000000000000000 ) ) ;
#4282 = DIRECTION ( 'NONE',  ( 0.000000000000000000, 0.000000000000000000, 1.000000000000000000 ) ) ;
#4284 = EDGE_CURVE ( 'NONE', #30712, #2971, #34800, .T. ) ;
#4283 = CARTESIAN_POINT ( 'NONE',  ( 0.000000000000000000, -11.69134295108990607, 6.750000000000024869 ) ) ;
#4285 = VECTOR ( 'NONE', #28507, 1000.000000000000227 ) ;
#4286 = EDGE_CURVE ( 'NONE', #33838, #28629, #19301, .T. ) ;
#4287 = VERTEX_POINT ( 'NONE', #1864 ) ;
#4288 = EDGE_CURVE ( 'NONE', #12838, #28732, #5222, .T. ) ;
#4289 = ADVANCED_FACE ( 'NONE', ( #29281 ), #4873, .F. ) ;
#4290 = ORIENTED_EDGE ( 'NONE', *, *, #10214, .F. ) ;
#4291 = ORIENTED_EDGE ( 'NONE', *, *, #18038, .F. ) ;
#4292 = AXIS2_PLACEMENT_3D ( 'NONE', #4869, #2044, #15768 ) ;
#4293 = DIRECTION ( 'NONE',  ( -1.000000000000000000, 0.000000000000000000, 0.000000000000000000 ) ) ;
#4294 = ORIENTED_EDGE ( 'NONE', *, *, #6081, .T. ) ;
#4295 = EDGE_LOOP ( 'NONE', ( #7356, #9666, #24294, #16465 ) ) ;
#4296 = ORIENTED_EDGE ( 'NONE', *, *, #4439, .F. ) ;
#4297 = DIRECTION ( 'NONE',  ( -1.000000000000000000, -0.000000000000000000, -0.000000000000000000 ) ) ;
#4298 = CIRCLE ( 'NONE', #28178, 7.999999999999979572 ) ;
#4299 = EDGE_CURVE ( 'NONE', #7716, #14308, #7768, .T. ) ;
#4300 = EDGE_LOOP ( 'NONE', ( #16936, #7458, #13111, #5106 ) ) ;
#4301 = DIRECTION ( 'NONE',  ( 1.000000000000000000, -0.000000000000000000, -0.000000000000000000 ) ) ;
#4302 = CARTESIAN_POINT ( 'NONE',  ( 0.7564103425703777583, 27.12319051591914487, 20.36165095825682414 ) ) ;
#4303 = ORIENTED_EDGE ( 'NONE', *, *, #29931, .F. ) ;
#4304 = ORIENTED_EDGE ( 'NONE', *, *, #33067, .F. ) ;
#4305 = CARTESIAN_POINT ( 'NONE',  ( -9.419006373467819770E-16, -1.318430554023032553, 13.49999999999999822 ) ) ;
#4306 = LINE ( 'NONE', #25682, #6157 ) ;
#4307 = VECTOR ( 'NONE', #35083, 1000.000000000000000 ) ;
#4308 = LINE ( 'NONE', #31207, #18756 ) ;
#4309 = DIRECTION ( 'NONE',  ( 1.000000000000000000, 0.000000000000000000, 0.000000000000000000 ) ) ;
#4310 = DIRECTION ( 'NONE',  ( 0.000000000000000000, 2.309213040847544338E-50, 1.000000000000000000 ) ) ;
#4311 = ORIENTED_EDGE ( 'NONE', *, *, #4030, .F. ) ;
#4312 = FACE_OUTER_BOUND ( 'NONE', #33109, .T. ) ;
#4313 = DIRECTION ( 'NONE',  ( 0.000000000000000000, -1.836970198721029934E-16, 1.000000000000000000 ) ) ;
#4314 = CIRCLE ( 'NONE', #25999, 4.750000000000004441 ) ;
#4315 = FACE_OUTER_BOUND ( 'NONE', #14554, .T. ) ;
#4316 = VERTEX_POINT ( 'NONE', #13970 ) ;
#4317 = LINE ( 'NONE', #15202, #15106 ) ;
#4318 = DIRECTION ( 'NONE',  ( 1.000000000000000000, 3.469446951953834515E-18, 0.000000000000000000 ) ) ;
#4319 = FILL_AREA_STYLE ('',( #28720 ) ) ;
#4320 = CARTESIAN_POINT ( 'NONE',  ( -1.625000000000000000, 2.702098422956710877, 4.679999999999999716 ) ) ;
#4322 = CARTESIAN_POINT ( 'NONE',  ( -103.3138142205062024, 4.840548292904077066, -5.731216124222060060 ) ) ;
#4321 = CARTESIAN_POINT ( 'NONE',  ( -347.0000000000000000, -135.0000000000000000, 114.0000000000000000 ) ) ;
#4323 = VECTOR ( 'NONE', #6410, 1000.000000000000000 ) ;
#4324 = CARTESIAN_POINT ( 'NONE',  ( -1.307386931792819285, 32.51914993179678959, 68.31122994652405112 ) ) ;
#4325 = ORIENTED_EDGE ( 'NONE', *, *, #324, .F. ) ;
#4326 = CARTESIAN_POINT ( 'NONE',  ( -441.9999999999999432, 109.0000000000000142, -155.0000000000000000 ) ) ;
#4328 = CARTESIAN_POINT ( 'NONE',  ( 0.000000000000000000, -31.68806325674604452, -4.003133335385915537 ) ) ;
#4327 = CARTESIAN_POINT ( 'NONE',  ( -3.250000000000000000, 5.404196845913421754, -0.7500000000000000000 ) ) ;
#4329 = AXIS2_PLACEMENT_3D ( 'NONE', #5622, #19357, #14199 ) ;
#4330 = VERTEX_POINT ( 'NONE', #2739 ) ;
#4331 = EDGE_CURVE ( 'NONE', #15148, #28176, #22147, .T. ) ;
#4332 = ADVANCED_FACE ( 'NONE', ( #3268 ), #2908, .F. ) ;
#4333 = DIRECTION ( 'NONE',  ( 1.000000000000000000, 0.000000000000000000, -0.000000000000000000 ) ) ;
#4334 = VECTOR ( 'NONE', #24783, 1000.000000000000000 ) ;
#4335 = ORIENTED_EDGE ( 'NONE', *, *, #25985, .T. ) ;
#4336 = EDGE_LOOP ( 'NONE', ( #30738, #3257, #24577, #34392 ) ) ;
#4337 = LINE ( 'NONE', #26232, #24741 ) ;
#4338 = EDGE_LOOP ( 'NONE', ( #32300, #31582, #259, #10240 ) ) ;
#4339 = ORIENTED_EDGE ( 'NONE', *, *, #18971, .F. ) ;
#4340 = DIRECTION ( 'NONE',  ( 0.000000000000000000, 0.000000000000000000, 1.000000000000000000 ) ) ;
#4341 = PRODUCT_DEFINITION_SHAPE ( 'NONE', 'NONE',  #35129 ) ;
#4342 = AXIS2_PLACEMENT_3D ( 'NONE', #20835, #9464, #18016 ) ;
#4343 = EDGE_CURVE ( 'NONE', #3555, #18475, #16832, .T. ) ;
#4344 = AXIS2_PLACEMENT_3D ( 'NONE', #31130, #25423, #11744 ) ;
#4345 = CARTESIAN_POINT ( 'NONE',  ( -5.469264258321805627, 1.713938105891546382, 0.000000000000000000 ) ) ;
#4346 = DIRECTION ( 'NONE',  ( -1.000000000000000000, 0.000000000000000000, 1.848892746611746966E-32 ) ) ;
#4347 = ORIENTED_EDGE ( 'NONE', *, *, #32215, .T. ) ;
#4348 = EDGE_LOOP ( 'NONE', ( #21678, #3670, #12559, #13536 ) ) ;
#4349 = DIRECTION ( 'NONE',  ( 0.000000000000000000, 0.000000000000000000, 1.000000000000000000 ) ) ;
#4350 = DIRECTION ( 'NONE',  ( -1.000000000000000000, -0.000000000000000000, -0.000000000000000000 ) ) ;
#4351 = CARTESIAN_POINT ( 'NONE',  ( 50.00050000000000239, 9.539392014169456147, 3.000000000000000000 ) ) ;
#4352 = EDGE_CURVE ( 'NONE', #5869, #3078, #14204, .T. ) ;
#4353 = CARTESIAN_POINT ( 'NONE',  ( 2.765921099433441999, -31.05158812718222450, 1.559667679918499417 ) ) ;
#4354 = CARTESIAN_POINT ( 'NONE',  ( -363.0000000000000000, -125.0000000000000284, 168.9999999999999716 ) ) ;
#4355 = ORIENTED_EDGE ( 'NONE', *, *, #22212, .F. ) ;
#4356 = ADVANCED_FACE ( 'NONE', ( #76 ), #10938, .T. ) ;
#4357 = EDGE_CURVE ( 'NONE', #27282, #5434, #22849, .T. ) ;
#4358 = CARTESIAN_POINT ( 'NONE',  ( -12.00000000000001066, -141.0000000000000000, 174.9999999999999432 ) ) ;
#4359 = DIRECTION ( 'NONE',  ( -1.000000000000000000, -3.469446951953834515E-18, 0.000000000000000000 ) ) ;
#4360 = VERTEX_POINT ( 'NONE', #6274 ) ;
#4361 = CARTESIAN_POINT ( 'NONE',  ( 0.000000000000000000, -14.75935258146432005, 26.65732927035515232 ) ) ;
#4362 = ADVANCED_FACE ( 'NONE', ( #6984 ), #33696, .F. ) ;
#4363 = FACE_OUTER_BOUND ( 'NONE', #4142, .T. ) ;
#4364 = DIRECTION ( 'NONE',  ( -1.000000000000000000, 0.000000000000000000, 0.000000000000000000 ) ) ;
#4365 = ORIENTED_EDGE ( 'NONE', *, *, #21259, .F. ) ;
#4366 = CARTESIAN_POINT ( 'NONE',  ( 11.99999999999999645, -55.00000000000002132, 159.0000000000000000 ) ) ;
#4367 = EDGE_LOOP ( 'NONE', ( #33169, #27149, #32648, #21965, #16147, #24832, #24199 ) ) ;
#4369 = CARTESIAN_POINT ( 'NONE',  ( -430.0000000000000000, 118.9999999999999858, 111.9999999999999858 ) ) ;
#4368 = PLANE ( 'NONE',  #34739 ) ;
#4370 = DIRECTION ( 'NONE',  ( -0.000000000000000000, 1.000000000000000000, -0.000000000000000000 ) ) ;
#4371 = VECTOR ( 'NONE', #6199, 1000.000000000000000 ) ;
#4372 = AXIS2_PLACEMENT_3D ( 'NONE', #28974, #10107, #7417 ) ;
#4373 = CIRCLE ( 'NONE', #23725, 34.41491905851385269 ) ;
#4374 = EDGE_LOOP ( 'NONE', ( #22803, #11011, #12293, #32546, #30410, #4291 ) ) ;
#4375 = CARTESIAN_POINT ( 'NONE',  ( -499.9999999999999432, 112.9999999999999574, -190.9999999999999716 ) ) ;
#4376 = CARTESIAN_POINT ( 'NONE',  ( 2.789999999999999147, -14.75935258146429341, 26.65732927035513811 ) ) ;
#4377 = ORIENTED_EDGE ( 'NONE', *, *, #34606, .F. ) ;
#4378 = AXIS2_PLACEMENT_3D ( 'NONE', #17225, #3659, #11878 ) ;
#4379 = DIRECTION ( 'NONE',  ( -0.1063910735369225230, 0.9943243633099118073, -1.000770725407345128E-14 ) ) ;
#4380 = VERTEX_POINT ( 'NONE', #25507 ) ;
#4381 = CARTESIAN_POINT ( 'NONE',  ( 100.6898240025452793, -3.792433597769625298, 11.91175651985687267 ) ) ;
#4382 = EDGE_LOOP ( 'NONE', ( #22835, #31284, #25271, #23563, #29961, #31171, #28671, #30939 ) ) ;
#4383 = DIRECTION ( 'NONE',  ( 0.000000000000000000, 0.000000000000000000, 1.000000000000000000 ) ) ;
#4384 = DIRECTION ( 'NONE',  ( -1.000000000000000000, 0.000000000000000000, 0.000000000000000000 ) ) ;
#4385 = VECTOR ( 'NONE', #1005, 1000.000000000000000 ) ;
#4386 = DIRECTION ( 'NONE',  ( 0.000000000000000000, 1.000000000000000000, 5.145227585319922065E-49 ) ) ;
#4387 = CARTESIAN_POINT ( 'NONE',  ( 0.000000000000000000, 0.000000000000000000, 13.00000000000000000 ) ) ;
#4388 = CONTEXT_DEPENDENT_SHAPE_REPRESENTATION ( #10580, #10050 ) ;
#4389 = ORIENTED_EDGE ( 'NONE', *, *, #25837, .T. ) ;
#4390 = ORIENTED_EDGE ( 'NONE', *, *, #28648, .T. ) ;
#4391 = ORIENTED_EDGE ( 'NONE', *, *, #15235, .F. ) ;
#4392 = PRODUCT_DEFINITION_SHAPE ( 'NONE', 'NONE',  #35112 ) ;
#4393 = CARTESIAN_POINT ( 'NONE',  ( -499.9999999999999432, -137.0000000000000000, -190.9999999999999716 ) ) ;
#4394 = DIRECTION ( 'NONE',  ( -1.000000000000000000, -0.000000000000000000, -0.000000000000000000 ) ) ;
#4395 = ADVANCED_FACE ( 'NONE', ( #14501 ), #19841, .F. ) ;
#4396 = AXIS2_PLACEMENT_3D ( 'NONE', #27265, #16080, #26913 ) ;
#4397 = VECTOR ( 'NONE', #1414, 1000.000000000000000 ) ;
#4398 = EDGE_CURVE ( 'NONE', #4705, #20910, #34075, .T. ) ;
#4399 = CARTESIAN_POINT ( 'NONE',  ( 2.261199745872888744, 33.21438043751174973, 3.418204286533153446 ) ) ;
#4400 = CARTESIAN_POINT ( 'NONE',  ( -12.00000000000001066, 124.9999999999999716, 162.9999999999999716 ) ) ;
#4401 = LINE ( 'NONE', #15293, #20876 ) ;
#4402 = CARTESIAN_POINT ( 'NONE',  ( -418.0000000000000000, -124.9999999999999716, 139.9999999999999716 ) ) ;
#4403 = EDGE_LOOP ( 'NONE', ( #14298, #34100, #23735, #8109, #27306, #23278, #16549, #34199, #20809, #21026, #31588 ) ) ;
#4404 = DIRECTION ( 'NONE',  ( 0.000000000000000000, 0.000000000000000000, 1.000000000000000000 ) ) ;
#4405 = VECTOR ( 'NONE', #7544, 1000.000000000000000 ) ;
#4406 = ORIENTED_EDGE ( 'NONE', *, *, #27074, .F. ) ;
#4407 = CARTESIAN_POINT ( 'NONE',  ( -445.9999999999999432, 113.0000000000000000, -175.0000000000000000 ) ) ;
#4408 = ORIENTED_EDGE ( 'NONE', *, *, #23641, .F. ) ;
#4409 = FACE_OUTER_BOUND ( 'NONE', #21454, .T. ) ;
#4410 = CARTESIAN_POINT ( 'NONE',  ( -12.00000000000001066, 144.9999999999999147, 155.0000000000000000 ) ) ;
#4411 = B_SPLINE_CURVE_WITH_KNOTS ( 'NONE', 3,
 ( #18324, #26485, #12973, #29157, #4753, #18505 ),
 .UNSPECIFIED., .F., .F.,
 ( 4, 2, 4 ),
 ( 0.04390953152370602464, 0.04785567665046381453, 0.05180182177722160441 ),
 .UNSPECIFIED. ) ;
#4412 = CIRCLE ( 'NONE', #24306, 7.999999999999979572 ) ;
#4413 = CARTESIAN_POINT ( 'NONE',  ( -499.9999999999999432, -137.0000000000000000, -187.0000000000000000 ) ) ;
#4414 = DIRECTION ( 'NONE',  ( 0.000000000000000000, 0.000000000000000000, 1.000000000000000000 ) ) ;
#4415 = VERTEX_POINT ( 'NONE', #23203 ) ;
#4416 = CIRCLE ( 'NONE', #28250, 1.649999999999999467 ) ;
#4417 = VECTOR ( 'NONE', #1425, 1000.000000000000000 ) ;
#4418 = EDGE_LOOP ( 'NONE', ( #13811, #31599, #10235, #6638 ) ) ;
#4419 = DIRECTION ( 'NONE',  ( -0.1063910735369017202, 0.9943243633099136947, -1.000770725407181676E-14 ) ) ;
#4420 =( REPRESENTATION_RELATIONSHIP ('NONE','NONE', #23037, #28231 ) REPRESENTATION_RELATIONSHIP_WITH_TRANSFORMATION ( #14134 )SHAPE_REPRESENTATION_RELATIONSHIP( ) );
#4421 = VERTEX_POINT ( 'NONE', #15193 ) ;
#4422 = CIRCLE ( 'NONE', #34581, 4.000000000000003553 ) ;
#4423 = CARTESIAN_POINT ( 'NONE',  ( 0.7561992169675183506, -32.97757984916171381, -7.919492155588399918 ) ) ;
#4424 = PLANE ( 'NONE',  #21276 ) ;
#4425 = CARTESIAN_POINT ( 'NONE',  ( 100.0637405348225144, -2.948796715283049874, 6.904248079351286371 ) ) ;
#4426 = CONTEXT_DEPENDENT_SHAPE_REPRESENTATION ( #25112, #21139 ) ;
#4427 = EDGE_LOOP ( 'NONE', ( #1158, #7109, #33611, #4266 ) ) ;
#4428 = CARTESIAN_POINT ( 'NONE',  ( -18.07349068442144358, -27.06572199953719604, -36.68877005347593467 ) ) ;
#4429 = ADVANCED_FACE ( 'NONE', ( #23028 ), #33880, .T. ) ;
#4430 = AXIS2_PLACEMENT_3D ( 'NONE', #14459, #6231, #1268 ) ;
#4431 = EDGE_CURVE ( 'NONE', #23023, #10318, #15020, .T. ) ;
#4433 = CYLINDRICAL_SURFACE ( 'NONE', #13006, 3.999999999999976019 ) ;
#4432 = CARTESIAN_POINT ( 'NONE',  ( -15.99999999999998579, 144.9999999999999716, 162.9999999999999716 ) ) ;
#4434 = VECTOR ( 'NONE', #10142, 1000.000000000000000 ) ;
#4435 = ORIENTED_EDGE ( 'NONE', *, *, #20467, .F. ) ;
#4436 = ORIENTED_EDGE ( 'NONE', *, *, #20528, .F. ) ;
#4437 = DIRECTION ( 'NONE',  ( -0.000000000000000000, -0.000000000000000000, -1.000000000000000000 ) ) ;
#4438 = ORIENTED_EDGE ( 'NONE', *, *, #1518, .F. ) ;
#4439 = EDGE_CURVE ( 'NONE', #32813, #26771, #28367, .T. ) ;
#4440 = CARTESIAN_POINT ( 'NONE',  ( -145.0000000000000568, -87.50000000000000000, 65.00000000000000000 ) ) ;
#4441 = CARTESIAN_POINT ( 'NONE',  ( 0.000000000000000000, 1.592040838891559095E-15, -13.00000000000000000 ) ) ;
#4442 = EDGE_LOOP ( 'NONE', ( #8413, #4726, #24882, #34079 ) ) ;
#4443 = VECTOR ( 'NONE', #1560, 1000.000000000000000 ) ;
#4444 = CARTESIAN_POINT ( 'NONE',  ( 19.99999999999996092, -145.0000000000000000, -186.9999999999999716 ) ) ;
#4445 = ORIENTED_EDGE ( 'NONE', *, *, #17253, .T. ) ;
#4446 = CARTESIAN_POINT ( 'NONE',  ( 0.02407890056655564992, 31.00221527374952046, 2.344426712874309260 ) ) ;
#4447 = CARTESIAN_POINT ( 'NONE',  ( -12.00000000000001066, 136.9999999999999716, -155.0000000000000000 ) ) ;
#4448 = CARTESIAN_POINT ( 'NONE',  ( -500.0000000000000000, -113.0000000000000000, 190.9999999999999716 ) ) ;
#4449 =( GEOMETRIC_REPRESENTATION_CONTEXT ( 3 ) GLOBAL_UNCERTAINTY_ASSIGNED_CONTEXT ( ( #33141 ) ) GLOBAL_UNIT_ASSIGNED_CONTEXT ( ( #29332, #1912, #12795 ) ) REPRESENTATION_CONTEXT ( 'NONE', 'WORKASPACE' ) );
#4451 = FACE_OUTER_BOUND ( 'NONE', #6884, .T. ) ;
#4450 = CARTESIAN_POINT ( 'NONE',  ( 1.040000000000001812, -34.41385771548413430, -0.2702793785573777696 ) ) ;
#4452 = CARTESIAN_POINT ( 'NONE',  ( 12.46788440507149964, 30.06253867087539078, -36.68877005347593467 ) ) ;
#4453 = PLANE ( 'NONE',  #83 ) ;
#4454 = CARTESIAN_POINT ( 'NONE',  ( 2.789999999999999147, 28.06759692514783922, -11.78059558880183921 ) ) ;
#4455 = CARTESIAN_POINT ( 'NONE',  ( 11.99999999999999645, 144.9999999999999716, -194.9999999999999432 ) ) ;
#4456 = CIRCLE ( 'NONE', #18701, 7.999999999999979572 ) ;
#4457 = ORIENTED_EDGE ( 'NONE', *, *, #3918, .T. ) ;
#4458 =( NAMED_UNIT ( * ) PLANE_ANGLE_UNIT ( ) SI_UNIT ( $, .RADIAN. ) );
#4459 = ORIENTED_EDGE ( 'NONE', *, *, #29162, .F. ) ;
#4460 = ORIENTED_EDGE ( 'NONE', *, *, #34428, .F. ) ;
#4461 = AXIS2_PLACEMENT_3D ( 'NONE', #31281, #6881, #28959 ) ;
#4462 = CARTESIAN_POINT ( 'NONE',  ( 1.749999999999999778, 0.000000000000000000, 0.000000000000000000 ) ) ;
#4463 = ORIENTED_EDGE ( 'NONE', *, *, #29097, .T. ) ;
#4464 = ORIENTED_EDGE ( 'NONE', *, *, #16564, .T. ) ;
#4465 = VERTEX_POINT ( 'NONE', #1138 ) ;
#4466 = CARTESIAN_POINT ( 'NONE',  ( -35.00000000000000000, 16.36947364650383818, -36.69637551990492597 ) ) ;
#4467 = EDGE_CURVE ( 'NONE', #31336, #5775, #4308, .T. ) ;
#4468 = VECTOR ( 'NONE', #16474, 1000.000000000000000 ) ;
#4469 = ITEM_DEFINED_TRANSFORMATION ( 'NONE', 'NONE', #13302,  #28566 ) ;
#4470 = VERTEX_POINT ( 'NONE', #1483 ) ;
#4471 = DIRECTION ( 'NONE',  ( 1.000000000000000000, 0.000000000000000000, -1.232595164407831220E-32 ) ) ;
#4472 = DIRECTION ( 'NONE',  ( 0.000000000000000000, 0.000000000000000000, 1.000000000000000000 ) ) ;
#4473 = ORIENTED_EDGE ( 'NONE', *, *, #8466, .T. ) ;
#4474 = ORIENTED_EDGE ( 'NONE', *, *, #4439, .T. ) ;
#4475 = DIRECTION ( 'NONE',  ( -0.000000000000000000, -0.000000000000000000, -1.000000000000000000 ) ) ;
#4476 = CYLINDRICAL_SURFACE ( 'NONE', #23230, 7.500000000000000000 ) ;
#4477 = EDGE_CURVE ( 'NONE', #20630, #26019, #9318, .T. ) ;
#4478 = DIRECTION ( 'NONE',  ( 0.000000000000000000, -1.000000000000000000, 0.000000000000000000 ) ) ;
#4479 = CARTESIAN_POINT ( 'NONE',  ( -363.0000000000000000, 134.9999999999999716, 113.9999999999999858 ) ) ;
#4480 = DIRECTION ( 'NONE',  ( -1.000000000000000000, -0.000000000000000000, -0.000000000000000000 ) ) ;
#4481 = ORIENTED_EDGE ( 'NONE', *, *, #29502, .F. ) ;
#4482 = DIRECTION ( 'NONE',  ( 0.000000000000000000, 1.000000000000000000, 0.000000000000000000 ) ) ;
#4483 = LINE ( 'NONE', #10021, #1472 ) ;
#4484 = VECTOR ( 'NONE', #15412, 1000.000000000000000 ) ;
#4485 = EDGE_CURVE ( 'NONE', #21809, #5416, #7331, .T. ) ;
#4486 = CYLINDRICAL_SURFACE ( 'NONE', #7347, 16.19999999999999218 ) ;
#4487 = ORIENTED_EDGE ( 'NONE', *, *, #6509, .T. ) ;
#4488 = PLANE ( 'NONE',  #5978 ) ;
#4489 = LINE ( 'NONE', #15204, #28043 ) ;
#4490 = EDGE_CURVE ( 'NONE', #23180, #25989, #15874, .T. ) ;
#4491 = CARTESIAN_POINT ( 'NONE',  ( 105.3925314386741405, 5.728031835420551943, -4.841551550731546527 ) ) ;
#4492 = DIRECTION ( 'NONE',  ( -1.000000000000000000, 0.000000000000000000, -1.300283923313630633E-47 ) ) ;
#4493 = VECTOR ( 'NONE', #23707, 1000.000000000000114 ) ;
#4494 = CARTESIAN_POINT ( 'NONE',  ( 22.89764159710615132, -1.579009122040560431, -87.50000000000000000 ) ) ;
#4495 = ORIENTED_EDGE ( 'NONE', *, *, #20466, .F. ) ;
#4496 = CARTESIAN_POINT ( 'NONE',  ( 104.6149967494879149, 5.737785766176327407, -11.10530569653546706 ) ) ;
#4498 = DIRECTION ( 'NONE',  ( 0.8835120444460224931, 0.4684084406997908179, 0.000000000000000000 ) ) ;
#4497 = CARTESIAN_POINT ( 'NONE',  ( 2.765921099433441555, 18.59128259035472297, 24.91982945642928016 ) ) ;
#4499 = VECTOR ( 'NONE', #5934, 1000.000000000000000 ) ;
#4500 = VERTEX_POINT ( 'NONE', #12002 ) ;
#4501 = CARTESIAN_POINT ( 'NONE',  ( 0.000000000000000000, 0.000000000000000000, 3.930000000000000160 ) ) ;
#4502 = EDGE_LOOP ( 'NONE', ( #15801, #16144, #1860, #32324 ) ) ;
#4503 = AXIS2_PLACEMENT_3D ( 'NONE', #3753, #12314, #22456 ) ;
#4504 = ORIENTED_EDGE ( 'NONE', *, *, #19900, .F. ) ;
#4505 = DIRECTION ( 'NONE',  ( -0.000000000000000000, 1.000000000000000000, -0.000000000000000000 ) ) ;
#4506 = EDGE_LOOP ( 'NONE', ( #11278, #34670, #29150, #31565, #17856, #4597, #6221, #336 ) ) ;
#4507 = VERTEX_POINT ( 'NONE', #33521 ) ;
#4508 = LINE ( 'NONE', #15399, #17907 ) ;
#4509 = CARTESIAN_POINT ( 'NONE',  ( 8.000000000000000000, 0.000000000000000000, 0.000000000000000000 ) ) ;
#4510 = DIRECTION ( 'NONE',  ( 0.000000000000000000, 0.000000000000000000, 1.000000000000000000 ) ) ;
#4511 = VERTEX_POINT ( 'NONE', #30683 ) ;
#4512 = ORIENTED_EDGE ( 'NONE', *, *, #24251, .F. ) ;
#4513 = CARTESIAN_POINT ( 'NONE',  ( -430.0000000000000000, 130.9999999999999716, 130.0000000000000000 ) ) ;
#4514 = CARTESIAN_POINT ( 'NONE',  ( -418.0000000000000000, -104.9999999999999858, -162.9999999999999716 ) ) ;
#4515 = DIRECTION ( 'NONE',  ( 0.000000000000000000, 1.000000000000000000, 0.000000000000000000 ) ) ;
#4516 = EDGE_CURVE ( 'NONE', #25899, #17680, #25683, .T. ) ;
#4517 = CARTESIAN_POINT ( 'NONE',  ( 0.000000000000000000, 11.30192140231274500, -28.29696565125059493 ) ) ;
#4518 = CARTESIAN_POINT ( 'NONE',  ( 1.394999999999999574, 22.14447232807506438, 26.34405054495565679 ) ) ;
#4519 = ORIENTED_EDGE ( 'NONE', *, *, #16453, .F. ) ;
#4520 = AXIS2_PLACEMENT_3D ( 'NONE', #11723, #6536, #20085 ) ;
#4521 = ORIENTED_EDGE ( 'NONE', *, *, #22881, .F. ) ;
#4522 = LINE ( 'NONE', #15416, #17942 ) ;
#4523 = ADVANCED_FACE ( 'NONE', ( #25864, #12352 ), #28008, .T. ) ;
#4524 = EDGE_CURVE ( 'NONE', #34913, #18033, #33683, .T. ) ;
#4525 = CARTESIAN_POINT ( 'NONE',  ( 0.1387913946425762823, -10.37119081301008272, 9.036570576874970229 ) ) ;
#4526 = ORIENTED_EDGE ( 'NONE', *, *, #9720, .T. ) ;
#4527 = PLANE ( 'NONE',  #26440 ) ;
#4528 = CARTESIAN_POINT ( 'NONE',  ( 2.789999999999999147, -7.666252171205694133, 29.49034198003803198 ) ) ;
#4529 = DIRECTION ( 'NONE',  ( 0.000000000000000000, 0.000000000000000000, 1.000000000000000000 ) ) ;
#4530 = ORIENTED_EDGE ( 'NONE', *, *, #18901, .F. ) ;
#4531 = LINE ( 'NONE', #24111, #11546 ) ;
#4532 = ORIENTED_EDGE ( 'NONE', *, *, #9727, .F. ) ;
#4534 = LINE ( 'NONE', #21106, #9445 ) ;
#4533 =( NAMED_UNIT ( * ) PLANE_ANGLE_UNIT ( ) SI_UNIT ( $, .RADIAN. ) );
#4535 = CARTESIAN_POINT ( 'NONE',  ( -12.00000000000003908, -134.9999999999999716, -194.9999999999999432 ) ) ;
#4536 = EDGE_CURVE ( 'NONE', #10851, #30170, #6457, .T. ) ;
#4537 = ORIENTED_EDGE ( 'NONE', *, *, #19786, .T. ) ;
#4538 = CARTESIAN_POINT ( 'NONE',  ( 11.99999999999999645, 112.9999999999999574, -175.0000000000000284 ) ) ;
#4539 = DIRECTION ( 'NONE',  ( 1.000000000000000000, 0.000000000000000000, 0.000000000000000000 ) ) ;
#4540 = EDGE_CURVE ( 'NONE', #11647, #18350, #21043, .T. ) ;
#4541 = ORIENTED_EDGE ( 'NONE', *, *, #8957, .F. ) ;
#4542 = CIRCLE ( 'NONE', #28433, 30.47050528711511674 ) ;
#4543 = ADVANCED_FACE ( 'NONE', ( #12881 ), #13049, .F. ) ;
#4544 = DIRECTION ( 'NONE',  ( -0.1063910735369225230, 0.9943243633099118073, -1.000770725407345128E-14 ) ) ;
#4545 = ORIENTED_EDGE ( 'NONE', *, *, #10903, .T. ) ;
#4546 = CARTESIAN_POINT ( 'NONE',  ( 99.45057497126383339, -1.507735446164281790, 12.41434713890700969 ) ) ;
#4547 = ORIENTED_EDGE ( 'NONE', *, *, #19257, .T. ) ;
#4548 = FACE_OUTER_BOUND ( 'NONE', #26726, .T. ) ;
#4549 = EDGE_CURVE ( 'NONE', #7253, #9347, #147, .T. ) ;
#4550 = CARTESIAN_POINT ( 'NONE',  ( -365.0000000000000000, 134.9999999999999716, 113.9999999999999858 ) ) ;
#4551 = CARTESIAN_POINT ( 'NONE',  ( 1.341640786499872284, 1.738998454789241944E-15, -14.20000000000000107 ) ) ;
#4552 = AXIS2_PLACEMENT_3D ( 'NONE', #3614, #35028, #3436 ) ;
#4553 = PLANE ( 'NONE',  #27888 ) ;
#4554 = ORIENTED_EDGE ( 'NONE', *, *, #20693, .F. ) ;
#4555 = VERTEX_POINT ( 'NONE', #4832 ) ;
#4556 = EDGE_LOOP ( 'NONE', ( #25851, #5534, #27281, #33332, #4770, #18880, #25460, #30973 ) ) ;
#4557 = CARTESIAN_POINT ( 'NONE',  ( 1.040000000000000258, 28.00026196654270905, 20.00929742917132614 ) ) ;
#4558 = CARTESIAN_POINT ( 'NONE',  ( -5.021133111224989953, -3.725253662474303784, -67.50000000000000000 ) ) ;
#4559 = CARTESIAN_POINT ( 'NONE',  ( -414.0000000000000000, -105.0000000000000142, -77.99999999999997158 ) ) ;
#4560 = CARTESIAN_POINT ( 'NONE',  ( 29.82459402470852083, 33.69708579775584667, 87.50000000000000000 ) ) ;
#4561 = EDGE_CURVE ( 'NONE', #32547, #7170, #25532, .T. ) ;
#4562 = EDGE_CURVE ( 'NONE', #2950, #2759, #23291, .T. ) ;
#4563 = CARTESIAN_POINT ( 'NONE',  ( 10.00000000000000000, 9.797174393178825657E-16, -8.000000000000000000 ) ) ;
#4564 = PLANE ( 'NONE',  #3343 ) ;
#4565 = ORIENTED_EDGE ( 'NONE', *, *, #7900, .T. ) ;
#4566 = VECTOR ( 'NONE', #10233, 1000.000000000000000 ) ;
#4567 = FACE_OUTER_BOUND ( 'NONE', #29904, .T. ) ;
#4568 = CARTESIAN_POINT ( 'NONE',  ( 99.85824206759374988, 2.553994279224884423, 12.23746534924524632 ) ) ;
#4569 = VECTOR ( 'NONE', #28439, 1000.000000000000000 ) ;
#4570 = LINE ( 'NONE', #32173, #8080 ) ;
#4571 = VERTEX_POINT ( 'NONE', #32067 ) ;
#4572 = CARTESIAN_POINT ( 'NONE',  ( -42.55956070192386420, -17.65143121711728469, 0.000000000000000000 ) ) ;
#4573 = EDGE_LOOP ( 'NONE', ( #30707, #29959, #6658, #26541 ) ) ;
#4574 = DIRECTION ( 'NONE',  ( -1.000000000000000000, 6.792721752314501023E-48, -3.697785493223492838E-32 ) ) ;
#4575 = DIRECTION ( 'NONE',  ( -0.2149704402110236556, 0.9766205557100866574, 0.000000000000000000 ) ) ;
#4576 = FACE_OUTER_BOUND ( 'NONE', #1934, .T. ) ;
#4577 = TOROIDAL_SURFACE ( 'NONE', #1205, 30.47050528711512030, 8.000000000000000000 ) ;
#4578 = CARTESIAN_POINT ( 'NONE',  ( -12.00000000000001066, -105.0000000000000142, -154.9999999999999716 ) ) ;
#4579 = DIRECTION ( 'NONE',  ( -1.000000000000000000, 0.000000000000000000, -1.300283923313630633E-47 ) ) ;
#4580 = EDGE_LOOP ( 'NONE', ( #17912, #11755, #20585, #14999 ) ) ;
#4581 = EDGE_CURVE ( 'NONE', #31215, #10268, #15728, .T. ) ;
#4582 = EDGE_CURVE ( 'NONE', #22453, #23243, #1652, .T. ) ;
#4583 = ORIENTED_EDGE ( 'NONE', *, *, #32660, .T. ) ;
#4584 = CARTESIAN_POINT ( 'NONE',  ( 775.3643468492665534, 1165.252033389440612, 1753.598338701303419 ) ) ;
#4585 = VECTOR ( 'NONE', #19274, 1000.000000000000000 ) ;
#4586 = ORIENTED_EDGE ( 'NONE', *, *, #30932, .T. ) ;
#4587 = VECTOR ( 'NONE', #9875, 1000.000000000000000 ) ;
#4588 = CARTESIAN_POINT ( 'NONE',  ( -19.99999999999998934, -145.0000000000000000, 162.9999999999999716 ) ) ;
#4589 = CARTESIAN_POINT ( 'NONE',  ( 0.000000000000000000, 0.000000000000000000, 0.000000000000000000 ) ) ;
#4590 = DIRECTION ( 'NONE',  ( -0.000000000000000000, -1.836970198721029688E-16, 1.000000000000000000 ) ) ;
#4592 = EDGE_CURVE ( 'NONE', #27567, #27216, #23881, .T. ) ;
#4591 = ORIENTED_EDGE ( 'NONE', *, *, #23547, .F. ) ;
#4593 = CARTESIAN_POINT ( 'NONE',  ( 8.000000000000000000, 0.000000000000000000, 0.000000000000000000 ) ) ;
#4595 = CARTESIAN_POINT ( 'NONE',  ( 9.199999999999999289, 0.000000000000000000, 0.000000000000000000 ) ) ;
#4594 = CARTESIAN_POINT ( 'NONE',  ( -365.0000000000000000, 116.9999999999999716, 126.0000000000000000 ) ) ;
#4597 = ORIENTED_EDGE ( 'NONE', *, *, #8046, .F. ) ;
#4596 = AXIS2_PLACEMENT_3D ( 'NONE', #7824, #18708, #7285 ) ;
#4598 = VERTEX_POINT ( 'NONE', #5179 ) ;
#4599 = CARTESIAN_POINT ( 'NONE',  ( -5.344999999999999751, 1.414467053015192657E-16, 3.931000000000000494 ) ) ;
#4600 = CIRCLE ( 'NONE', #19406, 12.00000000000001066 ) ;
#4601 = VERTEX_POINT ( 'NONE', #34752 ) ;
#4602 = CIRCLE ( 'NONE', #30781, 34.41491905851385269 ) ;
#4603 = AXIS2_PLACEMENT_3D ( 'NONE', #10156, #2144, #23505 ) ;
#4604 = LINE ( 'NONE', #20659, #10217 ) ;
#4605 = CARTESIAN_POINT ( 'NONE',  ( 2.789999999999999147, -11.13185981125896795, 28.36429779836946352 ) ) ;
#4606 = VERTEX_POINT ( 'NONE', #26730 ) ;
#4607 = DIRECTION ( 'NONE',  ( 0.000000000000000000, 0.000000000000000000, -1.000000000000000000 ) ) ;
#4608 = VERTEX_POINT ( 'NONE', #34937 ) ;
#4609 = ADVANCED_FACE ( 'NONE', ( #7503 ), #10364, .T. ) ;
#4610 = CARTESIAN_POINT ( 'NONE',  ( -19.99999999999998934, -105.0000000000000142, 187.0000000000000000 ) ) ;
#4611 = DIRECTION ( 'NONE',  ( 0.000000000000000000, 0.000000000000000000, 1.000000000000000000 ) ) ;
#4612 = VECTOR ( 'NONE', #17082, 1000.000000000000000 ) ;
#4613 = CARTESIAN_POINT ( 'NONE',  ( -15.99999999999998579, -112.9999999999999858, 155.0000000000000000 ) ) ;
#4615 = DIRECTION ( 'NONE',  ( 1.000000000000000000, 0.000000000000000000, -0.000000000000000000 ) ) ;
#4614 = FACE_OUTER_BOUND ( 'NONE', #21775, .T. ) ;
#4616 =( REPRESENTATION_RELATIONSHIP ('NONE','NONE', #23037, #15767 ) REPRESENTATION_RELATIONSHIP_WITH_TRANSFORMATION ( #32199 )SHAPE_REPRESENTATION_RELATIONSHIP( ) );
#4617 = LINE ( 'NONE', #7126, #12199 ) ;
#4618 = CARTESIAN_POINT ( 'NONE',  ( 1.205771365940050410, 15.58845726811990495, 1.140844902514640588E-16 ) ) ;
#4619 = DIRECTION ( 'NONE',  ( -1.000000000000000000, -0.000000000000000000, -0.000000000000000000 ) ) ;
#4620 = DIRECTION ( 'NONE',  ( 0.000000000000000000, 1.836970198721029688E-16, -1.000000000000000000 ) ) ;
#4621 = PRODUCT_DEFINITION_SHAPE ( 'NONE', 'NONE',  #35182 ) ;
#4622 = ADVANCED_FACE ( 'NONE', ( #15540 ), #15909, .T. ) ;
#4623 = EDGE_CURVE ( 'NONE', #23243, #30812, #17619, .T. ) ;
#4624 = COLOUR_RGB ( '',0.7921568627450980005, 0.8196078431372548767, 0.9333333333333333481 ) ;
#4625 = EDGE_CURVE ( 'NONE', #26014, #11706, #2343, .T. ) ;
#4626 = VERTEX_POINT ( 'NONE', #26381 ) ;
#4627 = AXIS2_PLACEMENT_3D ( 'NONE', #33035, #22196, #11173 ) ;
#4628 = VECTOR ( 'NONE', #23985, 1000.000000000000000 ) ;
#4629 = AXIS2_PLACEMENT_3D ( 'NONE', #12094, #22590, #33433 ) ;
#4630 = VECTOR ( 'NONE', #18717, 1000.000000000000000 ) ;
#4631 = EDGE_LOOP ( 'NONE', ( #28245, #8824, #2541, #6678 ) ) ;
#4632 = ORIENTED_EDGE ( 'NONE', *, *, #9637, .T. ) ;
#4633 = FACE_OUTER_BOUND ( 'NONE', #20108, .T. ) ;
#4634 = CARTESIAN_POINT ( 'NONE',  ( 0.000000000000000000, 0.000000000000000000, 0.000000000000000000 ) ) ;
#4635 = ORIENTED_EDGE ( 'NONE', *, *, #23749, .F. ) ;
#4636 = ORIENTED_EDGE ( 'NONE', *, *, #4357, .T. ) ;
#4637 = ORIENTED_EDGE ( 'NONE', *, *, #10693, .F. ) ;
#4638 = DIRECTION ( 'NONE',  ( -0.9635499925192227977, -0.2675283385292216987, -4.914415851915313010E-17 ) ) ;
#4639 = ITEM_DEFINED_TRANSFORMATION ( 'NONE', 'NONE', #6471,  #28566 ) ;
#4640 = VERTEX_POINT ( 'NONE', #31548 ) ;
#4641 = CARTESIAN_POINT ( 'NONE',  ( -70.00000000000000000, 4.559999999999908127, 168.2400000000000091 ) ) ;
#4642 = DIRECTION ( 'NONE',  ( 1.000000000000000000, 0.000000000000000000, 0.000000000000000000 ) ) ;
#4643 = ORIENTED_EDGE ( 'NONE', *, *, #8513, .T. ) ;
#4644 = ORIENTED_EDGE ( 'NONE', *, *, #21449, .F. ) ;
#4645 = CARTESIAN_POINT ( 'NONE',  ( 0.02407890056655781832, 4.286445725888479608, -30.79383171238939809 ) ) ;
#4646 = PLANE ( 'NONE',  #12993 ) ;
#4647 = DIRECTION ( 'NONE',  ( -1.000000000000000000, 0.000000000000000000, -1.300283923313630633E-47 ) ) ;
#4648 = CARTESIAN_POINT ( 'NONE',  ( -0.7181323043387224381, -1.866624223957557893, -0.7500000000000000000 ) ) ;
#4649 = CARTESIAN_POINT ( 'NONE',  ( 5.021133111224162171, -21.54630831098063481, -87.50000000000000000 ) ) ;
#4650 = EDGE_LOOP ( 'NONE', ( #32477, #31030, #19102, #11073 ) ) ;
#4651 = VECTOR ( 'NONE', #18769, 1000.000000000000000 ) ;
#4652 = FACE_OUTER_BOUND ( 'NONE', #16681, .T. ) ;
#4653 = CARTESIAN_POINT ( 'NONE',  ( -47.73029880539744596, 11.89540832764809508, 29.51713323100467434 ) ) ;
#4654 = CIRCLE ( 'NONE', #21723, 32.54542015209056416 ) ;
#4655 = ORIENTED_EDGE ( 'NONE', *, *, #31078, .F. ) ;
#4656 = AXIS2_PLACEMENT_3D ( 'NONE', #22342, #8808, #10646 ) ;
#4657 = CARTESIAN_POINT ( 'NONE',  ( -347.0000000000000000, 124.9999999999999432, 181.0000000000000000 ) ) ;
#4658 = DIRECTION ( 'NONE',  ( 0.000000000000000000, 2.309213040847544338E-50, 1.000000000000000000 ) ) ;
#4659 = DIRECTION ( 'NONE',  ( 0.000000000000000000, 1.131431318426415506E-52, 1.000000000000000000 ) ) ;
#4661 = CARTESIAN_POINT ( 'NONE',  ( -109.9413161124788445, 1.365406536427363315, -7.382450522560829675 ) ) ;
#4660 = DIRECTION ( 'NONE',  ( -1.000000000000000000, 0.000000000000000000, 0.000000000000000000 ) ) ;
#4662 = EDGE_CURVE ( 'NONE', #10319, #4812, #22712, .T. ) ;
#4663 = DIRECTION ( 'NONE',  ( 0.000000000000000000, 1.836970198721029441E-16, -1.000000000000000000 ) ) ;
#4664 = ORIENTED_EDGE ( 'NONE', *, *, #22172, .F. ) ;
#4665 = CARTESIAN_POINT ( 'NONE',  ( 109.5543437205592170, 3.510468032099188118, -12.00123740321143728 ) ) ;
#4667 = PLANE ( 'NONE',  #15751 ) ;
#4666 = CARTESIAN_POINT ( 'NONE',  ( -12.00000000000001066, -24.99999999999999289, -175.0000000000000000 ) ) ;
#4668 = EDGE_CURVE ( 'NONE', #9316, #28134, #26201, .T. ) ;
#4669 = EDGE_CURVE ( 'NONE', #16394, #14153, #12022, .T. ) ;
#4670 = ORIENTED_EDGE ( 'NONE', *, *, #28427, .T. ) ;
#4671 = DIRECTION ( 'NONE',  ( -1.000000000000000000, 6.792721752314501023E-48, -3.697785493223492838E-32 ) ) ;
#4672 = EDGE_CURVE ( 'NONE', #16780, #8132, #23267, .T. ) ;
#4673 = ORIENTED_EDGE ( 'NONE', *, *, #5133, .F. ) ;
#4674 = AXIS2_PLACEMENT_3D ( 'NONE', #34730, #24032, #13206 ) ;
#4675 = VECTOR ( 'NONE', #25431, 1000.000000000000000 ) ;
#4676=STYLED_ITEM('',(#35275),#34055);
#4677 = AXIS2_PLACEMENT_3D ( 'NONE', #23089, #12062, #4011 ) ;
#4678 = ORIENTED_EDGE ( 'NONE', *, *, #12906, .T. ) ;
#4679 = CARTESIAN_POINT ( 'NONE',  ( -365.0000000000000000, 130.9999999999999716, 130.0000000000000000 ) ) ;
#4680 = ORIENTED_EDGE ( 'NONE', *, *, #12361, .F. ) ;
#4681 = VERTEX_POINT ( 'NONE', #16603 ) ;
#4682 = CARTESIAN_POINT ( 'NONE',  ( 2.765921099433442443, 28.29688452313417812, -12.88099432405573630 ) ) ;
#4683 = EDGE_CURVE ( 'NONE', #28732, #18315, #21742, .T. ) ;
#4684 = DIRECTION ( 'NONE',  ( -0.1452892791026231256, -0.5232846903699686081, 0.8396809859716046764 ) ) ;
#4685 = DIRECTION ( 'NONE',  ( 0.000000000000000000, -1.000000000000000000, 0.000000000000000000 ) ) ;
#4686 = ORIENTED_EDGE ( 'NONE', *, *, #27186, .F. ) ;
#4687 = ORIENTED_EDGE ( 'NONE', *, *, #12173, .F. ) ;
#4688 = PLANE ( 'NONE',  #33896 ) ;
#4689 = CARTESIAN_POINT ( 'NONE',  ( -430.0000000000000000, 116.9999999999999858, 126.0000000000000000 ) ) ;
#4690 = CARTESIAN_POINT ( 'NONE',  ( -35.00000000000000000, 16.36947364650383818, -36.69637551990492597 ) ) ;
#4691 = LINE ( 'NONE', #2219, #17594 ) ;
#4692 = LINE ( 'NONE', #17927, #32446 ) ;
#4693 = ORIENTED_EDGE ( 'NONE', *, *, #4299, .T. ) ;
#4694 = ORIENTED_EDGE ( 'NONE', *, *, #1294, .F. ) ;
#4695 = CARTESIAN_POINT ( 'NONE',  ( 2.789999999999999147, 30.40449935640660684, 2.004522720844263084 ) ) ;
#4696 = AXIS2_PLACEMENT_3D ( 'NONE', #3279, #11480, #10779 ) ;
#4697 = CARTESIAN_POINT ( 'NONE',  ( 0.02407890056655868569, -17.95514392185398833, -25.38201125280375692 ) ) ;
#4698 = ORIENTED_EDGE ( 'NONE', *, *, #21804, .T. ) ;
#4699 = LINE ( 'NONE', #2747, #20213 ) ;
#4700 = CYLINDRICAL_SURFACE ( 'NONE', #7480, 16.19999999999999574 ) ;
#4701 = FACE_OUTER_BOUND ( 'NONE', #21536, .T. ) ;
#4702 = ORIENTED_EDGE ( 'NONE', *, *, #22566, .T. ) ;
#4703 = AXIS2_PLACEMENT_3D ( 'NONE', #18337, #13507, #35052 ) ;
#4704 = DIRECTION ( 'NONE',  ( 0.000000000000000000, 0.000000000000000000, -1.000000000000000000 ) ) ;
#4705 = VERTEX_POINT ( 'NONE', #3223 ) ;
#4706 = VECTOR ( 'NONE', #32700, 1000.000000000000000 ) ;
#4707 = MECHANICAL_DESIGN_GEOMETRIC_PRESENTATION_REPRESENTATION (  '', ( #9832 ), #31919 ) ;
#4708 = CIRCLE ( 'NONE', #24603, 30.47050528711512030 ) ;
#4709 = DIRECTION ( 'NONE',  ( 0.000000000000000000, -7.888609052210118054E-31, -1.000000000000000000 ) ) ;
#4710 = ORIENTED_EDGE ( 'NONE', *, *, #14205, .F. ) ;
#4711 = DIRECTION ( 'NONE',  ( 6.189473249308360462E-17, 0.000000000000000000, -1.000000000000000000 ) ) ;
#4712 = CARTESIAN_POINT ( 'NONE',  ( 0.006871066268349140978, 23.98851302352036186, 19.42881381898178716 ) ) ;
#4713 = B_SPLINE_CURVE_WITH_KNOTS ( 'NONE', 3,
 ( #19285, #21592, #24590, #2540 ),
 .UNSPECIFIED., .F., .F.,
 ( 4, 4 ),
 ( 0.005298347253562320572, 0.005985215922708605162 ),
 .UNSPECIFIED. ) ;
#4714 = ORIENTED_EDGE ( 'NONE', *, *, #4625, .T. ) ;
#4715 = CARTESIAN_POINT ( 'NONE',  ( -442.0000000000000000, -125.0000000000000000, 107.9999999999999858 ) ) ;
#4716 = DIRECTION ( 'NONE',  ( -1.000000000000000000, -0.000000000000000000, -0.000000000000000000 ) ) ;
#4717 = EDGE_CURVE ( 'NONE', #28240, #29230, #22278, .T. ) ;
#4718 = ADVANCED_FACE ( 'NONE', ( #33123 ), #213, .T. ) ;
#4719 = ORIENTED_EDGE ( 'NONE', *, *, #20729, .T. ) ;
#4720 = AXIS2_PLACEMENT_3D ( 'NONE', #3623, #11846, #31049 ) ;
#4721 = ADVANCED_FACE ( 'NONE', ( #16429 ), #13741, .T. ) ;
#4722 = EDGE_CURVE ( 'NONE', #5918, #31132, #24385, .T. ) ;
#4723 = CARTESIAN_POINT ( 'NONE',  ( 763.6081396259702387, 1275.124815697498434, 1753.598338701303419 ) ) ;
#4724 = ORIENTED_EDGE ( 'NONE', *, *, #28459, .T. ) ;
#4725 = DIRECTION ( 'NONE',  ( 0.000000000000000000, 1.000000000000000000, -6.123233995736766036E-17 ) ) ;
#4726 = ORIENTED_EDGE ( 'NONE', *, *, #30913, .T. ) ;
#4727 = DIRECTION ( 'NONE',  ( 1.000000000000000000, 0.000000000000000000, 0.000000000000000000 ) ) ;
#4728 = AXIS2_PLACEMENT_3D ( 'NONE', #13038, #34736, #24037 ) ;
#4729 = DIRECTION ( 'NONE',  ( -1.000000000000000000, 0.000000000000000000, 0.000000000000000000 ) ) ;
#4730 = CIRCLE ( 'NONE', #1361, 1.649999999999999911 ) ;
#4731 = CARTESIAN_POINT ( 'NONE',  ( -100.3602415740146228, -2.159755022470677854, -7.184107906894083406 ) ) ;
#4732 = CARTESIAN_POINT ( 'NONE',  ( -355.0000000000000000, -119.0000000000000000, 111.9999999999999858 ) ) ;
#4733 = ITEM_DEFINED_TRANSFORMATION ( 'NONE', 'NONE', #3594,  #28566 ) ;
#4734 = ORIENTED_EDGE ( 'NONE', *, *, #6971, .T. ) ;
#4735 = ORIENTED_EDGE ( 'NONE', *, *, #30501, .T. ) ;
#4736 = AXIS2_PLACEMENT_3D ( 'NONE', #34364, #31343, #20839 ) ;
#4737 = PRODUCT_DEFINITION_SHAPE ( 'NONE', 'NONE',  #35220 ) ;
#4738 = ORIENTED_EDGE ( 'NONE', *, *, #27574, .T. ) ;
#4739 = DIRECTION ( 'NONE',  ( 0.000000000000000000, 1.000000000000000000, 0.000000000000000000 ) ) ;
#4740 = EDGE_CURVE ( 'NONE', #29809, #23630, #11916, .T. ) ;
#4741 = CARTESIAN_POINT ( 'NONE',  ( 0.000000000000000000, -3.728217946243090886, 30.24156218513556738 ) ) ;
#4742 = CARTESIAN_POINT ( 'NONE',  ( 31.73435513276359643, 7.220462394039750542, 68.31122994652405112 ) ) ;
#4743 = FACE_OUTER_BOUND ( 'NONE', #27107, .T. ) ;
#4744 = DIRECTION ( 'NONE',  ( 0.000000000000000000, -1.000000000000000000, -2.465190328815662439E-32 ) ) ;
#4745 = CARTESIAN_POINT ( 'NONE',  ( -19.99999999999998934, 112.9999999999999574, -175.0000000000000284 ) ) ;
#4746 = EDGE_LOOP ( 'NONE', ( #5289, #375, #12548, #2256 ) ) ;
#4747 = DIRECTION ( 'NONE',  ( 0.000000000000000000, 1.000000000000000000, 0.000000000000000000 ) ) ;
#4748 = CARTESIAN_POINT ( 'NONE',  ( 99.26191511054629757, 0.3793982372081725063, 12.50000000000000000 ) ) ;
#4749 = CYLINDRICAL_SURFACE ( 'NONE', #23978, 4.682234377621698584 ) ;
#4751 = EDGE_CURVE ( 'NONE', #4890, #29871, #30279, .T. ) ;
#4750 = ORIENTED_EDGE ( 'NONE', *, *, #29800, .F. ) ;
#4752 = EDGE_CURVE ( 'NONE', #22681, #8703, #30675, .T. ) ;
#4753 = CARTESIAN_POINT ( 'NONE',  ( 0.8394537150704712847, -6.525267068029305229, -13.49999999999999822 ) ) ;
#4754 = ORIENTED_EDGE ( 'NONE', *, *, #20666, .T. ) ;
#4755 = LINE ( 'NONE', #23647, #20022 ) ;
#4756 = DIRECTION ( 'NONE',  ( 1.000000000000000000, 0.000000000000000000, 0.000000000000000000 ) ) ;
#4757 = AXIS2_PLACEMENT_3D ( 'NONE', #31790, #13117, #35008 ) ;
#4758 = VECTOR ( 'NONE', #12896, 1000.000000000000000 ) ;
#4759 = ORIENTED_EDGE ( 'NONE', *, *, #20854, .F. ) ;
#4760 = AXIS2_PLACEMENT_3D ( 'NONE', #27845, #28205, #9518 ) ;
#4761 = CYLINDRICAL_SURFACE ( 'NONE', #10882, 2.525000000000001243 ) ;
#4762 = DIRECTION ( 'NONE',  ( 0.5155538571770220679, 0.8568571761675890519, 0.000000000000000000 ) ) ;
#4763 = LINE ( 'NONE', #23652, #8632 ) ;
#4764 = VECTOR ( 'NONE', #18171, 1000.000000000000000 ) ;
#4765 = ORIENTED_EDGE ( 'NONE', *, *, #31959, .T. ) ;
#4766 = VERTEX_POINT ( 'NONE', #11076 ) ;
#4767 = EDGE_CURVE ( 'NONE', #33660, #29323, #566, .T. ) ;
#4768 = ADVANCED_FACE ( 'NONE', ( #30108 ), #31728, .T. ) ;
#4769 = DIRECTION ( 'NONE',  ( -0.1063910735369017202, 0.9943243633099136947, -1.000770725407181676E-14 ) ) ;
#4770 = ORIENTED_EDGE ( 'NONE', *, *, #25156, .F. ) ;
#4771 = ADVANCED_FACE ( 'NONE', ( #32417, #29758 ), #2699, .T. ) ;
#4772 = DIRECTION ( 'NONE',  ( -1.000000000000000000, 0.000000000000000000, 1.848892746611746966E-32 ) ) ;
#4773 = VECTOR ( 'NONE', #4727, 1000.000000000000000 ) ;
#4774 = LINE ( 'NONE', #5127, #7617 ) ;
#4775 = CARTESIAN_POINT ( 'NONE',  ( 100.4825637827005238, -3.557362730766958858, 6.611294427798556583 ) ) ;
#4776 = VERTEX_POINT ( 'NONE', #8562 ) ;
#4777 = DIRECTION ( 'NONE',  ( 1.000000000000000000, 0.000000000000000000, 0.000000000000000000 ) ) ;
#4778 = AXIS2_PLACEMENT_3D ( 'NONE', #31836, #9623, #31498 ) ;
#4779 = DIRECTION ( 'NONE',  ( 5.546364386991661285E-52, 0.000000000000000000, -1.000000000000000000 ) ) ;
#4781 = DIRECTION ( 'NONE',  ( 0.000000000000000000, 1.000000000000000000, 0.000000000000000000 ) ) ;
#4780 = LINE ( 'NONE', #34888, #5369 ) ;
#4782 = CIRCLE ( 'NONE', #820, 3.999999999999976019 ) ;
#4783 = ORIENTED_EDGE ( 'NONE', *, *, #34768, .F. ) ;
#4784 = ORIENTED_EDGE ( 'NONE', *, *, #16537, .T. ) ;
#4785 = AXIS2_PLACEMENT_3D ( 'NONE', #33326, #11812, #11979 ) ;
#4786 = CARTESIAN_POINT ( 'NONE',  ( 1.749999999999999778, -30.28730148581149706, -16.34215476954067015 ) ) ;
#4787 = ORIENTED_EDGE ( 'NONE', *, *, #277, .T. ) ;
#4788 = EDGE_CURVE ( 'NONE', #25489, #15525, #27437, .T. ) ;
#4789 = LINE ( 'NONE', #7644, #33510 ) ;
#4790 = DIRECTION ( 'NONE',  ( -1.000000000000000000, 0.000000000000000000, -0.000000000000000000 ) ) ;
#4791 = ORIENTED_EDGE ( 'NONE', *, *, #19067, .T. ) ;
#4792 = EDGE_CURVE ( 'NONE', #14584, #14420, #32, .T. ) ;
#4793 = EDGE_CURVE ( 'NONE', #10803, #2924, #9006, .T. ) ;
#4794 = CARTESIAN_POINT ( 'NONE',  ( -499.9999999999999432, 140.9999999999999716, 162.9999999999999716 ) ) ;
#4795 = ORIENTED_EDGE ( 'NONE', *, *, #2849, .F. ) ;
#4796 = FACE_OUTER_BOUND ( 'NONE', #19514, .T. ) ;
#4797 = DIRECTION ( 'NONE',  ( -1.000000000000000000, 0.000000000000000000, 0.000000000000000000 ) ) ;
#4798 = EDGE_CURVE ( 'NONE', #26810, #3104, #397, .T. ) ;
#4799 = CARTESIAN_POINT ( 'NONE',  ( 5.127716880498843092E-16, 30.15879770317936348, -5.529954278609071849 ) ) ;
#4801 = CARTESIAN_POINT ( 'NONE',  ( 11.99999999999999645, 134.9999999999999432, -194.9999999999999432 ) ) ;
#4800 = CARTESIAN_POINT ( 'NONE',  ( 0.1859802911799672831, -32.25918669212988021, -1.206152977788097713 ) ) ;
#4802 = AXIS2_PLACEMENT_3D ( 'NONE', #18777, #15757, #8072 ) ;
#4803 = EDGE_CURVE ( 'NONE', #4465, #21456, #4810, .T. ) ;
#4805 = ADVANCED_FACE ( 'NONE', ( #19796 ), #30815, .T. ) ;
#4804 = CARTESIAN_POINT ( 'NONE',  ( -20.00000000000007461, 108.9999999999999858, 162.9999999999999716 ) ) ;
#4806 = CARTESIAN_POINT ( 'NONE',  ( 212.5000000000000000, 0.000000000000000000, 0.000000000000000000 ) ) ;
#4807 = LINE ( 'NONE', #23341, #1955 ) ;
#4808 = DIRECTION ( 'NONE',  ( -1.000000000000000000, -0.000000000000000000, -0.000000000000000000 ) ) ;
#4809 = VECTOR ( 'NONE', #8695, 1000.000000000000000 ) ;
#4810 = CIRCLE ( 'NONE', #28891, 4.750000000000004441 ) ;
#4812 = VERTEX_POINT ( 'NONE', #22807 ) ;
#4811 = AXIS2_PLACEMENT_3D ( 'NONE', #7297, #21378, #2972 ) ;
#4813 = AXIS2_PLACEMENT_3D ( 'NONE', #3547, #25262, #897 ) ;
#4814 = DIRECTION ( 'NONE',  ( 0.1063910735368947813, -0.9943243633099144718, -3.335902418024520312E-15 ) ) ;
#4815 = ORIENTED_EDGE ( 'NONE', *, *, #7136, .T. ) ;
#4816 = CLOSED_SHELL ( 'NONE', ( #15483, #17690, #8395, #26969, #9679, #14570, #11624, #26790, #13248, #11276, #29983, #23696, #11103, #2010, #4245, #17829, #16493, #17504 ) ) ;
#4817 = ORIENTED_EDGE ( 'NONE', *, *, #1873, .F. ) ;
#4818 = CARTESIAN_POINT ( 'NONE',  ( 0.000000000000000000, 25.67797970382157402, -16.40405592474731833 ) ) ;
#4819 = ORIENTED_EDGE ( 'NONE', *, *, #29048, .F. ) ;
#4820 = ORIENTED_EDGE ( 'NONE', *, *, #31504, .F. ) ;
#4821 = CARTESIAN_POINT ( 'NONE',  ( 0.000000000000000000, 20.79173593595263370, 22.27454621808773538 ) ) ;
#4822 = CARTESIAN_POINT ( 'NONE',  ( 0.02407890056655911937, -15.32140196853734970, -27.05343472113007763 ) ) ;
#4823 = CONTEXT_DEPENDENT_SHAPE_REPRESENTATION ( #16516, #3686 ) ;
#4824 = CARTESIAN_POINT ( 'NONE',  ( 2.789999999999999147, -11.07880054387241664, 29.04985141099759360 ) ) ;
#4825 = CARTESIAN_POINT ( 'NONE',  ( -10.00000000000000000, 0.000000000000000000, 0.000000000000000000 ) ) ;
#4826 = ORIENTED_EDGE ( 'NONE', *, *, #24296, .T. ) ;
#4827 = VERTEX_POINT ( 'NONE', #22983 ) ;
#4828 = LINE ( 'NONE', #29410, #9479 ) ;
#4829 = VECTOR ( 'NONE', #14017, 1000.000000000000000 ) ;
#4830 = CARTESIAN_POINT ( 'NONE',  ( 0.02407890056655695096, 26.03801215795542134, -16.98986790278583570 ) ) ;
#4831 = CIRCLE ( 'NONE', #35001, 3.999999999999976019 ) ;
#4832 = CARTESIAN_POINT ( 'NONE',  ( -30.58418286738120884, -22.31615353445078043, -36.68877005347593467 ) ) ;
#4833 = DIRECTION ( 'NONE',  ( 1.000000000000000000, 0.000000000000000000, 0.000000000000000000 ) ) ;
#4834 = CARTESIAN_POINT ( 'NONE',  ( -442.0000000000000000, -125.0000000000000000, 104.0000000000000142 ) ) ;
#4835 = ORIENTED_EDGE ( 'NONE', *, *, #5450, .T. ) ;
#4836 = EDGE_CURVE ( 'NONE', #23446, #5845, #28346, .T. ) ;
#4837 = CARTESIAN_POINT ( 'NONE',  ( 9.199999999999999289, 13.50000000000000178, 0.000000000000000000 ) ) ;
#4838 = DIRECTION ( 'NONE',  ( -0.000000000000000000, 0.000000000000000000, 1.000000000000000000 ) ) ;
#4839 = ADVANCED_FACE ( 'NONE', ( #6412 ), #28143, .F. ) ;
#4840 = AXIS2_PLACEMENT_3D ( 'NONE', #25035, #9210, #3855 ) ;
#4841 = APPLICATION_CONTEXT ( 'automotive_design' ) ;
#4842 = AXIS2_PLACEMENT_3D ( 'NONE', #1681, #17911, #12549 ) ;
#4843 = CIRCLE ( 'NONE', #1461, 7.500000000000000000 ) ;
#4844 = CYLINDRICAL_SURFACE ( 'NONE', #6075, 5.115020388170798959 ) ;
#4845 = DIRECTION ( 'NONE',  ( -1.000000000000000000, -0.000000000000000000, 0.000000000000000000 ) ) ;
#4846 = DIRECTION ( 'NONE',  ( -1.000000000000000000, -3.040835319149746090E-31, 1.232595164407830946E-32 ) ) ;
#4848 = FACE_OUTER_BOUND ( 'NONE', #18990, .T. ) ;
#4847 = CARTESIAN_POINT ( 'NONE',  ( -145.0000000000000568, -90.42893218813456713, 44.81798139211241505 ) ) ;
#4849 = DIRECTION ( 'NONE',  ( 1.000000000000000000, -0.000000000000000000, -0.000000000000000000 ) ) ;
#4850 = VERTEX_POINT ( 'NONE', #4088 ) ;
#4851 = CARTESIAN_POINT ( 'NONE',  ( 100.0299053779175580, 2.891935069322401297, -12.16509469334830307 ) ) ;
#4853 = LINE ( 'NONE', #31907, #26523 ) ;
#4852 = DIRECTION ( 'NONE',  ( 0.000000000000000000, 0.000000000000000000, -1.000000000000000000 ) ) ;
#4854 = VECTOR ( 'NONE', #33919, 1000.000000000000227 ) ;
#4855 = ORIENTED_EDGE ( 'NONE', *, *, #28938, .F. ) ;
#4856 = CARTESIAN_POINT ( 'NONE',  ( -28.23027531293552528, -10.15143121711728469, 20.00000000000000000 ) ) ;
#4857 = AXIS2_PLACEMENT_3D ( 'NONE', #30327, #19488, #16298 ) ;
#4858 = EDGE_LOOP ( 'NONE', ( #34273, #30610, #6487, #7399, #16364, #19702 ) ) ;
#4859 = ORIENTED_EDGE ( 'NONE', *, *, #31267, .F. ) ;
#4860 = CARTESIAN_POINT ( 'NONE',  ( -0.9727285265192158192, -1.747512292859697114, 3.180000000000000160 ) ) ;
#4861 = EDGE_LOOP ( 'NONE', ( #12941, #33600, #3787, #3261, #11105, #7387 ) ) ;
#4862 = ORIENTED_EDGE ( 'NONE', *, *, #14813, .T. ) ;
#4863 = CARTESIAN_POINT ( 'NONE',  ( 19.99999999999998224, 112.9999999999999574, -155.0000000000000000 ) ) ;
#4864 = VECTOR ( 'NONE', #34907, 1000.000000000000000 ) ;
#4865 = CARTESIAN_POINT ( 'NONE',  ( -499.9999999999999432, 112.9999999999999574, -162.9999999999999716 ) ) ;
#4866 = CARTESIAN_POINT ( 'NONE',  ( 0.000000000000000000, 0.000000000000000000, 0.000000000000000000 ) ) ;
#4867 = VERTEX_POINT ( 'NONE', #3919 ) ;
#4868 = EDGE_LOOP ( 'NONE', ( #29614, #34580, #26910, #1631 ) ) ;
#4869 = CARTESIAN_POINT ( 'NONE',  ( 22.89764159710611224, 15.60017778382161246, -77.50000000000000000 ) ) ;
#4870 = DIRECTION ( 'NONE',  ( 0.7259954919231307313, -0.6876994588534234287, -0.000000000000000000 ) ) ;
#4871 = DIRECTION ( 'NONE',  ( -1.000000000000000000, -0.000000000000000000, -0.000000000000000000 ) ) ;
#4872 = EDGE_CURVE ( 'NONE', #24340, #8764, #22637, .T. ) ;
#4873 = PLANE ( 'NONE',  #24965 ) ;
#4874 = CARTESIAN_POINT ( 'NONE',  ( -430.0000000000000000, 130.9999999999999716, 113.9999999999999858 ) ) ;
#4875 = UNCERTAINTY_MEASURE_WITH_UNIT (LENGTH_MEASURE( 1.000000000000000082E-05 ), #13910, 'distance_accuracy_value', 'NONE');
#4876 = EDGE_LOOP ( 'NONE', ( #28780, #33434, #12387, #9377 ) ) ;
#4877 = CIRCLE ( 'NONE', #28201, 1.154999999999999805 ) ;
#4878 = DIRECTION ( 'NONE',  ( 0.1378075576670459712, -0.8405889147755769564, -0.5238505067347569710 ) ) ;
#4879 = ADVANCED_FACE ( 'NONE', ( #3398 ), #11963, .T. ) ;
#4880 = CARTESIAN_POINT ( 'NONE',  ( 22.89764159710611224, 15.60017778382161246, -77.50000000000000000 ) ) ;
#4881 = EDGE_LOOP ( 'NONE', ( #15001, #7925, #11194, #15897, #26891, #20999, #12021, #554 ) ) ;
#4882 = EDGE_CURVE ( 'NONE', #20393, #32015, #7352, .T. ) ;
#4883 = B_SPLINE_CURVE_WITH_KNOTS ( 'NONE', 3,
 ( #30092, #29920, #2683, #27065 ),
 .UNSPECIFIED., .F., .F.,
 ( 4, 4 ),
 ( 4.404817005620765685E-07, 0.001749480761540356689 ),
 .UNSPECIFIED. ) ;
#4884 = AXIS2_PLACEMENT_3D ( 'NONE', #10644, #13141, #23974 ) ;
#4885 = DIRECTION ( 'NONE',  ( -0.000000000000000000, 1.836970198721029688E-16, -1.000000000000000000 ) ) ;
#4886 = DIRECTION ( 'NONE',  ( 0.000000000000000000, -1.000000000000000000, -2.132064625830773463E-16 ) ) ;
#4887 = CARTESIAN_POINT ( 'NONE',  ( -5.038454199367317976, -32.15304576796696523, 68.31122994652405112 ) ) ;
#4888 = ORIENTED_EDGE ( 'NONE', *, *, #5873, .T. ) ;
#4889 = DIRECTION ( 'NONE',  ( 0.9289767198167918627, 0.3701381553399134550, 6.799327607689963350E-17 ) ) ;
#4890 = VERTEX_POINT ( 'NONE', #9276 ) ;
#4891 =( REPRESENTATION_RELATIONSHIP ('NONE','NONE', #23037, #28231 ) REPRESENTATION_RELATIONSHIP_WITH_TRANSFORMATION ( #3949 )SHAPE_REPRESENTATION_RELATIONSHIP( ) );
#4892 = CARTESIAN_POINT ( 'NONE',  ( -12.00000000000001066, -145.0000000000000000, -162.9999999999999432 ) ) ;
#4893 = EDGE_LOOP ( 'NONE', ( #17206, #26632 ) ) ;
#4895 = DIRECTION ( 'NONE',  ( -0.000000000000000000, 1.836970198721029934E-16, -1.000000000000000000 ) ) ;
#4894 =( NAMED_UNIT ( * ) SI_UNIT ( $, .STERADIAN. ) SOLID_ANGLE_UNIT ( ) );
#4897 = AXIS2_PLACEMENT_3D ( 'NONE', #13196, #32039, #19070 ) ;
#4896 = FACE_OUTER_BOUND ( 'NONE', #5351, .T. ) ;
#4898 = ORIENTED_EDGE ( 'NONE', *, *, #26687, .T. ) ;
#4899 = DIRECTION ( 'NONE',  ( -0.000000000000000000, -0.000000000000000000, -1.000000000000000000 ) ) ;
#4900 = CARTESIAN_POINT ( 'NONE',  ( 0.000000000000000000, 33.69708579775584667, 49.43553178847298568 ) ) ;
#4901 = ORIENTED_EDGE ( 'NONE', *, *, #15315, .T. ) ;
#4902 = VECTOR ( 'NONE', #30465, 1000.000000000000227 ) ;
#4903 = CARTESIAN_POINT ( 'NONE',  ( 759.4588900177482174, 1313.903444747400954, 1753.598338701303419 ) ) ;
#4904 = ORIENTED_EDGE ( 'NONE', *, *, #31270, .F. ) ;
#4905 = CARTESIAN_POINT ( 'NONE',  ( 110.4382027763065963, -1.869077253746796341, 12.36451290817386450 ) ) ;
#4906 = ORIENTED_EDGE ( 'NONE', *, *, #13949, .T. ) ;
#4907 = AXIS2_PLACEMENT_3D ( 'NONE', #20412, #12059, #23256 ) ;
#4908 = CYLINDRICAL_SURFACE ( 'NONE', #9349, 2.033421858999711507 ) ;
#4909 = CARTESIAN_POINT ( 'NONE',  ( 2.783107618804362193, 30.78707849925352136, -2.258378142202823735 ) ) ;
#4910 = CARTESIAN_POINT ( 'NONE',  ( -109.8286890707746011, -1.696008709688487048, -7.307621933264762504 ) ) ;
#4911 = CARTESIAN_POINT ( 'NONE',  ( 2.790000000000000924, 12.80000000000000071, -3.000000000000000000 ) ) ;
#4912 = ITEM_DEFINED_TRANSFORMATION ( 'NONE', 'NONE', #26898,  #28566 ) ;
#4913 = ORIENTED_EDGE ( 'NONE', *, *, #34504, .F. ) ;
#4914 = EDGE_LOOP ( 'NONE', ( #7192, #16179, #12089, #27858 ) ) ;
#4915 = ORIENTED_EDGE ( 'NONE', *, *, #26478, .T. ) ;
#4916 = CARTESIAN_POINT ( 'NONE',  ( -499.9999999999999432, 112.9999999999999574, 187.0000000000000000 ) ) ;
#4917 = DIRECTION ( 'NONE',  ( 0.000000000000000000, 0.000000000000000000, 1.000000000000000000 ) ) ;
#4918 = CIRCLE ( 'NONE', #12320, 2.524999999999999467 ) ;
#4919 = ADVANCED_FACE ( 'NONE', ( #25818 ), #17314, .F. ) ;
#4920 = CARTESIAN_POINT ( 'NONE',  ( 143.0000000000000568, -97.49999999999998579, 51.88904920397793319 ) ) ;
#4921 = FACE_OUTER_BOUND ( 'NONE', #13858, .T. ) ;
#4922 = CARTESIAN_POINT ( 'NONE',  ( 11.99999999999999645, 144.9999999999999716, -194.9999999999999432 ) ) ;
#4923 = DIRECTION ( 'NONE',  ( 0.000000000000000000, -7.888609052210118054E-31, -1.000000000000000000 ) ) ;
#4924 = CARTESIAN_POINT ( 'NONE',  ( 2.789999999999999147, 25.67797970382158113, -16.40405592474728635 ) ) ;
#4925 = ORIENTED_EDGE ( 'NONE', *, *, #5213, .F. ) ;
#4926 = ADVANCED_FACE ( 'NONE', ( #33479 ), #11609, .T. ) ;
#4927 = VECTOR ( 'NONE', #5939, 1000.000000000000000 ) ;
#4928 = LINE ( 'NONE', #15824, #10602 ) ;
#4929 = ADVANCED_FACE ( 'NONE', ( #17661 ), #19965, .F. ) ;
#4930 = CARTESIAN_POINT ( 'NONE',  ( -430.0000000000000000, 132.9999999999999716, 113.9999999999999858 ) ) ;
#4931 = LINE ( 'NONE', #15828, #9784 ) ;
#4932 = ORIENTED_EDGE ( 'NONE', *, *, #16204, .T. ) ;
#4933 = VECTOR ( 'NONE', #16029, 1000.000000000000000 ) ;
#4934 = CIRCLE ( 'NONE', #14708, 12.50000000000000000 ) ;
#4935 = EDGE_CURVE ( 'NONE', #13888, #35039, #14638, .T. ) ;
#4936 = EDGE_CURVE ( 'NONE', #25101, #3590, #25464, .T. ) ;
#4937 = CARTESIAN_POINT ( 'NONE',  ( -15.99999999999998579, -112.9999999999999858, 174.9999999999999432 ) ) ;
#4938 = VERTEX_POINT ( 'NONE', #20317 ) ;
#4939 = DIRECTION ( 'NONE',  ( 0.000000000000000000, 0.000000000000000000, -1.000000000000000000 ) ) ;
#4940 = EDGE_CURVE ( 'NONE', #4151, #11554, #10140, .T. ) ;
#4941 = CARTESIAN_POINT ( 'NONE',  ( -12.00000000000001066, 124.9999999999999716, 155.0000000000000000 ) ) ;
#4942 = EDGE_LOOP ( 'NONE', ( #21439, #33003, #28983, #33705 ) ) ;
#4943 = CARTESIAN_POINT ( 'NONE',  ( -347.0000000000000000, 124.9999999999999432, 168.9999999999999716 ) ) ;
#4944 = VECTOR ( 'NONE', #10971, 1000.000000000000000 ) ;
#4945 = DIRECTION ( 'NONE',  ( -1.000000000000000000, 0.000000000000000000, 0.000000000000000000 ) ) ;
#4946 = CYLINDRICAL_SURFACE ( 'NONE', #12641, 11.80000000000000071 ) ;
#4947 = EDGE_LOOP ( 'NONE', ( #30164, #18875, #27210, #25641 ) ) ;
#4948 = VERTEX_POINT ( 'NONE', #3570 ) ;
#4949 = CIRCLE ( 'NONE', #12376, 32.54542015209056416 ) ;
#4950 = DIRECTION ( 'NONE',  ( -7.893605728314050488E-14, 1.618803117314786135E-15, 0.9999999999999998890 ) ) ;
#4951 = ORIENTED_EDGE ( 'NONE', *, *, #22673, .F. ) ;
#4952 = DIRECTION ( 'NONE',  ( 0.000000000000000000, 0.000000000000000000, -1.000000000000000000 ) ) ;
#4953 = VECTOR ( 'NONE', #12007, 1000.000000000000000 ) ;
#4954 = AXIS2_PLACEMENT_3D ( 'NONE', #11617, #22468, #8221 ) ;
#4955 = PLANE ( 'NONE',  #33779 ) ;
#4956 = CARTESIAN_POINT ( 'NONE',  ( 108.7726925648793070, -4.338569679229816067, 6.125236864567445316 ) ) ;
#4957 = ORIENTED_EDGE ( 'NONE', *, *, #7933, .T. ) ;
#4958 = DIRECTION ( 'NONE',  ( 0.000000000000000000, 0.000000000000000000, 1.000000000000000000 ) ) ;
#4959 = VECTOR ( 'NONE', #18655, 1000.000000000000000 ) ;
#4961 = DIRECTION ( 'NONE',  ( 0.000000000000000000, 0.000000000000000000, 1.000000000000000000 ) ) ;
#4960 = FACE_OUTER_BOUND ( 'NONE', #17112, .T. ) ;
#4962 = ORIENTED_EDGE ( 'NONE', *, *, #18553, .T. ) ;
#4963 = ORIENTED_EDGE ( 'NONE', *, *, #20775, .T. ) ;
#4964 = CARTESIAN_POINT ( 'NONE',  ( 2.567399184519788768, -37.78162119159486565, 68.31122994652405112 ) ) ;
#4965 = ORIENTED_EDGE ( 'NONE', *, *, #31449, .F. ) ;
#4966 = CARTESIAN_POINT ( 'NONE',  ( 2.765921099433443775, -26.45933846664182099, -16.32596387352474565 ) ) ;
#4967 = EDGE_CURVE ( 'NONE', #7013, #474, #20146, .T. ) ;
#4968 = LINE ( 'NONE', #34895, #26777 ) ;
#4969 = ORIENTED_EDGE ( 'NONE', *, *, #5430, .T. ) ;
#4970 = CARTESIAN_POINT ( 'NONE',  ( 0.000000000000000000, -25.83993731729808729, 18.77381338200959604 ) ) ;
#4971 = VECTOR ( 'NONE', #29657, 1000.000000000000000 ) ;
#4972 = EDGE_CURVE ( 'NONE', #34245, #11988, #16489, .T. ) ;
#4973 = EDGE_CURVE ( 'NONE', #17236, #13268, #34177, .T. ) ;
#4974 = CARTESIAN_POINT ( 'NONE',  ( 3.754050022231059892E-15, -12.02207793746707765, -6.177150199754210647 ) ) ;
#4975 = ORIENTED_EDGE ( 'NONE', *, *, #30527, .T. ) ;
#4976 = FACE_OUTER_BOUND ( 'NONE', #12978, .T. ) ;
#4977 = PLANE ( 'NONE',  #19993 ) ;
#4978 = DIRECTION ( 'NONE',  ( 0.000000000000000000, -1.000000000000000000, -3.083952846180991760E-16 ) ) ;
#4980 = DIRECTION ( 'NONE',  ( 1.000000000000000000, 0.000000000000000000, 0.000000000000000000 ) ) ;
#4979 = CARTESIAN_POINT ( 'NONE',  ( 22.89764159710615132, -5.651112684911595352, -87.50000000000000000 ) ) ;
#4981 = VECTOR ( 'NONE', #744, 1000.000000000000000 ) ;
#4982 = AXIS2_PLACEMENT_3D ( 'NONE', #29015, #1965, #34362 ) ;
#4983 = CARTESIAN_POINT ( 'NONE',  ( 15.44711578872680846, -28.64595934308655956, 68.31122994652405112 ) ) ;
#4984 = CARTESIAN_POINT ( 'NONE',  ( -6.637260778198712075, 37.28255902965930346, -36.68877005347593467 ) ) ;
#4985 = CARTESIAN_POINT ( 'NONE',  ( 55.00000000000000711, 0.000000000000000000, 6.898500000000000298 ) ) ;
#4986 = EDGE_CURVE ( 'NONE', #21129, #24766, #32025, .T. ) ;
#4987 = VECTOR ( 'NONE', #27292, 1000.000000000000000 ) ;
#4988 = ORIENTED_EDGE ( 'NONE', *, *, #27834, .F. ) ;
#4989 = DIRECTION ( 'NONE',  ( 0.000000000000000000, 0.000000000000000000, 1.000000000000000000 ) ) ;
#4990 =( NAMED_UNIT ( * ) SI_UNIT ( $, .STERADIAN. ) SOLID_ANGLE_UNIT ( ) );
#4991 = PRODUCT_DEFINITION_CONTEXT ( 'detailed design', #27146, 'design' ) ;
#4992 = EDGE_LOOP ( 'NONE', ( #13882, #8361, #15083, #8795 ) ) ;
#4994 = ORIENTED_EDGE ( 'NONE', *, *, #17509, .T. ) ;
#4993 = EDGE_CURVE ( 'NONE', #26683, #33608, #23677, .T. ) ;
#4995 = EDGE_CURVE ( 'NONE', #1095, #10828, #4789, .T. ) ;
#4996 = EDGE_CURVE ( 'NONE', #22138, #25172, #4604, .T. ) ;
#4997 = DIRECTION ( 'NONE',  ( 0.9868265225415260300, 0.1617819965527650394, -0.000000000000000000 ) ) ;
#4998 = ORIENTED_EDGE ( 'NONE', *, *, #21523, .T. ) ;
#4999 = VERTEX_POINT ( 'NONE', #34708 ) ;
#5000 = LINE ( 'NONE', #13390, #2548 ) ;
#5001 = DIRECTION ( 'NONE',  ( 0.000000000000000000, -1.000000000000000000, 2.465190328815661892E-32 ) ) ;
#5002 = EDGE_CURVE ( 'NONE', #22371, #14920, #15688, .T. ) ;
#5003 = ITEM_DEFINED_TRANSFORMATION ( 'NONE', 'NONE', #7577,  #28566 ) ;
#5004 = CIRCLE ( 'NONE', #24905, 10.30000000000000071 ) ;
#5005 = DIRECTION ( 'NONE',  ( -1.000000000000000000, -0.000000000000000000, 0.000000000000000000 ) ) ;
#5006 = EDGE_LOOP ( 'NONE', ( #30955, #3980, #29530, #11072 ) ) ;
#5007 = ORIENTED_EDGE ( 'NONE', *, *, #1761, .F. ) ;
#5008 = DIRECTION ( 'NONE',  ( 0.000000000000000000, 1.310824597558155437E-49, 1.000000000000000000 ) ) ;
#5009 = LINE ( 'NONE', #24050, #23783 ) ;
#5010 = DIRECTION ( 'NONE',  ( 1.000000000000000000, 0.000000000000000000, -0.000000000000000000 ) ) ;
#5011 = CARTESIAN_POINT ( 'NONE',  ( -355.0000000000000000, -131.0000000000000000, 111.9999999999999858 ) ) ;
#5012 = CARTESIAN_POINT ( 'NONE',  ( -9.144464960067640646, -31.23432620483743705, -36.68877005347593467 ) ) ;
#5013 = ORIENTED_EDGE ( 'NONE', *, *, #28068, .F. ) ;
#5014 = AXIS2_PLACEMENT_3D ( 'NONE', #20278, #28450, #25774 ) ;
#5015 = CARTESIAN_POINT ( 'NONE',  ( -355.0000000000000000, -131.0000000000000000, 109.9999999999999858 ) ) ;
#5016 = CARTESIAN_POINT ( 'NONE',  ( 37.71145559917817280, 3.353962854566138851, 49.43553178847298568 ) ) ;
#5017 = LINE ( 'NONE', #18921, #19773 ) ;
#5018 = ADVANCED_FACE ( 'NONE', ( #1782 ), #2299, .F. ) ;
#5019 = DIRECTION ( 'NONE',  ( 0.000000000000000000, 0.000000000000000000, 1.000000000000000000 ) ) ;
#5020 = CARTESIAN_POINT ( 'NONE',  ( -442.0000000000000000, -137.0000000000000000, 154.9999999999999716 ) ) ;
#5021 = VECTOR ( 'NONE', #22943, 1000.000000000000000 ) ;
#5022 = CARTESIAN_POINT ( 'NONE',  ( -430.0000000000000000, 118.9999999999999716, 113.9999999999999858 ) ) ;
#5024 = DIRECTION ( 'NONE',  ( 0.000000000000000000, 1.131431318426415506E-52, 1.000000000000000000 ) ) ;
#5023 = CARTESIAN_POINT ( 'NONE',  ( 0.000000000000000000, 9.869977788040968036, 30.37666815053940539 ) ) ;
#5025 = AXIS2_PLACEMENT_3D ( 'NONE', #735, #11785, #19958 ) ;
#5026 = LINE ( 'NONE', #7342, #3627 ) ;
#5027 = VERTEX_POINT ( 'NONE', #34532 ) ;
#5028 = DIRECTION ( 'NONE',  ( -1.000000000000000000, 0.000000000000000000, -5.546364386991661285E-52 ) ) ;
#5030 = DIRECTION ( 'NONE',  ( 1.000000000000000000, 0.000000000000000000, 1.300283923313630633E-47 ) ) ;
#5029 = CARTESIAN_POINT ( 'NONE',  ( -45.00000000000000000, -4.831299144296466785, -15.81122994652406355 ) ) ;
#5031 = CIRCLE ( 'NONE', #3338, 3.999999999999976019 ) ;
#5032 = ORIENTED_EDGE ( 'NONE', *, *, #9390, .F. ) ;
#5033 = DIRECTION ( 'NONE',  ( 1.000000000000000000, 0.000000000000000000, 0.000000000000000000 ) ) ;
#5034 = PRODUCT_DEFINITION_SHAPE ( 'NONE', 'NONE',  #35228 ) ;
#5035 = ORIENTED_EDGE ( 'NONE', *, *, #20099, .T. ) ;
#5036 = AXIS2_PLACEMENT_3D ( 'NONE', #2438, #32687, #10641 ) ;
#5037 = EDGE_CURVE ( 'NONE', #32385, #34696, #18195, .T. ) ;
#5038 = ADVANCED_FACE ( 'NONE', ( #10148 ), #23495, .T. ) ;
#5039 = ORIENTED_EDGE ( 'NONE', *, *, #31322, .T. ) ;
#5040 = DIRECTION ( 'NONE',  ( 0.9075754196709571175, -0.4198891015602644883, -7.713237663339537239E-17 ) ) ;
#5041 = VERTEX_POINT ( 'NONE', #34894 ) ;
#5042 = ORIENTED_EDGE ( 'NONE', *, *, #32400, .T. ) ;
#5043 = CARTESIAN_POINT ( 'NONE',  ( -442.0000000000000000, -105.0000000000000142, -155.0000000000000000 ) ) ;
#5044 = AXIS2_PLACEMENT_3D ( 'NONE', #28411, #22896, #17227 ) ;
#5045 = DIRECTION ( 'NONE',  ( 0.000000000000000000, 0.000000000000000000, 1.000000000000000000 ) ) ;
#5046 = PLANE ( 'NONE',  #2878 ) ;
#5047 = ORIENTED_EDGE ( 'NONE', *, *, #8835, .F. ) ;
#5048 = ORIENTED_EDGE ( 'NONE', *, *, #9299, .F. ) ;
#5049 = CARTESIAN_POINT ( 'NONE',  ( 1.040000000000001368, -30.28730148581149706, -16.34215476954066304 ) ) ;
#5050 = DIRECTION ( 'NONE',  ( 0.000000000000000000, 0.000000000000000000, -1.000000000000000000 ) ) ;
#5051 = CARTESIAN_POINT ( 'NONE',  ( 0.006915246992955798207, 27.98916443103565399, -12.86217335695007868 ) ) ;
#5052 = CARTESIAN_POINT ( 'NONE',  ( -26.18205399241665177, -19.33143609808334418, -36.68877005347593467 ) ) ;
#5053 = LINE ( 'NONE', #16470, #25052 ) ;
#5054 = ORIENTED_EDGE ( 'NONE', *, *, #5438, .T. ) ;
#5055 = VECTOR ( 'NONE', #4729, 1000.000000000000000 ) ;
#5056 = DIRECTION ( 'NONE',  ( -0.000000000000000000, -1.000000000000000000, -0.000000000000000000 ) ) ;
#5057 = CARTESIAN_POINT ( 'NONE',  ( -361.0000000000000000, -125.0000000000000284, 168.9999999999999716 ) ) ;
#5058 = ORIENTED_EDGE ( 'NONE', *, *, #5207, .T. ) ;
#5059 = CARTESIAN_POINT ( 'NONE',  ( -20.00000000000004619, -137.0000000000000000, -187.0000000000000000 ) ) ;
#5060 = CARTESIAN_POINT ( 'NONE',  ( -500.0000000000000000, -113.0000000000000000, 190.9999999999999716 ) ) ;
#5061 = CARTESIAN_POINT ( 'NONE',  ( 2.265105943055672810, -17.22577838686547835, -28.59166429730548487 ) ) ;
#5062 = ORIENTED_EDGE ( 'NONE', *, *, #231, .F. ) ;
#5063 = VECTOR ( 'NONE', #28015, 1000.000000000000000 ) ;
#5064 = CARTESIAN_POINT ( 'NONE',  ( 44.94043929807611448, -32.65143121711728469, 20.00000000000000000 ) ) ;
#5065 = ORIENTED_EDGE ( 'NONE', *, *, #18741, .T. ) ;
#5066 = DIRECTION ( 'NONE',  ( 0.000000000000000000, 1.000000000000000000, 1.224646799147353207E-16 ) ) ;
#5067 = ORIENTED_EDGE ( 'NONE', *, *, #25008, .F. ) ;
#5068 = ADVANCED_FACE ( 'NONE', ( #26516 ), #15500, .T. ) ;
#5070 = DIRECTION ( 'NONE',  ( 1.000000000000000000, 0.000000000000000000, -0.000000000000000000 ) ) ;
#5069 = CYLINDRICAL_SURFACE ( 'NONE', #28493, 3.999999999999948042 ) ;
#5071 = DIRECTION ( 'NONE',  ( 0.000000000000000000, -1.000000000000000000, -1.310824597558155437E-49 ) ) ;
#5072 = AXIS2_PLACEMENT_3D ( 'NONE', #18220, #18395, #18749 ) ;
#5073 = EDGE_LOOP ( 'NONE', ( #6133, #11536, #3605, #34483 ) ) ;
#5074 = CYLINDRICAL_SURFACE ( 'NONE', #6927, 4.309328216469825001 ) ;
#5075 = CARTESIAN_POINT ( 'NONE',  ( 129.3530333899765594, 6.000000000000000000, 62.49999999999999289 ) ) ;
#5076 = EDGE_CURVE ( 'NONE', #18937, #9222, #19645, .T. ) ;
#5077 = VERTEX_POINT ( 'NONE', #4966 ) ;
#5078 = EDGE_CURVE ( 'NONE', #12986, #23261, #18354, .T. ) ;
#5079 = EDGE_CURVE ( 'NONE', #25727, #3001, #15866, .T. ) ;
#5080 = DIRECTION ( 'NONE',  ( -0.1063910735369225230, 0.9943243633099118073, -1.000770725407345128E-14 ) ) ;
#5081 = VERTEX_POINT ( 'NONE', #25993 ) ;
#5082 = CARTESIAN_POINT ( 'NONE',  ( 0.000000000000000000, 3.670182593897650235E-31, 87.50000000000000000 ) ) ;
#5083 = ADVANCED_FACE ( 'NONE', ( #23846 ), #31673, .F. ) ;
#5084 = ORIENTED_EDGE ( 'NONE', *, *, #1462, .T. ) ;
#5085 = B_SPLINE_CURVE_WITH_KNOTS ( 'NONE', 3,
 ( #27057, #24020, #24728, #29912, #2492, #7651 ),
 .UNSPECIFIED., .F., .F.,
 ( 4, 2, 4 ),
 ( 4.404817030685402330E-07, 0.001874269627226453306, 0.003748098772749838131 ),
 .UNSPECIFIED. ) ;
#5086 = CARTESIAN_POINT ( 'NONE',  ( -20.63749999999999929, 1.445083222993876839E-15, 11.80000000000000071 ) ) ;
#5087 = VECTOR ( 'NONE', #12336, 1000.000000000000000 ) ;
#5088 = LINE ( 'NONE', #2081, #10772 ) ;
#5089 = CARTESIAN_POINT ( 'NONE',  ( -99.95520222082589612, -0.8621751556914646342, -7.452240479933208483 ) ) ;
#5090 = LINE ( 'NONE', #14002, #18231 ) ;
#5091 = ORIENTED_EDGE ( 'NONE', *, *, #30449, .F. ) ;
#5092 = EDGE_LOOP ( 'NONE', ( #2806, #13100, #2462, #10252 ) ) ;
#5093 = ORIENTED_EDGE ( 'NONE', *, *, #27195, .F. ) ;
#5094 = FACE_OUTER_BOUND ( 'NONE', #13253, .T. ) ;
#5095 = LINE ( 'NONE', #5615, #34525 ) ;
#5096 = DIRECTION ( 'NONE',  ( 0.000000000000000000, 1.000000000000000000, 0.000000000000000000 ) ) ;
#5097 = DIRECTION ( 'NONE',  ( 0.000000000000000000, 1.836970198721029688E-16, -1.000000000000000000 ) ) ;
#5098 = CARTESIAN_POINT ( 'NONE',  ( -361.0000000000000000, 124.9999999999999432, 164.9999999999999716 ) ) ;
#5100 = CARTESIAN_POINT ( 'NONE',  ( 3.235562306570555532E-30, -5.758675521474015291, -67.50000000000000000 ) ) ;
#5099 =( REPRESENTATION_RELATIONSHIP ('NONE','NONE', #23037, #15767 ) REPRESENTATION_RELATIONSHIP_WITH_TRANSFORMATION ( #30409 )SHAPE_REPRESENTATION_RELATIONSHIP( ) );
#5101 = DIRECTION ( 'NONE',  ( -0.000000000000000000, -1.000000000000000000, -0.000000000000000000 ) ) ;
#5102 = VERTEX_POINT ( 'NONE', #21181 ) ;
#5103 = CARTESIAN_POINT ( 'NONE',  ( 22.89764159710613001, 6.310691531022070144, -77.50000000000000000 ) ) ;
#5104 = CARTESIAN_POINT ( 'NONE',  ( -5.781867695661277118, -1.866624223957557671, 4.679999999999999716 ) ) ;
#5105 = LINE ( 'NONE', #15467, #11496 ) ;
#5106 = ORIENTED_EDGE ( 'NONE', *, *, #13037, .F. ) ;
#5107 = CARTESIAN_POINT ( 'NONE',  ( -12.00000000000001066, 144.9999999999999716, 187.0000000000000000 ) ) ;
#5108 = EDGE_LOOP ( 'NONE', ( #34830, #16296, #32852, #25071 ) ) ;
#5109 = B_SPLINE_CURVE_WITH_KNOTS ( 'NONE', 3,
 ( #4697, #34626, #6853, #34095, #31426, #15592 ),
 .UNSPECIFIED., .F., .F.,
 ( 4, 2, 4 ),
 ( 2.073839991539819829E-07, 0.001873405686414693827, 0.003746603988830233666 ),
 .UNSPECIFIED. ) ;
#5110 = CARTESIAN_POINT ( 'NONE',  ( -103.6627159225451180, 4.948560684155824951, -11.47897987543853660 ) ) ;
#5111 = LINE ( 'NONE', #21843, #9888 ) ;
#5112 = CIRCLE ( 'NONE', #14244, 12.50000000000000000 ) ;
#5113 = ORIENTED_EDGE ( 'NONE', *, *, #3278, .T. ) ;
#5114 = EDGE_CURVE ( 'NONE', #7721, #26602, #28390, .T. ) ;
#5115 = DIRECTION ( 'NONE',  ( 0.9868265225415260300, -0.1617819965527647341, 0.000000000000000000 ) ) ;
#5116 = LINE ( 'NONE', #22035, #19055 ) ;
#5117 = LINE ( 'NONE', #26844, #12069 ) ;
#5118 = EDGE_CURVE ( 'NONE', #29579, #31238, #5664, .T. ) ;
#5119 = ORIENTED_EDGE ( 'NONE', *, *, #18466, .T. ) ;
#5120 = ORIENTED_EDGE ( 'NONE', *, *, #21973, .F. ) ;
#5121 = DIRECTION ( 'NONE',  ( -0.1063910735369017202, 0.9943243633099136947, -1.000770725407181676E-14 ) ) ;
#5122 = CARTESIAN_POINT ( 'NONE',  ( -35.00000000000000000, -4.831299144296466785, -15.81122994652406355 ) ) ;
#5123 = EDGE_CURVE ( 'NONE', #30715, #6277, #24412, .T. ) ;
#5124 = ORIENTED_EDGE ( 'NONE', *, *, #11905, .F. ) ;
#5125 = DIRECTION ( 'NONE',  ( 0.000000000000000000, 0.000000000000000000, 1.000000000000000000 ) ) ;
#5126 = CARTESIAN_POINT ( 'NONE',  ( -442.0000000000000000, 105.0000000000000000, -69.99999999999998579 ) ) ;
#5127 = CARTESIAN_POINT ( 'NONE',  ( 2.789999999999999147, 9.869977788041397915, -27.85166815053926115 ) ) ;
#5128 = DIRECTION ( 'NONE',  ( 0.000000000000000000, 7.888609052210118054E-31, 1.000000000000000000 ) ) ;
#5129 = ADVANCED_FACE ( 'NONE', ( #24719 ), #530, .T. ) ;
#5130 = VERTEX_POINT ( 'NONE', #27396 ) ;
#5131 = CIRCLE ( 'NONE', #11487, 7.999999999999979572 ) ;
#5132 = DIRECTION ( 'NONE',  ( 1.000000000000000000, 0.000000000000000000, 0.000000000000000000 ) ) ;
#5133 = EDGE_CURVE ( 'NONE', #33286, #25337, #16417, .T. ) ;
#5134 = VECTOR ( 'NONE', #20438, 1000.000000000000000 ) ;
#5135 = EDGE_CURVE ( 'NONE', #22985, #26377, #26123, .T. ) ;
#5137 = CARTESIAN_POINT ( 'NONE',  ( 2.033800773663356765, -10.98362253094254726, 32.08736770015211448 ) ) ;
#5136 = LINE ( 'NONE', #2474, #31524 ) ;
#5138 = ORIENTED_EDGE ( 'NONE', *, *, #2842, .F. ) ;
#5139 = ORIENTED_EDGE ( 'NONE', *, *, #18904, .T. ) ;
#5140 = CARTESIAN_POINT ( 'NONE',  ( 0.7564103416931459156, 5.833445725192799358, 33.41010632092324073 ) ) ;
#5141 = ORIENTED_EDGE ( 'NONE', *, *, #10617, .T. ) ;
#5142 = DIRECTION ( 'NONE',  ( 0.000000000000000000, 1.000000000000000000, -6.123233995736766036E-17 ) ) ;
#5143 = LINE ( 'NONE', #31844, #34170 ) ;
#5144 = ORIENTED_EDGE ( 'NONE', *, *, #15905, .T. ) ;
#5145 = PLANE ( 'NONE',  #7264 ) ;
#5146 = VECTOR ( 'NONE', #21224, 1000.000000000000000 ) ;
#5147 = VECTOR ( 'NONE', #13455, 1000.000000000000000 ) ;
#5148 = DIRECTION ( 'NONE',  ( 1.000000000000000000, 0.000000000000000000, 0.000000000000000000 ) ) ;
#5149 = ORIENTED_EDGE ( 'NONE', *, *, #28007, .T. ) ;
#5150 = CARTESIAN_POINT ( 'NONE',  ( -32.37866696771086339, 3.290334066652097267, -36.68877005347593467 ) ) ;
#5151 = CARTESIAN_POINT ( 'NONE',  ( -500.0000000000000000, -141.0000000000000000, 187.0000000000000000 ) ) ;
#5152 = CARTESIAN_POINT ( 'NONE',  ( -418.0000000000000000, 124.9999999999999432, -155.0000000000000000 ) ) ;
#5153 = CARTESIAN_POINT ( 'NONE',  ( -12.00000000000001066, -141.0000000000000000, 155.0000000000000000 ) ) ;
#5154 = FACE_OUTER_BOUND ( 'NONE', #27045, .T. ) ;
#5155 = CARTESIAN_POINT ( 'NONE',  ( -262.5000000000000000, 0.000000000000000000, 0.000000000000000000 ) ) ;
#5156 = VECTOR ( 'NONE', #16117, 1000.000000000000114 ) ;
#5157 = LINE ( 'NONE', #13375, #26881 ) ;
#5158 = VECTOR ( 'NONE', #4685, 1000.000000000000000 ) ;
#5159 = ORIENTED_EDGE ( 'NONE', *, *, #253, .T. ) ;
#5160 = DIRECTION ( 'NONE',  ( 0.000000000000000000, 1.836970198721029441E-16, -1.000000000000000000 ) ) ;
#5161 = DIRECTION ( 'NONE',  ( 1.000000000000000000, 0.000000000000000000, 0.000000000000000000 ) ) ;
#5162 = ORIENTED_EDGE ( 'NONE', *, *, #6706, .F. ) ;
#5163 = ORIENTED_EDGE ( 'NONE', *, *, #5759, .T. ) ;
#5164 = ADVANCED_FACE ( 'NONE', ( #16561 ), #32733, .F. ) ;
#5165 = VECTOR ( 'NONE', #5319, 1000.000000000000000 ) ;
#5166 = EDGE_CURVE ( 'NONE', #34985, #30302, #27187, .T. ) ;
#5167 = DIRECTION ( 'NONE',  ( 0.000000000000000000, -1.000000000000000000, -0.000000000000000000 ) ) ;
#5168 = ADVANCED_FACE ( 'NONE', ( #16392 ), #27573, .F. ) ;
#5169 = DIRECTION ( 'NONE',  ( 1.000000000000000000, 0.000000000000000000, 0.000000000000000000 ) ) ;
#5170 = AXIS2_PLACEMENT_3D ( 'NONE', #4806, #7657, #2313 ) ;
#5171 = VERTEX_POINT ( 'NONE', #27046 ) ;
#5172 = DIRECTION ( 'NONE',  ( 1.300283923313630633E-47, 0.000000000000000000, 1.000000000000000000 ) ) ;
#5173 = CARTESIAN_POINT ( 'NONE',  ( 10.17231796313407344, -5.651112684911598016, -77.50000000000000000 ) ) ;
#5174 = ORIENTED_EDGE ( 'NONE', *, *, #33517, .F. ) ;
#5175 = VERTEX_POINT ( 'NONE', #355 ) ;
#5176 = CARTESIAN_POINT ( 'NONE',  ( -9.978866888775632660, -1.691831803474591833, -67.50000000000000000 ) ) ;
#5178 = DIRECTION ( 'NONE',  ( 0.000000000000000000, 0.000000000000000000, -1.000000000000000000 ) ) ;
#5177 = CIRCLE ( 'NONE', #24486, 2.033421858999710619 ) ;
#5179 = CARTESIAN_POINT ( 'NONE',  ( 3.985664461616346953E-15, 32.54542015209056416, 68.31122994652405112 ) ) ;
#5181 = EDGE_CURVE ( 'NONE', #29231, #27481, #13529, .T. ) ;
#5180 = FACE_OUTER_BOUND ( 'NONE', #20182, .T. ) ;
#5182 = CARTESIAN_POINT ( 'NONE',  ( -12.00000000000001066, -124.9999999999999432, -154.9999999999999716 ) ) ;
#5183 = EDGE_LOOP ( 'NONE', ( #28428, #12778, #10898, #34241, #29681, #32616, #19948, #11191 ) ) ;
#5184 = CIRCLE ( 'NONE', #13745, 3.999999999999976019 ) ;
#5185 = CARTESIAN_POINT ( 'NONE',  ( -15.99999999999998579, -124.9999999999999432, -162.9999999999999432 ) ) ;
#5186 = DIRECTION ( 'NONE',  ( -0.000000000000000000, -1.000000000000000000, -0.000000000000000000 ) ) ;
#5187 = DIRECTION ( 'NONE',  ( 1.000000000000000000, 0.000000000000000000, 0.000000000000000000 ) ) ;
#5188 = CARTESIAN_POINT ( 'NONE',  ( -105.0000000000000000, 0.000000000000000000, 60.00000000000000000 ) ) ;
#5189 = EDGE_CURVE ( 'NONE', #20760, #34690, #26627, .T. ) ;
#5190 = LINE ( 'NONE', #32260, #9834 ) ;
#5192 = LINE ( 'NONE', #16087, #24187 ) ;
#5191 = DIRECTION ( 'NONE',  ( 0.000000000000000000, 0.000000000000000000, -1.000000000000000000 ) ) ;
#5193 = EDGE_CURVE ( 'NONE', #3477, #16642, #15856, .T. ) ;
#5194 = EDGE_CURVE ( 'NONE', #7946, #17530, #13952, .T. ) ;
#5195 = AXIS2_PLACEMENT_3D ( 'NONE', #9194, #20067, #17583 ) ;
#5196 = FACE_OUTER_BOUND ( 'NONE', #11018, .T. ) ;
#5198 = EDGE_LOOP ( 'NONE', ( #21138, #11714, #13499, #26497 ) ) ;
#5197 = CIRCLE ( 'NONE', #29631, 32.54542015209056416 ) ;
#5199 = CIRCLE ( 'NONE', #14338, 7.999999999999952038 ) ;
#5201 = DIRECTION ( 'NONE',  ( 1.000000000000000000, 0.000000000000000000, -1.848892746611746966E-32 ) ) ;
#5200 = LINE ( 'NONE', #7520, #29707 ) ;
#5202 = ORIENTED_EDGE ( 'NONE', *, *, #16240, .T. ) ;
#5203 = DIRECTION ( 'NONE',  ( 1.000000000000000000, 0.000000000000000000, 0.000000000000000000 ) ) ;
#5204 = EDGE_LOOP ( 'NONE', ( #23392, #8814, #21848, #26233 ) ) ;
#5205 = CIRCLE ( 'NONE', #23420, 4.000000000000003553 ) ;
#5206 = EDGE_CURVE ( 'NONE', #24311, #10245, #32875, .T. ) ;
#5207 = EDGE_CURVE ( 'NONE', #22615, #28417, #2831, .T. ) ;
#5208 = VERTEX_POINT ( 'NONE', #2480 ) ;
#5209 = FACE_OUTER_BOUND ( 'NONE', #31791, .T. ) ;
#5210 = ORIENTED_EDGE ( 'NONE', *, *, #34210, .F. ) ;
#5211 = ORIENTED_EDGE ( 'NONE', *, *, #21013, .F. ) ;
#5212 = CARTESIAN_POINT ( 'NONE',  ( 31.73435513276359643, 7.220462394039750542, 68.31122994652405112 ) ) ;
#5213 = EDGE_CURVE ( 'NONE', #23118, #27049, #32375, .T. ) ;
#5214 = VECTOR ( 'NONE', #22208, 1000.000000000000000 ) ;
#5215 = CARTESIAN_POINT ( 'NONE',  ( -14.49673343639653744, 34.98409864655523904, -36.68877005347593467 ) ) ;
#5216 = AXIS2_PLACEMENT_3D ( 'NONE', #16305, #5229, #32819 ) ;
#5217 = CARTESIAN_POINT ( 'NONE',  ( 26.04754872656010178, -19.51229300245306320, 68.31122994652405112 ) ) ;
#5218 = ORIENTED_EDGE ( 'NONE', *, *, #31065, .F. ) ;
#5219 = ORIENTED_EDGE ( 'NONE', *, *, #28327, .T. ) ;
#5220 = VECTOR ( 'NONE', #27147, 1000.000000000000000 ) ;
#5221 = CARTESIAN_POINT ( 'NONE',  ( 0.02407890056655608360, -27.96208973699893008, -13.59246946040217630 ) ) ;
#5222 = LINE ( 'NONE', #23763, #15916 ) ;
#5223 = DIRECTION ( 'NONE',  ( -1.000000000000000000, 0.000000000000000000, 0.000000000000000000 ) ) ;
#5224 = ORIENTED_EDGE ( 'NONE', *, *, #18035, .F. ) ;
#5225 = LINE ( 'NONE', #10773, #6000 ) ;
#5226 = DIRECTION ( 'NONE',  ( 1.000000000000000000, 0.000000000000000000, 0.000000000000000000 ) ) ;
#5227 = ORIENTED_EDGE ( 'NONE', *, *, #29984, .F. ) ;
#5228 = DIRECTION ( 'NONE',  ( 5.546364386991661285E-52, 0.000000000000000000, 1.000000000000000000 ) ) ;
#5229 = DIRECTION ( 'NONE',  ( -1.000000000000000000, 0.000000000000000000, -0.000000000000000000 ) ) ;
#5230 = CARTESIAN_POINT ( 'NONE',  ( 187.4264068711928530, -12.50000000000001066, 15.00000000000001243 ) ) ;
#5231 = ORIENTED_EDGE ( 'NONE', *, *, #20853, .F. ) ;
#5232 = ADVANCED_FACE ( 'NONE', ( #13362 ), #13879, .T. ) ;
#5233 = PLANE ( 'NONE',  #19482 ) ;
#5234 = VERTEX_POINT ( 'NONE', #29718 ) ;
#5235 = EDGE_CURVE ( 'NONE', #25895, #5645, #5318, .T. ) ;
#5236 = DIRECTION ( 'NONE',  ( 0.000000000000000000, 0.000000000000000000, -1.000000000000000000 ) ) ;
#5237 = VERTEX_POINT ( 'NONE', #16919 ) ;
#5239 = CARTESIAN_POINT ( 'NONE',  ( 1.040000000000000258, 22.14447232807544452, -26.34405054495532639 ) ) ;
#5238 = CARTESIAN_POINT ( 'NONE',  ( 10.17231796313407344, -1.579009122040560431, -87.50000000000000000 ) ) ;
#5240 = DIRECTION ( 'NONE',  ( -0.000000000000000000, -1.836970198721029688E-16, 1.000000000000000000 ) ) ;
#5241 = EDGE_CURVE ( 'NONE', #32323, #33070, #14144, .T. ) ;
#5242 =( GEOMETRIC_REPRESENTATION_CONTEXT ( 3 ) GLOBAL_UNCERTAINTY_ASSIGNED_CONTEXT ( ( #9608 ) ) GLOBAL_UNIT_ASSIGNED_CONTEXT ( ( #24956, #11279, #14303 ) ) REPRESENTATION_CONTEXT ( 'NONE', 'WORKASPACE' ) );
#5243 = EDGE_CURVE ( 'NONE', #22914, #29991, #19756, .T. ) ;
#5245 = EDGE_LOOP ( 'NONE', ( #11945, #24399, #34992, #4898, #1637, #15865, #30497, #24758 ) ) ;
#5244 = CIRCLE ( 'NONE', #25143, 7.999999999999979572 ) ;
#5246 = VECTOR ( 'NONE', #21760, 1000.000000000000000 ) ;
#5247 = VECTOR ( 'NONE', #28936, 1000.000000000000000 ) ;
#5248 = LINE ( 'NONE', #13112, #5220 ) ;
#5249 = ADVANCED_FACE ( 'NONE', ( #6561 ), #1228, .F. ) ;
#5250 = DIRECTION ( 'NONE',  ( 0.000000000000000000, -1.000000000000000000, -1.836970198721029934E-16 ) ) ;
#5251 = EDGE_LOOP ( 'NONE', ( #20390, #31552, #25028, #22486 ) ) ;
#5252 = ORIENTED_EDGE ( 'NONE', *, *, #27717, .F. ) ;
#5253 = CARTESIAN_POINT ( 'NONE',  ( -5.210000000000000853, 0.000000000000000000, 0.000000000000000000 ) ) ;
#5254 = LINE ( 'NONE', #8468, #13620 ) ;
#5255 = VERTEX_POINT ( 'NONE', #33440 ) ;
#5256 = FACE_OUTER_BOUND ( 'NONE', #27990, .T. ) ;
#5257 =( LENGTH_UNIT ( ) NAMED_UNIT ( * ) SI_UNIT ( .MILLI., .METRE. ) );
#5258 = CARTESIAN_POINT ( 'NONE',  ( -102.7050928880580329, -4.583230167788444831, -5.938965658480648280 ) ) ;
#5259 = DIRECTION ( 'NONE',  ( 0.000000000000000000, 0.000000000000000000, 1.000000000000000000 ) ) ;
#5260 = ORIENTED_EDGE ( 'NONE', *, *, #21334, .F. ) ;
#5261 = ORIENTED_EDGE ( 'NONE', *, *, #30865, .T. ) ;
#5262 = VERTEX_POINT ( 'NONE', #17274 ) ;
#5263 = CARTESIAN_POINT ( 'NONE',  ( 11.99999999999995559, -134.9999999999999716, -186.9999999999999716 ) ) ;
#5264 = EDGE_CURVE ( 'NONE', #25766, #24257, #9596, .T. ) ;
#5265 = CYLINDRICAL_SURFACE ( 'NONE', #8945, 15.00000000000000000 ) ;
#5266 = B_SPLINE_CURVE_WITH_KNOTS ( 'NONE', 3,
 ( #33014, #18996, #2947, #11505 ),
 .UNSPECIFIED., .F., .F.,
 ( 4, 4 ),
 ( 0.005298373595863164684, 0.005985241895929849926 ),
 .UNSPECIFIED. ) ;
#5267 = CARTESIAN_POINT ( 'NONE',  ( -19.99999999999998934, -134.9999999999999716, 187.0000000000000000 ) ) ;
#5268 = AXIS2_PLACEMENT_3D ( 'NONE', #22964, #12122, #33816 ) ;
#5269 = FACE_OUTER_BOUND ( 'NONE', #10633, .T. ) ;
#5270 = CARTESIAN_POINT ( 'NONE',  ( 1.394999999999999574, 6.183021911001842064, 33.85493898757065523 ) ) ;
#5271 = VECTOR ( 'NONE', #31778, 1000.000000000000000 ) ;
#5272 = COLOUR_RGB ( '',0.7921568627450980005, 0.8196078431372548767, 0.9333333333333333481 ) ;
#5273 = DIRECTION ( 'NONE',  ( 1.000000000000000000, -0.000000000000000000, -0.000000000000000000 ) ) ;
#5274 = AXIS2_PLACEMENT_3D ( 'NONE', #3581, #28336, #24943 ) ;
#5275 = LINE ( 'NONE', #35030, #6177 ) ;
#5276 = ORIENTED_EDGE ( 'NONE', *, *, #25205, .T. ) ;
#5277 = ADVANCED_FACE ( 'NONE', ( #19578 ), #19926, .F. ) ;
#5278 = CARTESIAN_POINT ( 'NONE',  ( 2.765921099433443331, -3.506335382740311868, -30.89238256715869468 ) ) ;
#5279 = LINE ( 'NONE', #8659, #19460 ) ;
#5280 = EDGE_CURVE ( 'NONE', #1101, #12035, #25598, .T. ) ;
#5281 = CARTESIAN_POINT ( 'NONE',  ( 2.789999999999999147, -0.09145294252698496495, 30.47036804522407749 ) ) ;
#5282 = VERTEX_POINT ( 'NONE', #30773 ) ;
#5283 = EDGE_CURVE ( 'NONE', #12803, #16672, #14600, .T. ) ;
#5284 = DIRECTION ( 'NONE',  ( -0.000000000000000000, 2.465190328815661892E-32, 1.000000000000000000 ) ) ;
#5285 = ORIENTED_EDGE ( 'NONE', *, *, #15353, .T. ) ;
#5286 = CARTESIAN_POINT ( 'NONE',  ( 2.789999999999999147, 29.94779062842786743, 5.619744560739183825 ) ) ;
#5287 = CARTESIAN_POINT ( 'NONE',  ( 2.789999999999999147, -29.68817180695669578, -9.232883799364548949 ) ) ;
#5288 = CIRCLE ( 'NONE', #11570, 3.999999999999976019 ) ;
#5289 = ORIENTED_EDGE ( 'NONE', *, *, #25264, .T. ) ;
#5290 = DIRECTION ( 'NONE',  ( 1.000000000000000000, 0.000000000000000000, 0.000000000000000000 ) ) ;
#5291 = DIRECTION ( 'NONE',  ( -1.000000000000000000, -0.000000000000000000, -0.000000000000000000 ) ) ;
#5292 = DIRECTION ( 'NONE',  ( 0.000000000000000000, -1.000000000000000000, -0.000000000000000000 ) ) ;
#5293 = ORIENTED_EDGE ( 'NONE', *, *, #6404, .T. ) ;
#5294 = AXIS2_PLACEMENT_3D ( 'NONE', #7266, #6918, #23312 ) ;
#5295 = ORIENTED_EDGE ( 'NONE', *, *, #1947, .T. ) ;
#5296 = AXIS2_PLACEMENT_3D ( 'NONE', #33363, #28555, #22870 ) ;
#5297 = CARTESIAN_POINT ( 'NONE',  ( 782.2089425601827770, 1372.430637675913886, 1753.598338701303874 ) ) ;
#5298 = AXIS2_PLACEMENT_3D ( 'NONE', #3928, #11973, #932 ) ;
#5299 = DIRECTION ( 'NONE',  ( 0.000000000000000000, 1.000000000000000000, 0.000000000000000000 ) ) ;
#5300 = ORIENTED_EDGE ( 'NONE', *, *, #29781, .T. ) ;
#5301 = LINE ( 'NONE', #19212, #28303 ) ;
#5302 = DIRECTION ( 'NONE',  ( 0.000000000000000000, -1.000000000000000000, 0.000000000000000000 ) ) ;
#5303 = DIRECTION ( 'NONE',  ( -0.000000000000000000, -0.000000000000000000, -1.000000000000000000 ) ) ;
#5304 = CARTESIAN_POINT ( 'NONE',  ( -109.5657259334022342, -2.311989032590052950, 7.136426621730641351 ) ) ;
#5305 = CONTEXT_DEPENDENT_SHAPE_REPRESENTATION ( #8749, #25658 ) ;
#5306 = ORIENTED_EDGE ( 'NONE', *, *, #14522, .F. ) ;
#5307 =( REPRESENTATION_RELATIONSHIP ('NONE','NONE', #23037, #15767 ) REPRESENTATION_RELATIONSHIP_WITH_TRANSFORMATION ( #1084 )SHAPE_REPRESENTATION_RELATIONSHIP( ) );
#5308 = ORIENTED_EDGE ( 'NONE', *, *, #22945, .F. ) ;
#5309 = CARTESIAN_POINT ( 'NONE',  ( 2.789999999999999147, 2.005524111408653720, -31.87689292423236154 ) ) ;
#5310 = VECTOR ( 'NONE', #27370, 1000.000000000000000 ) ;
#5312 = DIRECTION ( 'NONE',  ( 0.000000000000000000, 0.000000000000000000, 1.000000000000000000 ) ) ;
#5311 = DIRECTION ( 'NONE',  ( -1.000000000000000000, 0.000000000000000000, 0.000000000000000000 ) ) ;
#5313 = ORIENTED_EDGE ( 'NONE', *, *, #33547, .F. ) ;
#5314 = EDGE_LOOP ( 'NONE', ( #23751, #438, #34233, #23436, #14022, #30155 ) ) ;
#5315 = FACE_OUTER_BOUND ( 'NONE', #9021, .T. ) ;
#5316 = VERTEX_POINT ( 'NONE', #11565 ) ;
#5317 = ADVANCED_FACE ( 'NONE', ( #22237 ), #25426, .T. ) ;
#5318 = LINE ( 'NONE', #28286, #499 ) ;
#5319 = DIRECTION ( 'NONE',  ( 1.000000000000000000, 0.000000000000000000, 0.000000000000000000 ) ) ;
#5320 = ORIENTED_EDGE ( 'NONE', *, *, #19424, .T. ) ;
#5321 = AXIS2_PLACEMENT_3D ( 'NONE', #21297, #26279, #21474 ) ;
#5322 = VERTEX_POINT ( 'NONE', #11923 ) ;
#5323 = CARTESIAN_POINT ( 'NONE',  ( -442.0000000000000000, -124.9999999999999858, -77.99999999999997158 ) ) ;
#5324 = EDGE_CURVE ( 'NONE', #13597, #14760, #27745, .T. ) ;
#5325 = AXIS2_PLACEMENT_3D ( 'NONE', #32608, #32263, #7883 ) ;
#5326 = AXIS2_PLACEMENT_3D ( 'NONE', #18160, #1585, #4575 ) ;
#5327 = PRODUCT_DEFINITION_SHAPE ( 'NONE', 'NONE',  #35213 ) ;
#5328 = FACE_OUTER_BOUND ( 'NONE', #14914, .T. ) ;
#5329 = ORIENTED_EDGE ( 'NONE', *, *, #27121, .F. ) ;
#5330 = ADVANCED_FACE ( 'NONE', ( #25062 ), #30952, .T. ) ;
#5331 = DIRECTION ( 'NONE',  ( -0.000000000000000000, -0.000000000000000000, 1.000000000000000000 ) ) ;
#5332 = CARTESIAN_POINT ( 'NONE',  ( -8.000000000000000000, 0.000000000000000000, 0.000000000000000000 ) ) ;
#5333 = CARTESIAN_POINT ( 'NONE',  ( 2.789999999999999147, -23.70329957282570632, -20.11932597908854703 ) ) ;
#5334 = DIRECTION ( 'NONE',  ( 0.000000000000000000, 0.6845471059286788451, 0.7289686274214207673 ) ) ;
#5335 = FACE_OUTER_BOUND ( 'NONE', #7595, .T. ) ;
#5336 = CARTESIAN_POINT ( 'NONE',  ( -19.99999999999998934, -137.0000000000000000, 190.9999999999999716 ) ) ;
#5337 = CARTESIAN_POINT ( 'NONE',  ( 2.790000000000000924, 0.000000000000000000, 0.000000000000000000 ) ) ;
#5338 = EDGE_CURVE ( 'NONE', #24819, #19022, #22414, .T. ) ;
#5339 = VECTOR ( 'NONE', #17607, 1000.000000000000114 ) ;
#5340 = ORIENTED_EDGE ( 'NONE', *, *, #6899, .T. ) ;
#5341 = CARTESIAN_POINT ( 'NONE',  ( -442.0000000000000000, -105.0000000000000142, -101.9999999999999858 ) ) ;
#5342 = CARTESIAN_POINT ( 'NONE',  ( 824.8301442019526348, 989.3487216806496463, 1753.598338701303646 ) ) ;
#5343 = ORIENTED_EDGE ( 'NONE', *, *, #7900, .F. ) ;
#5344 = CIRCLE ( 'NONE', #7633, 13.50000000000000178 ) ;
#5345 = ORIENTED_EDGE ( 'NONE', *, *, #25188, .F. ) ;
#5346 = DIRECTION ( 'NONE',  ( 1.000000000000000000, 0.000000000000000000, -1.232595164407831220E-32 ) ) ;
#5347 = AXIS2_PLACEMENT_3D ( 'NONE', #24775, #8576, #2880 ) ;
#5348 = CARTESIAN_POINT ( 'NONE',  ( 99.26191511054628336, 0.3953117532656757471, 7.500000000000019540 ) ) ;
#5349 = APPLICATION_PROTOCOL_DEFINITION ( 'draft international standard', 'automotive_design', 1998, #15794 ) ;
#5350 = AXIS2_PLACEMENT_3D ( 'NONE', #23000, #33497, #25484 ) ;
#5351 = EDGE_LOOP ( 'NONE', ( #30007, #2306, #13825, #13245 ) ) ;
#5352 = CARTESIAN_POINT ( 'NONE',  ( 2.789999999999999147, 20.79173593595296055, -22.27454621808740853 ) ) ;
#5353 = CIRCLE ( 'NONE', #6481, 7.999999999999979572 ) ;
#5354 = DIRECTION ( 'NONE',  ( -1.000000000000000000, -0.000000000000000000, -0.000000000000000000 ) ) ;
#5355 = EDGE_LOOP ( 'NONE', ( #4963, #33386, #10408, #3537 ) ) ;
#5356 = ORIENTED_EDGE ( 'NONE', *, *, #5609, .F. ) ;
#5357 = DIRECTION ( 'NONE',  ( 0.000000000000000000, 0.000000000000000000, 1.000000000000000000 ) ) ;
#5358 = CARTESIAN_POINT ( 'NONE',  ( -6.500000000000000000, 0.000000000000000000, 0.000000000000000000 ) ) ;
#5359 = EDGE_CURVE ( 'NONE', #29676, #19146, #17090, .T. ) ;
#5360 = DIRECTION ( 'NONE',  ( 1.000000000000000000, -8.433758354584418579E-81, 1.232595164407830946E-32 ) ) ;
#5361 = CARTESIAN_POINT ( 'NONE',  ( 2.789999999999999147, 23.28319895603611300, -19.33937915510192695 ) ) ;
#5362 = PLANE ( 'NONE',  #11451 ) ;
#5363 = ORIENTED_EDGE ( 'NONE', *, *, #25345, .T. ) ;
#5364 = DIRECTION ( 'NONE',  ( 0.000000000000000000, 0.000000000000000000, -1.000000000000000000 ) ) ;
#5365 = CARTESIAN_POINT ( 'NONE',  ( 2.719051659264935417, -30.32005755872691921, 9.230678093032533837 ) ) ;
#5366 = AXIS2_PLACEMENT_3D ( 'NONE', #29617, #5396, #18950 ) ;
#5367 = CARTESIAN_POINT ( 'NONE',  ( 2.719051683032043254, -15.78353653323396166, 27.48438217453478671 ) ) ;
#5368 = EDGE_CURVE ( 'NONE', #27865, #19356, #17456, .T. ) ;
#5369 = VECTOR ( 'NONE', #2129, 1000.000000000000000 ) ;
#5370 = DIRECTION ( 'NONE',  ( 0.000000000000000000, -0.08715574274765887364, -0.9961946980917455452 ) ) ;
#5371 = CARTESIAN_POINT ( 'NONE',  ( 0.07098932975109609189, 7.308614668456146823, 30.84037831947998143 ) ) ;
#5372 = EDGE_CURVE ( 'NONE', #6316, #2726, #24465, .T. ) ;
#5373 = EDGE_CURVE ( 'NONE', #29370, #31410, #26756, .T. ) ;
#5374 = DIRECTION ( 'NONE',  ( 0.000000000000000000, 0.9048270524660234626, -0.4257792915650642773 ) ) ;
#5376 = CARTESIAN_POINT ( 'NONE',  ( 1.040000000000000924, 14.89726405156217126, 31.02351007835982344 ) ) ;
#5375 = LINE ( 'NONE', #26395, #4233 ) ;
#5377 = COLOUR_RGB ( '',0.7921568627450980005, 0.8196078431372548767, 0.9333333333333333481 ) ;
#5378 = ADVANCED_FACE ( 'NONE', ( #13463 ), #10664, .T. ) ;
#5379 = EDGE_CURVE ( 'NONE', #21471, #11116, #22611, .T. ) ;
#5380 = VECTOR ( 'NONE', #28814, 1000.000000000000114 ) ;
#5381 = FACE_OUTER_BOUND ( 'NONE', #16709, .T. ) ;
#5382 = VERTEX_POINT ( 'NONE', #13813 ) ;
#5383 = CYLINDRICAL_SURFACE ( 'NONE', #18473, 34.41491905851385269 ) ;
#5385 = FACE_OUTER_BOUND ( 'NONE', #19054, .T. ) ;
#5384 = CARTESIAN_POINT ( 'NONE',  ( -19.99999999999998934, 144.9999999999999147, 162.9999999999999716 ) ) ;
#5386 = EDGE_CURVE ( 'NONE', #27028, #21429, #20894, .T. ) ;
#5387 = ORIENTED_EDGE ( 'NONE', *, *, #10036, .T. ) ;
#5388 = CARTESIAN_POINT ( 'NONE',  ( -37.58721499952019940, -4.609089608337754385, 68.31122994652405112 ) ) ;
#5389 = VERTEX_POINT ( 'NONE', #5776 ) ;
#5390 = EDGE_CURVE ( 'NONE', #25766, #1742, #8110, .T. ) ;
#5391 = VECTOR ( 'NONE', #29403, 1000.000000000000000 ) ;
#5392 = EDGE_LOOP ( 'NONE', ( #22412, #4965, #27605, #29640 ) ) ;
#5393 = PLANE ( 'NONE',  #239 ) ;
#5394 = ORIENTED_EDGE ( 'NONE', *, *, #14375, .T. ) ;
#5395 = ORIENTED_EDGE ( 'NONE', *, *, #17447, .F. ) ;
#5396 = DIRECTION ( 'NONE',  ( 0.000000000000000000, -1.000000000000000000, 6.123233995736766036E-17 ) ) ;
#5397 = AXIS2_PLACEMENT_3D ( 'NONE', #2609, #13480, #24318 ) ;
#5398 = DIRECTION ( 'NONE',  ( 0.000000000000000000, 1.000000000000000000, 1.224646799147353207E-16 ) ) ;
#5399 = CARTESIAN_POINT ( 'NONE',  ( -15.99999999999998579, 75.55999999999990280, -177.7400000000000091 ) ) ;
#5400 = VERTEX_POINT ( 'NONE', #16145 ) ;
#5401 = EDGE_LOOP ( 'NONE', ( #20859, #16425, #11828, #26068 ) ) ;
#5402 = AXIS2_PLACEMENT_3D ( 'NONE', #3684, #8855, #33411 ) ;
#5403 = CARTESIAN_POINT ( 'NONE',  ( 21.24400529595486020, -24.65555945140047811, 68.31122994652405112 ) ) ;
#5404 = CARTESIAN_POINT ( 'NONE',  ( 2.789999999999999147, 23.53611639059710114, 19.35207786518998319 ) ) ;
#5405=STYLED_ITEM('',(#35254),#100);
#5406 = CARTESIAN_POINT ( 'NONE',  ( 100.1361914745664592, -3.050121699374163331, -12.12320065612944120 ) ) ;
#5407 = CARTESIAN_POINT ( 'NONE',  ( -35.00000000000000000, 16.36947364650383818, -36.69637551990492597 ) ) ;
#5408 = EDGE_LOOP ( 'NONE', ( #26039, #23272, #28643, #17954 ) ) ;
#5409 = CARTESIAN_POINT ( 'NONE',  ( -35.00000000000000000, -14.38258422898375066, 68.31122994652405112 ) ) ;
#5410 = PLANE ( 'NONE',  #30667 ) ;
#5411 = ORIENTED_EDGE ( 'NONE', *, *, #4592, .T. ) ;
#5412 = LINE ( 'NONE', #21277, #15665 ) ;
#5413 = DIRECTION ( 'NONE',  ( 0.000000000000000000, 7.888609052210118054E-31, 1.000000000000000000 ) ) ;
#5414 = LINE ( 'NONE', #32645, #3008 ) ;
#5415 = DIRECTION ( 'NONE',  ( 1.000000000000000000, 0.000000000000000000, 0.000000000000000000 ) ) ;
#5416 = VERTEX_POINT ( 'NONE', #19335 ) ;
#5417 = CIRCLE ( 'NONE', #7674, 3.999999999999976019 ) ;
#5418 = ADVANCED_FACE ( 'NONE', ( #33007 ), #32669, .F. ) ;
#5419 = EDGE_CURVE ( 'NONE', #14420, #16320, #7231, .T. ) ;
#5420 = FACE_OUTER_BOUND ( 'NONE', #14418, .T. ) ;
#5421 = ORIENTED_EDGE ( 'NONE', *, *, #19538, .T. ) ;
#5422 = DIRECTION ( 'NONE',  ( -3.469446951953832974E-18, -1.000000000000000000, -7.888609052210116302E-31 ) ) ;
#5423 = AXIS2_PLACEMENT_3D ( 'NONE', #25512, #4838, #20707 ) ;
#5424 = LINE ( 'NONE', #26796, #17129 ) ;
#5425 = ORIENTED_EDGE ( 'NONE', *, *, #18757, .F. ) ;
#5426 = DIRECTION ( 'NONE',  ( -1.000000000000000000, 0.000000000000000000, 0.000000000000000000 ) ) ;
#5427 = LINE ( 'NONE', #16318, #2918 ) ;
#5428 = TOROIDAL_SURFACE ( 'NONE', #35006, 30.47050528711512030, 8.000000000000000000 ) ;
#5429 = EDGE_LOOP ( 'NONE', ( #11822, #19601, #33767, #9833 ) ) ;
#5430 = EDGE_CURVE ( 'NONE', #31108, #13597, #16673, .T. ) ;
#5431 = ORIENTED_EDGE ( 'NONE', *, *, #19622, .T. ) ;
#5432 = LINE ( 'NONE', #10794, #20343 ) ;
#5433 = CARTESIAN_POINT ( 'NONE',  ( -109.8376268937510218, 1.695881020439944598, 7.312931660397135047 ) ) ;
#5434 = VERTEX_POINT ( 'NONE', #22351 ) ;
#5435 = ORIENTED_EDGE ( 'NONE', *, *, #1313, .T. ) ;
#5436 = DIRECTION ( 'NONE',  ( 0.000000000000000000, 0.000000000000000000, -1.000000000000000000 ) ) ;
#5437 = EDGE_CURVE ( 'NONE', #28097, #33936, #14665, .T. ) ;
#5438 = EDGE_CURVE ( 'NONE', #14972, #26158, #5526, .T. ) ;
#5439 = CARTESIAN_POINT ( 'NONE',  ( 0.000000000000000000, -11.69134295108991672, -6.750000000000007105 ) ) ;
#5440 = ADVANCED_FACE ( 'NONE', ( #5955 ), #24299, .T. ) ;
#5441 = VECTOR ( 'NONE', #26421, 1000.000000000000000 ) ;
#5442 = LINE ( 'NONE', #16331, #4944 ) ;
#5443 = DIRECTION ( 'NONE',  ( 0.000000000000000000, 0.000000000000000000, 1.000000000000000000 ) ) ;
#5444 = ORIENTED_EDGE ( 'NONE', *, *, #8008, .F. ) ;
#5445 = ORIENTED_EDGE ( 'NONE', *, *, #19569, .F. ) ;
#5446 = CARTESIAN_POINT ( 'NONE',  ( 3.985664461616347742E-15, 32.54542015209057126, 87.50000000000000000 ) ) ;
#5447 = DIRECTION ( 'NONE',  ( 0.000000000000000000, 0.000000000000000000, -1.000000000000000000 ) ) ;
#5448 = CARTESIAN_POINT ( 'NONE',  ( -12.00000000000001066, 124.9999999999999716, 155.0000000000000000 ) ) ;
#5449 = AXIS2_PLACEMENT_3D ( 'NONE', #24323, #11060, #18497 ) ;
#5450 = EDGE_CURVE ( 'NONE', #4470, #27012, #2941, .T. ) ;
#5451 = CARTESIAN_POINT ( 'NONE',  ( -20.00000000000007461, -109.0000000000000142, -187.0000000000000000 ) ) ;
#5452 = DIRECTION ( 'NONE',  ( -1.292961597001347186E-16, 0.000000000000000000, 1.000000000000000000 ) ) ;
#5453 = CARTESIAN_POINT ( 'NONE',  ( 1.395000000000002238, -30.02688531850407827, 16.81585001935568968 ) ) ;
#5454 = LINE ( 'NONE', #2787, #11229 ) ;
#5455 = LINE ( 'NONE', #13653, #3899 ) ;
#5456 = ORIENTED_EDGE ( 'NONE', *, *, #15677, .F. ) ;
#5457 = CIRCLE ( 'NONE', #28213, 3.999999999999976019 ) ;
#5458 = CARTESIAN_POINT ( 'NONE',  ( 29.82459402470852083, -33.69708579775584667, 87.50000000000000000 ) ) ;
#5459 = CARTESIAN_POINT ( 'NONE',  ( -12.00000000000001066, -124.9999999999999432, -186.9999999999999716 ) ) ;
#5460 = FACE_OUTER_BOUND ( 'NONE', #18521, .T. ) ;
#5461 = VERTEX_POINT ( 'NONE', #16740 ) ;
#5462 = AXIS2_PLACEMENT_3D ( 'NONE', #999, #17398, #9009 ) ;
#5463 = EDGE_CURVE ( 'NONE', #24766, #23118, #5432, .T. ) ;
#5464 = DIRECTION ( 'NONE',  ( 0.000000000000000000, 0.000000000000000000, -1.000000000000000000 ) ) ;
#5465 = ORIENTED_EDGE ( 'NONE', *, *, #22209, .F. ) ;
#5466 = CARTESIAN_POINT ( 'NONE',  ( -100.1508892704537459, 1.661471846880724357, -12.39299840842996048 ) ) ;
#5467 = CARTESIAN_POINT ( 'NONE',  ( 5.713835024271039842, 32.03991982186465748, 68.31122994652405112 ) ) ;
#5468 = VECTOR ( 'NONE', #1267, 1000.000000000000000 ) ;
#5469 = EDGE_LOOP ( 'NONE', ( #19997, #26673, #24979, #2826, #6751, #19896 ) ) ;
#5470 = CARTESIAN_POINT ( 'NONE',  ( -36.04853892210773836, 11.59936550071288330, -36.68877005347593467 ) ) ;
#5471 = LINE ( 'NONE', #27021, #3709 ) ;
#5472 = FACE_OUTER_BOUND ( 'NONE', #11128, .T. ) ;
#5473 = ORIENTED_EDGE ( 'NONE', *, *, #17425, .T. ) ;
#5474 = VERTEX_POINT ( 'NONE', #30175 ) ;
#5475 = DIRECTION ( 'NONE',  ( -7.893605728314050488E-14, 1.618803117314786135E-15, 0.9999999999999998890 ) ) ;
#5476 = DIRECTION ( 'NONE',  ( -1.000000000000000000, 0.000000000000000000, -1.300283923313630633E-47 ) ) ;
#5477 = EDGE_LOOP ( 'NONE', ( #32552, #10131, #15350, #5421 ) ) ;
#5478 = CYLINDRICAL_SURFACE ( 'NONE', #17525, 16.19999999999999574 ) ;
#5479 = EDGE_CURVE ( 'NONE', #8317, #33041, #27152, .T. ) ;
#5480 = EDGE_CURVE ( 'NONE', #13630, #18484, #19768, .T. ) ;
#5481 = CARTESIAN_POINT ( 'NONE',  ( 2.765921099433443331, 14.63235270440974922, -27.43224275967423509 ) ) ;
#5482 = CARTESIAN_POINT ( 'NONE',  ( -110.0713174531508827, -0.6892679340434131330, 7.470251853870532699 ) ) ;
#5483 = CONTEXT_DEPENDENT_SHAPE_REPRESENTATION ( #34430, #8879 ) ;
#5484 = EDGE_LOOP ( 'NONE', ( #9410, #876, #3181, #34065, #28483, #23898 ) ) ;
#5485 = EDGE_LOOP ( 'NONE', ( #33883, #463, #4459, #12787, #9206, #9659 ) ) ;
#5486 = CARTESIAN_POINT ( 'NONE',  ( -355.0000000000000000, -131.0000000000000000, 126.0000000000000000 ) ) ;
#5487 = AXIS2_PLACEMENT_3D ( 'NONE', #27970, #19804, #14107 ) ;
#5488 = CARTESIAN_POINT ( 'NONE',  ( -418.0000000000000568, -105.0000000000000142, 100.0000000000000000 ) ) ;
#5489 = VECTOR ( 'NONE', #22593, 1000.000000000000000 ) ;
#5490 = CARTESIAN_POINT ( 'NONE',  ( 1.749999999999999778, -10.37741591188916424, 32.81304455236865181 ) ) ;
#5491 = EDGE_LOOP ( 'NONE', ( #3395, #33863, #30225, #21326 ) ) ;
#5492 = ORIENTED_EDGE ( 'NONE', *, *, #23666, .F. ) ;
#5493 = CARTESIAN_POINT ( 'NONE',  ( -361.0000000000000000, 134.9999999999999716, 110.0000000000000000 ) ) ;
#5494 = ORIENTED_EDGE ( 'NONE', *, *, #66, .F. ) ;
#5495 = CARTESIAN_POINT ( 'NONE',  ( -418.0000000000000000, 105.0000000000000000, 132.0000000000000000 ) ) ;
#5496 = CARTESIAN_POINT ( 'NONE',  ( -12.00000000000001066, 144.9999999999999716, -186.9999999999999716 ) ) ;
#5497 = ORIENTED_EDGE ( 'NONE', *, *, #4162, .F. ) ;
#5498 = ORIENTED_EDGE ( 'NONE', *, *, #28764, .T. ) ;
#5499 = DIRECTION ( 'NONE',  ( 0.000000000000000000, 0.000000000000000000, -1.000000000000000000 ) ) ;
#5500 = DIRECTION ( 'NONE',  ( 4.043477172016626614E-17, 0.000000000000000000, 1.000000000000000000 ) ) ;
#5501 = ORIENTED_EDGE ( 'NONE', *, *, #11064, .T. ) ;
#5502 = LINE ( 'NONE', #32743, #3291 ) ;
#5503 = CARTESIAN_POINT ( 'NONE',  ( 8.000000000000000000, 0.000000000000000000, 0.000000000000000000 ) ) ;
#5504 = DIRECTION ( 'NONE',  ( 0.000000000000000000, -1.000000000000000000, -2.465190328815662439E-32 ) ) ;
#5505 = CARTESIAN_POINT ( 'NONE',  ( 2.789999999999999147, 27.60935207499552035, 12.89090262359662731 ) ) ;
#5506 = CARTESIAN_POINT ( 'NONE',  ( 0.02407890056655825201, -17.95514392185434360, 25.38201125280350468 ) ) ;
#5507 = CARTESIAN_POINT ( 'NONE',  ( -70.00000000000000000, 75.55999999999990280, -172.9900000000000091 ) ) ;
#5508 = SURFACE_STYLE_FILL_AREA ( #13716 ) ;
#5509 = AXIS2_PLACEMENT_3D ( 'NONE', #14246, #9067, #22420 ) ;
#5510 = VECTOR ( 'NONE', #5792, 1000.000000000000000 ) ;
#5511 = CIRCLE ( 'NONE', #2121, 7.999999999999979572 ) ;
#5512 = VERTEX_POINT ( 'NONE', #22000 ) ;
#5513 = CARTESIAN_POINT ( 'NONE',  ( 12.00000000000003908, -55.00000000000000711, -158.9999999999999716 ) ) ;
#5514 = DIRECTION ( 'NONE',  ( 0.000000000000000000, 0.000000000000000000, -1.000000000000000000 ) ) ;
#5515 = VERTEX_POINT ( 'NONE', #24833 ) ;
#5516 = EDGE_LOOP ( 'NONE', ( #5786, #23663, #33910, #4036 ) ) ;
#5517 = EDGE_CURVE ( 'NONE', #14714, #6804, #6686, .T. ) ;
#5518 = EDGE_CURVE ( 'NONE', #12319, #2702, #25436, .T. ) ;
#5519 = DIRECTION ( 'NONE',  ( -1.000000000000000000, 0.000000000000000000, 0.000000000000000000 ) ) ;
#5520 = ORIENTED_EDGE ( 'NONE', *, *, #6405, .F. ) ;
#5521 = ADVANCED_FACE ( 'NONE', ( #6502 ), #23247, .T. ) ;
#5522 = CARTESIAN_POINT ( 'NONE',  ( 2.765921099433441110, -17.95514392185398833, -25.38201125280375692 ) ) ;
#5523 = FILL_AREA_STYLE_COLOUR ( '', #1087 ) ;
#5524 = CONTEXT_DEPENDENT_SHAPE_REPRESENTATION ( #32860, #7290 ) ;
#5525 = CARTESIAN_POINT ( 'NONE',  ( 0.000000000000000000, 3.524919873834583163E-15, 68.31122994652405112 ) ) ;
#5526 = CIRCLE ( 'NONE', #32823, 2.033421858999711951 ) ;
#5527 = ORIENTED_EDGE ( 'NONE', *, *, #22904, .T. ) ;
#5528 = ORIENTED_EDGE ( 'NONE', *, *, #24153, .F. ) ;
#5529 = CYLINDRICAL_SURFACE ( 'NONE', #28778, 2.036051781435508801 ) ;
#5530 = CARTESIAN_POINT ( 'NONE',  ( 110.7380848894536598, -4.118294838564020743E-16, 7.500000000000000000 ) ) ;
#5531 = DIRECTION ( 'NONE',  ( -0.000000000000000000, -0.000000000000000000, -1.000000000000000000 ) ) ;
#5532 = CARTESIAN_POINT ( 'NONE',  ( 145.0000000000000568, -78.33668825982573480, -65.00000000000000000 ) ) ;
#5533 = PLANE ( 'NONE',  #18277 ) ;
#5534 = ORIENTED_EDGE ( 'NONE', *, *, #26429, .F. ) ;
#5536 = AXIS2_PLACEMENT_3D ( 'NONE', #7872, #21407, #21746 ) ;
#5535 = CARTESIAN_POINT ( 'NONE',  ( -430.0000000000000000, 130.9999999999999716, 126.0000000000000000 ) ) ;
#5537 = CARTESIAN_POINT ( 'NONE',  ( 2.765921099433443331, -29.68817180695682723, 9.232883799364120847 ) ) ;
#5538 = DIRECTION ( 'NONE',  ( 0.000000000000000000, 0.000000000000000000, -1.000000000000000000 ) ) ;
#5539 = CARTESIAN_POINT ( 'NONE',  ( 1.040000000000000480, -10.89151784028265979, -32.64600270996228204 ) ) ;
#5540 = DIRECTION ( 'NONE',  ( -1.000000000000000000, 0.000000000000000000, 0.000000000000000000 ) ) ;
#5541 = FACE_OUTER_BOUND ( 'NONE', #11820, .T. ) ;
#5542 = AXIS2_PLACEMENT_3D ( 'NONE', #15582, #28924, #1863 ) ;
#5544 = CARTESIAN_POINT ( 'NONE',  ( -100.0603537787683592, 1.371756618311863685, -7.381329779211299957 ) ) ;
#5543 = CARTESIAN_POINT ( 'NONE',  ( -418.0000000000000000, 105.0000000000000000, -73.99999999999998579 ) ) ;
#5545 = FACE_OUTER_BOUND ( 'NONE', #20152, .T. ) ;
#5546 = ORIENTED_EDGE ( 'NONE', *, *, #16139, .F. ) ;
#5547 = CARTESIAN_POINT ( 'NONE',  ( -499.9999999999999432, 144.9999999999999716, 187.0000000000000000 ) ) ;
#5549 = DIRECTION ( 'NONE',  ( 0.000000000000000000, -1.000000000000000000, -3.374343856708137958E-53 ) ) ;
#5548 = DIRECTION ( 'NONE',  ( -1.000000000000000000, 0.000000000000000000, -0.000000000000000000 ) ) ;
#5550 = VECTOR ( 'NONE', #14317, 1000.000000000000227 ) ;
#5551 = VERTEX_POINT ( 'NONE', #3658 ) ;
#5552 = ADVANCED_FACE ( 'NONE', ( #23077 ), #22725, .T. ) ;
#5553 = ORIENTED_EDGE ( 'NONE', *, *, #15657, .F. ) ;
#5554 = EDGE_CURVE ( 'NONE', #474, #20668, #12228, .T. ) ;
#5555 = AXIS2_PLACEMENT_3D ( 'NONE', #22263, #8726, #6044 ) ;
#5556 =( REPRESENTATION_RELATIONSHIP ('NONE','NONE', #23037, #28231 ) REPRESENTATION_RELATIONSHIP_WITH_TRANSFORMATION ( #30313 )SHAPE_REPRESENTATION_RELATIONSHIP( ) );
#5557 = VECTOR ( 'NONE', #11203, 1000.000000000000000 ) ;
#5558 = ORIENTED_EDGE ( 'NONE', *, *, #6742, .F. ) ;
#5559 = CARTESIAN_POINT ( 'NONE',  ( -442.0000000000000000, -105.0000000000000142, -174.9999999999999716 ) ) ;
#5560 = ORIENTED_EDGE ( 'NONE', *, *, #30163, .T. ) ;
#5561 = EDGE_LOOP ( 'NONE', ( #16389, #21797, #33200, #25822, #29105, #1669 ) ) ;
#5562 = ADVANCED_FACE ( 'NONE', ( #25373 ), #33920, .T. ) ;
#5563 = CARTESIAN_POINT ( 'NONE',  ( -442.0000000000000000, -112.9999999999999858, -155.0000000000000000 ) ) ;
#5564 = CIRCLE ( 'NONE', #30034, 30.47050528711511674 ) ;
#5565 = DIRECTION ( 'NONE',  ( 0.000000000000000000, 0.000000000000000000, 1.000000000000000000 ) ) ;
#5566 = DIRECTION ( 'NONE',  ( 0.000000000000000000, 0.000000000000000000, 1.000000000000000000 ) ) ;
#5567 = ORIENTED_EDGE ( 'NONE', *, *, #20376, .F. ) ;
#5568 = EDGE_CURVE ( 'NONE', #19338, #13474, #34088, .T. ) ;
#5569 = VERTEX_POINT ( 'NONE', #28408 ) ;
#5570 = DIRECTION ( 'NONE',  ( -0.9476531711828030113, -0.3193015301359780622, 0.000000000000000000 ) ) ;
#5571 = SURFACE_STYLE_FILL_AREA ( #16291 ) ;
#5572 = EDGE_CURVE ( 'NONE', #16565, #31475, #28582, .T. ) ;
#5573 = CARTESIAN_POINT ( 'NONE',  ( 99.56179722369340368, -1.869077253746796785, -12.36451290817385917 ) ) ;
#5574 = DIRECTION ( 'NONE',  ( -1.000000000000000000, -0.000000000000000000, -0.000000000000000000 ) ) ;
#5575 = ORIENTED_EDGE ( 'NONE', *, *, #17635, .T. ) ;
#5576 = EDGE_CURVE ( 'NONE', #12309, #23161, #6681, .T. ) ;
#5577 = CARTESIAN_POINT ( 'NONE',  ( -499.9999999999999432, 112.9999999999999574, 155.0000000000000000 ) ) ;
#5578 = VECTOR ( 'NONE', #23841, 1000.000000000000000 ) ;
#5579 = CARTESIAN_POINT ( 'NONE',  ( 1.039999999999999813, -30.02688531850407117, 16.81585001935569323 ) ) ;
#5580 = ORIENTED_EDGE ( 'NONE', *, *, #30823, .F. ) ;
#5581 = DIRECTION ( 'NONE',  ( -0.7960930657056438653, -0.6051742151937650194, -1.111686998345334199E-16 ) ) ;
#5582 = DIRECTION ( 'NONE',  ( 0.000000000000000000, -1.000000000000000000, -2.465190328815662439E-32 ) ) ;
#5583 = DIRECTION ( 'NONE',  ( -0.000000000000000000, 1.836970198721029934E-16, -1.000000000000000000 ) ) ;
#5584 = CARTESIAN_POINT ( 'NONE',  ( -17.07420202168509604, 33.79163469797341435, 68.31122994652405112 ) ) ;
#5585 = DIRECTION ( 'NONE',  ( 0.000000000000000000, 0.000000000000000000, -1.000000000000000000 ) ) ;
#5586 = AXIS2_PLACEMENT_3D ( 'NONE', #15098, #18300, #1898 ) ;
#5587 = PLANE ( 'NONE',  #24074 ) ;
#5588 = ORIENTED_EDGE ( 'NONE', *, *, #32376, .T. ) ;
#5590 = CARTESIAN_POINT ( 'NONE',  ( 0.5288002523874972827, 21.87231946537524152, -25.22857168675658812 ) ) ;
#5589 = DIRECTION ( 'NONE',  ( 1.000000000000000000, 0.000000000000000000, 0.000000000000000000 ) ) ;
#5591 = CYLINDRICAL_SURFACE ( 'NONE', #25040, 4.309328216469825001 ) ;
#5592 = CIRCLE ( 'NONE', #15308, 30.47050528711511674 ) ;
#5593 = VERTEX_POINT ( 'NONE', #11876 ) ;
#5594 = CARTESIAN_POINT ( 'NONE',  ( -347.0000000000000000, 124.9999999999999432, 181.0000000000000000 ) ) ;
#5595 = DIRECTION ( 'NONE',  ( 0.000000000000000000, 0.000000000000000000, 1.000000000000000000 ) ) ;
#5596 = ORIENTED_EDGE ( 'NONE', *, *, #11618, .F. ) ;
#5597 = CIRCLE ( 'NONE', #24946, 7.999999999999992895 ) ;
#5598 = ORIENTED_EDGE ( 'NONE', *, *, #34641, .T. ) ;
#5599 = CARTESIAN_POINT ( 'NONE',  ( -499.9999999999999432, 108.9999999999999858, 162.9999999999999716 ) ) ;
#5600 = LINE ( 'NONE', #35010, #28957 ) ;
#5601 = ORIENTED_EDGE ( 'NONE', *, *, #31868, .T. ) ;
#5602 = ORIENTED_EDGE ( 'NONE', *, *, #3405, .F. ) ;
#5603 = DIRECTION ( 'NONE',  ( 1.000000000000000000, 0.000000000000000000, 0.000000000000000000 ) ) ;
#5604 = EDGE_CURVE ( 'NONE', #7246, #29898, #14547, .T. ) ;
#5605 = CARTESIAN_POINT ( 'NONE',  ( -355.0000000000000000, -135.0000000000000000, 126.0000000000000000 ) ) ;
#5606 = VECTOR ( 'NONE', #19875, 1000.000000000000000 ) ;
#5607 = CARTESIAN_POINT ( 'NONE',  ( 4.815661544189684840, -32.18716788982705168, 68.31122994652405112 ) ) ;
#5608 = DIRECTION ( 'NONE',  ( 3.697785493223492838E-32, 1.934419779023891545E-16, -1.000000000000000000 ) ) ;
#5609 = EDGE_CURVE ( 'NONE', #11612, #24525, #28749, .T. ) ;
#5610 = EDGE_LOOP ( 'NONE', ( #21331, #15365, #15943, #18376 ) ) ;
#5611 = EDGE_CURVE ( 'NONE', #16642, #5950, #25729, .T. ) ;
#5612 = ORIENTED_EDGE ( 'NONE', *, *, #19594, .T. ) ;
#5613 = PLANE ( 'NONE',  #10544 ) ;
#5614 = CARTESIAN_POINT ( 'NONE',  ( -500.0000000000000000, -113.0000000000000000, 162.9999999999999716 ) ) ;
#5615 = CARTESIAN_POINT ( 'NONE',  ( 20.89386240318430055, 24.95297350523386015, 68.31122994652405112 ) ) ;
#5616 = DIRECTION ( 'NONE',  ( 1.000000000000000000, 0.000000000000000000, 0.000000000000000000 ) ) ;
#5617 = CIRCLE ( 'NONE', #20986, 2.085824230283342740 ) ;
#5618 = DIRECTION ( 'NONE',  ( 0.000000000000000000, 1.836970198721029441E-16, -1.000000000000000000 ) ) ;
#5619 = LINE ( 'NONE', #21658, #32253 ) ;
#5620 = DIRECTION ( 'NONE',  ( 1.000000000000000000, -0.000000000000000000, -0.000000000000000000 ) ) ;
#5621 = ORIENTED_EDGE ( 'NONE', *, *, #24211, .T. ) ;
#5622 = CARTESIAN_POINT ( 'NONE',  ( 2.789999999999999147, -8.813854705727257155, -29.13568936554952060 ) ) ;
#5623 = DIRECTION ( 'NONE',  ( 0.1081190184239420177, 0.9941379571543595972, -0.000000000000000000 ) ) ;
#5624 = EDGE_CURVE ( 'NONE', #17462, #1337, #3834, .T. ) ;
#5625 = DIRECTION ( 'NONE',  ( 1.848892746611746419E-32, 6.842277657836020854E-49, -1.000000000000000000 ) ) ;
#5626 = ORIENTED_EDGE ( 'NONE', *, *, #10438, .F. ) ;
#5627 = AXIS2_PLACEMENT_3D ( 'NONE', #18578, #10553, #5010 ) ;
#5628 = CARTESIAN_POINT ( 'NONE',  ( -70.00000000000000000, 75.55999999999990280, 172.9900000000000091 ) ) ;
#5629 = VERTEX_POINT ( 'NONE', #20404 ) ;
#5630 = FACE_OUTER_BOUND ( 'NONE', #3355, .T. ) ;
#5631 = CARTESIAN_POINT ( 'NONE',  ( -100.4147610035674916, 2.273103392716669724, -12.29250028061669120 ) ) ;
#5632 = EDGE_CURVE ( 'NONE', #15054, #29695, #4949, .T. ) ;
#5633 = ADVANCED_FACE ( 'NONE', ( #33560 ), #4178, .T. ) ;
#5634 = ADVANCED_FACE ( 'NONE', ( #3829 ), #9183, .F. ) ;
#5635 = ORIENTED_EDGE ( 'NONE', *, *, #13751, .F. ) ;
#5636 = DIRECTION ( 'NONE',  ( -1.000000000000000000, 0.000000000000000000, 0.000000000000000000 ) ) ;
#5637 = CARTESIAN_POINT ( 'NONE',  ( 3.235562306570555532E-30, 24.02303923978504940, -67.50000000000000000 ) ) ;
#5638 = DIRECTION ( 'NONE',  ( 0.000000000000000000, 0.000000000000000000, 1.000000000000000000 ) ) ;
#5639 = EDGE_CURVE ( 'NONE', #26315, #22871, #14895, .T. ) ;
#5640 = ORIENTED_EDGE ( 'NONE', *, *, #13661, .T. ) ;
#5641 = VECTOR ( 'NONE', #9485, 1000.000000000000000 ) ;
#5642 = ORIENTED_EDGE ( 'NONE', *, *, #23617, .T. ) ;
#5643 = DIRECTION ( 'NONE',  ( 0.1063910735369155841, -0.9943243633099125844, -3.335902418025060287E-15 ) ) ;
#5644 = DIRECTION ( 'NONE',  ( 0.000000000000000000, 1.836970198721029688E-16, -1.000000000000000000 ) ) ;
#5645 = VERTEX_POINT ( 'NONE', #1355 ) ;
#5646 = CARTESIAN_POINT ( 'NONE',  ( 0.7561992215529863559, 27.12277411069277377, -20.36158770325022260 ) ) ;
#5647 = CARTESIAN_POINT ( 'NONE',  ( 32.54460952423470133, 0.2297037030477266373, 68.31122994652405112 ) ) ;
#5648 = VECTOR ( 'NONE', #5531, 1000.000000000000000 ) ;
#5649 = PLANE ( 'NONE',  #8796 ) ;
#5650 = CARTESIAN_POINT ( 'NONE',  ( -99.88497961182920903, -0.3503014826537200754, 7.499999999999999112 ) ) ;
#5651 = ITEM_DEFINED_TRANSFORMATION ( 'NONE', 'NONE', #20662,  #28566 ) ;
#5652 = ADVANCED_FACE ( 'NONE', ( #8388 ), #13088, .F. ) ;
#5653 = ORIENTED_EDGE ( 'NONE', *, *, #7415, .F. ) ;
#5654 = EDGE_CURVE ( 'NONE', #12217, #29695, #28923, .T. ) ;
#5655 = EDGE_LOOP ( 'NONE', ( #14366, #24253, #22758, #20656 ) ) ;
#5656 = ORIENTED_EDGE ( 'NONE', *, *, #23486, .T. ) ;
#5657 = LINE ( 'NONE', #13521, #21435 ) ;
#5658 = LINE ( 'NONE', #32062, #17725 ) ;
#5659 = DIRECTION ( 'NONE',  ( 0.000000000000000000, 0.000000000000000000, 1.000000000000000000 ) ) ;
#5660 = ORIENTED_EDGE ( 'NONE', *, *, #4044, .F. ) ;
#5661 = EDGE_LOOP ( 'NONE', ( #21149, #5062 ) ) ;
#5662 = CARTESIAN_POINT ( 'NONE',  ( -499.9999999999999432, -137.0000000000000000, -162.9999999999999716 ) ) ;
#5663 = ORIENTED_EDGE ( 'NONE', *, *, #28958, .F. ) ;
#5664 = LINE ( 'NONE', #7995, #13629 ) ;
#5665 = DIRECTION ( 'NONE',  ( 1.000000000000000000, 0.000000000000000000, 0.000000000000000000 ) ) ;
#5666 = EDGE_LOOP ( 'NONE', ( #10450, #18151, #22236, #1603 ) ) ;
#5667 = AXIS2_PLACEMENT_3D ( 'NONE', #26504, #4590, #34162 ) ;
#5668 = ORIENTED_EDGE ( 'NONE', *, *, #22792, .F. ) ;
#5669 = FACE_OUTER_BOUND ( 'NONE', #4573, .T. ) ;
#5670 = CARTESIAN_POINT ( 'NONE',  ( -19.99999999999998934, -124.9999999999999432, -162.9999999999999432 ) ) ;
#5671 = VERTEX_POINT ( 'NONE', #29456 ) ;
#5672 = FACE_OUTER_BOUND ( 'NONE', #17156, .T. ) ;
#5673 = CARTESIAN_POINT ( 'NONE',  ( -499.9999999999999432, 136.9999999999999432, 187.0000000000000000 ) ) ;
#5674 = DIRECTION ( 'NONE',  ( 0.000000000000000000, 0.000000000000000000, 1.000000000000000000 ) ) ;
#5675 = EDGE_CURVE ( 'NONE', #12264, #29470, #27699, .T. ) ;
#5676 = CARTESIAN_POINT ( 'NONE',  ( 1.749999999999999778, -2.430610048906265419, 34.32897884578299852 ) ) ;
#5677 = EDGE_CURVE ( 'NONE', #30602, #21957, #20746, .T. ) ;
#5678 = LINE ( 'NONE', #2494, #22243 ) ;
#5679 = CARTESIAN_POINT ( 'NONE',  ( 15.99999999999998579, 4.559999999999908127, 172.9900000000000091 ) ) ;
#5680 =( NAMED_UNIT ( * ) SI_UNIT ( $, .STERADIAN. ) SOLID_ANGLE_UNIT ( ) );
#5681 = EDGE_CURVE ( 'NONE', #24390, #7431, #1562, .T. ) ;
#5682 = VERTEX_POINT ( 'NONE', #30102 ) ;
#5683 = DIRECTION ( 'NONE',  ( 0.000000000000000000, 1.836970198721029688E-16, -1.000000000000000000 ) ) ;
#5684 = DIRECTION ( 'NONE',  ( 0.1063910735368947813, -0.9943243633099144718, -3.335902418024520312E-15 ) ) ;
#5685 = ADVANCED_FACE ( 'NONE', ( #26246 ), #32763, .F. ) ;
#5686 = ORIENTED_EDGE ( 'NONE', *, *, #19932, .F. ) ;
#5687 = EDGE_LOOP ( 'NONE', ( #9570, #28, #3639, #21966, #13053, #19672, #1830, #5732 ) ) ;
#5688 = AXIS2_PLACEMENT_3D ( 'NONE', #25048, #691, #6543 ) ;
#5689 = CARTESIAN_POINT ( 'NONE',  ( 101.2209703486791881, 4.332787265952012135, 6.129206022554251732 ) ) ;
#5690 = ITEM_DEFINED_TRANSFORMATION ( 'NONE', 'NONE', #19505,  #28566 ) ;
#5691 = ORIENTED_EDGE ( 'NONE', *, *, #2202, .T. ) ;
#5692 = CARTESIAN_POINT ( 'NONE',  ( 0.000000000000000000, 0.000000000000000000, 0.000000000000000000 ) ) ;
#5693 = DIRECTION ( 'NONE',  ( 0.000000000000000000, -1.000000000000000000, -1.131431318426415506E-52 ) ) ;
#5695 = DIRECTION ( 'NONE',  ( -1.000000000000000000, 0.000000000000000000, 0.000000000000000000 ) ) ;
#5694 = LINE ( 'NONE', #23407, #24679 ) ;
#5697 = ORIENTED_EDGE ( 'NONE', *, *, #24499, .T. ) ;
#5696 = CIRCLE ( 'NONE', #15472, 2.036051781435517682 ) ;
#5698 = ORIENTED_EDGE ( 'NONE', *, *, #27195, .T. ) ;
#5699 = DIRECTION ( 'NONE',  ( 3.697785493223492838E-32, 1.934419779023891545E-16, -1.000000000000000000 ) ) ;
#5701 = EDGE_CURVE ( 'NONE', #15650, #26161, #31757, .T. ) ;
#5700 = DIRECTION ( 'NONE',  ( -1.000000000000000000, 0.000000000000000000, -1.300283923313630633E-47 ) ) ;
#5702 = CARTESIAN_POINT ( 'NONE',  ( 0.7564103365129547507, 13.95893286369010688, 30.90974742850075074 ) ) ;
#5703 = DIRECTION ( 'NONE',  ( -0.9985334138511239299, 0.05413890858541753337, 0.000000000000000000 ) ) ;
#5704 = CARTESIAN_POINT ( 'NONE',  ( 5.021133111224265200, -11.61907005722761532, -67.50000000000000000 ) ) ;
#5705 = ORIENTED_EDGE ( 'NONE', *, *, #16115, .F. ) ;
#5706 = DIRECTION ( 'NONE',  ( 1.000000000000000000, 0.000000000000000000, 1.300283923313630633E-47 ) ) ;
#5707 = LINE ( 'NONE', #8746, #14008 ) ;
#5708 = CARTESIAN_POINT ( 'NONE',  ( 145.0000000000000568, -90.42893218813456713, 44.81798139211241505 ) ) ;
#5709 = CIRCLE ( 'NONE', #6863, 2.033421858999711951 ) ;
#5710 = CARTESIAN_POINT ( 'NONE',  ( 53.89849999999999852, 0.000000000000000000, 8.000000000000000000 ) ) ;
#5711 = EDGE_CURVE ( 'NONE', #15141, #10000, #31677, .T. ) ;
#5712 = CARTESIAN_POINT ( 'NONE',  ( 1.040000000000002034, 6.714005886384948774, 33.75364837705175347 ) ) ;
#5713 = AXIS2_PLACEMENT_3D ( 'NONE', #20228, #30549, #3307 ) ;
#5714 = DIRECTION ( 'NONE',  ( 0.000000000000000000, 0.000000000000000000, 1.000000000000000000 ) ) ;
#5715 = EDGE_CURVE ( 'NONE', #34278, #5461, #21192, .T. ) ;
#5717 = CARTESIAN_POINT ( 'NONE',  ( -102.2775073974855644, 4.333302303957503376, -6.122453330911794112 ) ) ;
#5716 = CARTESIAN_POINT ( 'NONE',  ( 20.62763069236413926, -31.74750072459299588, 68.31122994652405112 ) ) ;
#5718 = EDGE_CURVE ( 'NONE', #4776, #3490, #5694, .T. ) ;
#5719 = CARTESIAN_POINT ( 'NONE',  ( 0.02407890056655521624, 28.29688452313399338, 12.88099432405614309 ) ) ;
#5720 = EDGE_LOOP ( 'NONE', ( #19462, #17581 ) ) ;
#5721 = CARTESIAN_POINT ( 'NONE',  ( 12.00000000000001066, -64.99999999999997158, 154.9999999999999716 ) ) ;
#5722 = PLANE ( 'NONE',  #1508 ) ;
#5723 = ORIENTED_EDGE ( 'NONE', *, *, #23863, .F. ) ;
#5724 = VECTOR ( 'NONE', #6985, 1000.000000000000000 ) ;
#5725 = DIRECTION ( 'NONE',  ( 0.000000000000000000, -1.000000000000000000, 0.000000000000000000 ) ) ;
#5726 = AXIS2_PLACEMENT_3D ( 'NONE', #23307, #1757, #12631 ) ;
#5727=STYLED_ITEM('',(#35275),#33706);
#5728 = VERTEX_POINT ( 'NONE', #34797 ) ;
#5729 = ORIENTED_EDGE ( 'NONE', *, *, #20886, .T. ) ;
#5730 = DIRECTION ( 'NONE',  ( 0.000000000000000000, -1.000000000000000000, -1.836970198721029688E-16 ) ) ;
#5731 = EDGE_LOOP ( 'NONE', ( #22281, #16856, #9079, #7898, #23020, #2800 ) ) ;
#5732 = ORIENTED_EDGE ( 'NONE', *, *, #34314, .T. ) ;
#5733 = CIRCLE ( 'NONE', #28502, 7.999999999999952038 ) ;
#5734 = DIRECTION ( 'NONE',  ( 0.000000000000000000, 0.000000000000000000, 1.000000000000000000 ) ) ;
#5735 = CIRCLE ( 'NONE', #12609, 7.500000000000000000 ) ;
#5736 = CYLINDRICAL_SURFACE ( 'NONE', #33979, 7.999999999999979572 ) ;
#5737 = LINE ( 'NONE', #16639, #22790 ) ;
#5738 = ORIENTED_EDGE ( 'NONE', *, *, #30830, .F. ) ;
#5739 = EDGE_LOOP ( 'NONE', ( #21856, #23526, #12653, #15325 ) ) ;
#5740 = CARTESIAN_POINT ( 'NONE',  ( 13.32059394339353986, -35.43959265050634144, 68.31122994652405112 ) ) ;
#5741 = CARTESIAN_POINT ( 'NONE',  ( -9.978866888775527855, 4.168562732279005090, -67.50000000000000000 ) ) ;
#5742 = CARTESIAN_POINT ( 'NONE',  ( 109.9606688226409119, -2.890043774996748027, -12.16248655421355451 ) ) ;
#5743 = LINE ( 'NONE', #8261, #17111 ) ;
#5744 = ORIENTED_EDGE ( 'NONE', *, *, #24115, .T. ) ;
#5745 = CARTESIAN_POINT ( 'NONE',  ( -19.99999999999998934, -137.0000000000000000, 159.0000000000000000 ) ) ;
#5746 = AXIS2_PLACEMENT_3D ( 'NONE', #13699, #29902, #5665 ) ;
#5747 = DIRECTION ( 'NONE',  ( 0.000000000000000000, 0.000000000000000000, 1.000000000000000000 ) ) ;
#5748 = ORIENTED_EDGE ( 'NONE', *, *, #17601, .T. ) ;
#5749 = VECTOR ( 'NONE', #34288, 1000.000000000000000 ) ;
#5750 = EDGE_CURVE ( 'NONE', #27942, #29489, #23002, .T. ) ;
#5751 = AXIS2_PLACEMENT_3D ( 'NONE', #4900, #15796, #10432 ) ;
#5752 = AXIS2_PLACEMENT_3D ( 'NONE', #5332, #16223, #27229 ) ;
#5753 = CYLINDRICAL_SURFACE ( 'NONE', #12901, 1.999999999999999556 ) ;
#5754 = DIRECTION ( 'NONE',  ( -0.000000000000000000, 1.836970198721029688E-16, -1.000000000000000000 ) ) ;
#5755 = EDGE_CURVE ( 'NONE', #3590, #7140, #27252, .T. ) ;
#5756 = DIRECTION ( 'NONE',  ( -0.000000000000000000, 1.000000000000000000, -0.000000000000000000 ) ) ;
#5757 = CARTESIAN_POINT ( 'NONE',  ( -365.0000000000000000, -117.0000000000000000, 113.9999999999999858 ) ) ;
#5758 = ORIENTED_EDGE ( 'NONE', *, *, #25395, .T. ) ;
#5759 = EDGE_CURVE ( 'NONE', #18227, #25758, #31927, .T. ) ;
#5760 = LINE ( 'NONE', #19500, #13854 ) ;
#5761 = VERTEX_POINT ( 'NONE', #15409 ) ;
#5762 = EDGE_CURVE ( 'NONE', #19390, #14536, #5344, .T. ) ;
#5764 =( LENGTH_UNIT ( ) NAMED_UNIT ( * ) SI_UNIT ( .MILLI., .METRE. ) );
#5763 = DIRECTION ( 'NONE',  ( -0.7259954919231307313, -0.6876994588534234287, 0.000000000000000000 ) ) ;
#5765 = ORIENTED_EDGE ( 'NONE', *, *, #11059, .T. ) ;
#5766 =( REPRESENTATION_RELATIONSHIP ('NONE','NONE', #23037, #15767 ) REPRESENTATION_RELATIONSHIP_WITH_TRANSFORMATION ( #22050 )SHAPE_REPRESENTATION_RELATIONSHIP( ) );
#5767 = DIRECTION ( 'NONE',  ( -0.9985334138511239299, 0.05413890858541762358, 0.000000000000000000 ) ) ;
#5768 = PRODUCT ( 'top shell', 'top shell', '', ( #13906 ) ) ;
#5769 = DIRECTION ( 'NONE',  ( 0.000000000000000000, 0.000000000000000000, 1.000000000000000000 ) ) ;
#5770 = ADVANCED_FACE ( 'NONE', ( #7543 ), #24568, .T. ) ;
#5771 = VERTEX_POINT ( 'NONE', #1862 ) ;
#5772 = ORIENTED_EDGE ( 'NONE', *, *, #11104, .F. ) ;
#5773 = AXIS2_PLACEMENT_3D ( 'NONE', #10296, #13502, #24337 ) ;
#5774 = CIRCLE ( 'NONE', #17209, 34.41491905851385269 ) ;
#5775 = VERTEX_POINT ( 'NONE', #34442 ) ;
#5776 = CARTESIAN_POINT ( 'NONE',  ( 1.749999999999999778, -18.66807150955433769, 28.91175816027496381 ) ) ;
#5777 = CARTESIAN_POINT ( 'NONE',  ( -101.8770720491269088, 4.063889691276224347, 6.307349793299453111 ) ) ;
#5778 = ORIENTED_EDGE ( 'NONE', *, *, #6154, .T. ) ;
#5779 = ORIENTED_EDGE ( 'NONE', *, *, #32383, .F. ) ;
#5780 = VECTOR ( 'NONE', #19721, 1000.000000000000000 ) ;
#5781 = DIRECTION ( 'NONE',  ( -1.000000000000000000, 0.000000000000000000, 0.000000000000000000 ) ) ;
#5782 = CARTESIAN_POINT ( 'NONE',  ( 11.99999999999999645, -124.9999999999999432, -154.9999999999999716 ) ) ;
#5783 = CARTESIAN_POINT ( 'NONE',  ( 2.033800782743256708, -24.35691930005240735, -23.60041548268739220 ) ) ;
#5784 = LINE ( 'NONE', #116, #10257 ) ;
#5785 = VERTEX_POINT ( 'NONE', #29094 ) ;
#5786 = ORIENTED_EDGE ( 'NONE', *, *, #3909, .F. ) ;
#5787 = CARTESIAN_POINT ( 'NONE',  ( -414.0000000000000568, -124.9999999999999716, 132.0000000000000000 ) ) ;
#5788 = LINE ( 'NONE', #120, #1038 ) ;
#5789 = DIRECTION ( 'NONE',  ( 0.000000000000000000, 0.000000000000000000, 1.000000000000000000 ) ) ;
#5790 = DIRECTION ( 'NONE',  ( 0.000000000000000000, 0.000000000000000000, -1.000000000000000000 ) ) ;
#5791 = CARTESIAN_POINT ( 'NONE',  ( -20.63749999999999929, 1.374666032042903655E-15, 11.22499999999999787 ) ) ;
#5792 = DIRECTION ( 'NONE',  ( -0.000000000000000000, -1.000000000000000000, -0.000000000000000000 ) ) ;
#5793 = DIRECTION ( 'NONE',  ( 1.000000000000000000, 0.000000000000000000, -0.000000000000000000 ) ) ;
#5794 = VERTEX_POINT ( 'NONE', #4689 ) ;
#5795 = DIRECTION ( 'NONE',  ( 1.000000000000000000, 3.040835319149746090E-31, 1.232595164407830946E-32 ) ) ;
#5796 = LINE ( 'NONE', #27178, #27948 ) ;
#5797 = EDGE_CURVE ( 'NONE', #8817, #11568, #19023, .T. ) ;
#5798 = VECTOR ( 'NONE', #23744, 1000.000000000000000 ) ;
#5799 = CARTESIAN_POINT ( 'NONE',  ( 0.5390048853417120922, 5.257018938344060643, -13.49999999999999645 ) ) ;
#5800 = EDGE_LOOP ( 'NONE', ( #421, #10683, #17475, #32735 ) ) ;
#5801 = B_SPLINE_CURVE_WITH_KNOTS ( 'NONE', 3,
 ( #23975, #34859, #10467, #21323 ),
 .UNSPECIFIED., .F., .F.,
 ( 4, 4 ),
 ( 4.077050493238099252E-07, 0.0006881451559005025012 ),
 .UNSPECIFIED. ) ;
#5802 = AXIS2_PLACEMENT_3D ( 'NONE', #15032, #34901, #5148 ) ;
#5803 = AXIS2_PLACEMENT_3D ( 'NONE', #2543, #21595, #18935 ) ;
#5804 = AXIS2_PLACEMENT_3D ( 'NONE', #13621, #11134, #32299 ) ;
#5805 = CARTESIAN_POINT ( 'NONE',  ( 127.4999999999999147, 0.000000000000000000, 12.50000000000000000 ) ) ;
#5806 = ORIENTED_EDGE ( 'NONE', *, *, #32929, .T. ) ;
#5807 = EDGE_CURVE ( 'NONE', #701, #30793, #816, .T. ) ;
#5808 = PLANE ( 'NONE',  #32666 ) ;
#5809 = CARTESIAN_POINT ( 'NONE',  ( -106.3372840774548536, 4.948560684155827616, 11.47897987543853837 ) ) ;
#5810 = EDGE_CURVE ( 'NONE', #6974, #18838, #5926, .T. ) ;
#5811 = ORIENTED_EDGE ( 'NONE', *, *, #12501, .T. ) ;
#5812 = ADVANCED_FACE ( 'NONE', ( #3565 ), #22273, .T. ) ;
#5813 = EDGE_CURVE ( 'NONE', #15484, #32236, #12770, .T. ) ;
#5814 = LINE ( 'NONE', #2631, #20020 ) ;
#5815 = DIRECTION ( 'NONE',  ( -1.000000000000000000, 0.000000000000000000, 0.000000000000000000 ) ) ;
#5816 = DIRECTION ( 'NONE',  ( 0.000000000000000000, 1.000000000000000000, 0.000000000000000000 ) ) ;
#5817 = ORIENTED_EDGE ( 'NONE', *, *, #23141, .F. ) ;
#5818 = DIRECTION ( 'NONE',  ( 0.1063910735369155841, -0.9943243633099125844, -3.335902418025060287E-15 ) ) ;
#5819 = DIRECTION ( 'NONE',  ( 0.000000000000000000, 0.9510565162951500895, 0.3090169943749579984 ) ) ;
#5820 = VERTEX_POINT ( 'NONE', #14272 ) ;
#5821 = DIRECTION ( 'NONE',  ( 1.000000000000000000, 0.000000000000000000, -0.000000000000000000 ) ) ;
#5822 = EDGE_CURVE ( 'NONE', #3430, #14410, #6588, .T. ) ;
#5823 = AXIS2_PLACEMENT_3D ( 'NONE', #11769, #14442, #22620 ) ;
#5824 = DIRECTION ( 'NONE',  ( -1.000000000000000000, 0.000000000000000000, 0.000000000000000000 ) ) ;
#5825 = CIRCLE ( 'NONE', #10390, 3.999999999999976019 ) ;
#5826 = DIRECTION ( 'NONE',  ( -0.9476531711828025673, -0.3193015301359797831, -5.865473952658197586E-17 ) ) ;
#5827 = CARTESIAN_POINT ( 'NONE',  ( -106.6861982456198916, -4.840385614786934632, 5.731315639859859701 ) ) ;
#5828 = CIRCLE ( 'NONE', #18942, 0.3000000000000016542 ) ;
#5829 = EDGE_LOOP ( 'NONE', ( #13908, #12301, #9272, #28673 ) ) ;
#5830 = VERTEX_POINT ( 'NONE', #25099 ) ;
#5831 = AXIS2_PLACEMENT_3D ( 'NONE', #17235, #17754, #15078 ) ;
#5832 = ORIENTED_EDGE ( 'NONE', *, *, #29290, .F. ) ;
#5833 = CARTESIAN_POINT ( 'NONE',  ( 0.000000000000000000, -29.00730259674847034, 9.328884633908835156 ) ) ;
#5834 = FACE_OUTER_BOUND ( 'NONE', #3454, .T. ) ;
#5835 = EDGE_CURVE ( 'NONE', #17427, #22841, #25836, .T. ) ;
#5836 = LINE ( 'NONE', #33076, #4809 ) ;
#5837 = EDGE_CURVE ( 'NONE', #10851, #18104, #16955, .T. ) ;
#5838 = VERTEX_POINT ( 'NONE', #914 ) ;
#5839 = ORIENTED_EDGE ( 'NONE', *, *, #31094, .T. ) ;
#5840 = CYLINDRICAL_SURFACE ( 'NONE', #19166, 34.41491905851385269 ) ;
#5841 = ORIENTED_EDGE ( 'NONE', *, *, #10301, .F. ) ;
#5842 = DIRECTION ( 'NONE',  ( 0.000000000000000000, 0.000000000000000000, 1.000000000000000000 ) ) ;
#5843 = PLANE ( 'NONE',  #31327 ) ;
#5844 = EDGE_LOOP ( 'NONE', ( #13677, #15893, #34133, #9914 ) ) ;
#5845 = VERTEX_POINT ( 'NONE', #3040 ) ;
#5846 = SURFACE_STYLE_USAGE ( .BOTH. , #33270 ) ;
#5847 = AXIS2_PLACEMENT_3D ( 'NONE', #34236, #4845, #34761 ) ;
#5848 = LINE ( 'NONE', #2838, #15513 ) ;
#5849 = VERTEX_POINT ( 'NONE', #11784 ) ;
#5850 = LINE ( 'NONE', #16747, #33987 ) ;
#5851 = CARTESIAN_POINT ( 'NONE',  ( 1.749999999999999778, 0.000000000000000000, 0.000000000000000000 ) ) ;
#5852 = DIRECTION ( 'NONE',  ( 0.000000000000000000, 0.000000000000000000, -1.000000000000000000 ) ) ;
#5854 = LINE ( 'NONE', #369, #24771 ) ;
#5853 = AXIS2_PLACEMENT_3D ( 'NONE', #16189, #18856, #29697 ) ;
#5855 = CIRCLE ( 'NONE', #17811, 2.524999999999999467 ) ;
#5856 = EDGE_CURVE ( 'NONE', #11163, #10000, #13912, .T. ) ;
#5857 = ADVANCED_FACE ( 'NONE', ( #560 ), #8733, .T. ) ;
#5858 = CIRCLE ( 'NONE', #18392, 4.000000000000003553 ) ;
#5859 = DIRECTION ( 'NONE',  ( 0.000000000000000000, 0.000000000000000000, 1.000000000000000000 ) ) ;
#5860 = FACE_OUTER_BOUND ( 'NONE', #34716, .T. ) ;
#5861 = LINE ( 'NONE', #22255, #29679 ) ;
#5862 = EDGE_LOOP ( 'NONE', ( #22382, #29696, #13327, #14311 ) ) ;
#5863 = DIRECTION ( 'NONE',  ( 2.631201909438060269E-14, -5.396010391056495992E-16, 0.9999999999999998890 ) ) ;
#5864 = VERTEX_POINT ( 'NONE', #9094 ) ;
#5865 = ORIENTED_EDGE ( 'NONE', *, *, #33499, .T. ) ;
#5866 = CARTESIAN_POINT ( 'NONE',  ( 1.040000000000000702, -10.89151784028311809, 32.64600270996213283 ) ) ;
#5867 = CARTESIAN_POINT ( 'NONE',  ( 10.96230482721425403, -16.64466345897533017, -77.50000000000000000 ) ) ;
#5868 = PRODUCT_CONTEXT ( 'NONE', #547, 'mechanical' ) ;
#5869 = VERTEX_POINT ( 'NONE', #3747 ) ;
#5870 = CARTESIAN_POINT ( 'NONE',  ( -442.0000000000000000, 105.0000000000000000, -77.99999999999997158 ) ) ;
#5871 = CARTESIAN_POINT ( 'NONE',  ( 15.99999999999998579, -55.00000000000000711, 154.9999999999999716 ) ) ;
#5872 = EDGE_CURVE ( 'NONE', #11863, #13812, #32632, .T. ) ;
#5873 = EDGE_CURVE ( 'NONE', #7256, #8689, #32937, .T. ) ;
#5874 = AXIS2_PLACEMENT_3D ( 'NONE', #18811, #24127, #10087 ) ;
#5875 = EDGE_CURVE ( 'NONE', #16444, #14255, #19957, .T. ) ;
#5877 = CARTESIAN_POINT ( 'NONE',  ( 2.033589656796778833, -18.61839266759088929, -28.34818773854082963 ) ) ;
#5876 = LINE ( 'NONE', #16777, #1946 ) ;
#5878 = CIRCLE ( 'NONE', #26900, 2.525000000000000799 ) ;
#5879 = ORIENTED_EDGE ( 'NONE', *, *, #11927, .F. ) ;
#5880 = VERTEX_POINT ( 'NONE', #30638 ) ;
#5881 = CIRCLE ( 'NONE', #13856, 3.999999999999976019 ) ;
#5882 = DIRECTION ( 'NONE',  ( 0.000000000000000000, -1.000000000000000000, 6.123233995736766036E-17 ) ) ;
#5883 = EDGE_CURVE ( 'NONE', #16221, #25357, #27780, .T. ) ;
#5884 = DIRECTION ( 'NONE',  ( -1.000000000000000000, -0.000000000000000000, -0.000000000000000000 ) ) ;
#5885 = LINE ( 'NONE', #3224, #9152 ) ;
#5886 = DIRECTION ( 'NONE',  ( 0.000000000000000000, -1.000000000000000000, -1.836970198721029934E-16 ) ) ;
#5887 = ORIENTED_EDGE ( 'NONE', *, *, #31119, .T. ) ;
#5888 = DIRECTION ( 'NONE',  ( 1.000000000000000000, 0.000000000000000000, -1.848892746611746966E-32 ) ) ;
#5889 = DIRECTION ( 'NONE',  ( -1.000000000000000000, -0.000000000000000000, -0.000000000000000000 ) ) ;
#5890 = LINE ( 'NONE', #12141, #20303 ) ;
#5891 = EDGE_CURVE ( 'NONE', #9401, #24518, #14093, .T. ) ;
#5892 = EDGE_LOOP ( 'NONE', ( #10072, #8196, #17320, #30908 ) ) ;
#5893 = CARTESIAN_POINT ( 'NONE',  ( 29.83064097883987742, 23.32756518004833168, 49.43553178847298568 ) ) ;
#5894 =( NAMED_UNIT ( * ) SI_UNIT ( $, .STERADIAN. ) SOLID_ANGLE_UNIT ( ) );
#5895 = DIRECTION ( 'NONE',  ( 0.000000000000000000, 0.000000000000000000, 1.000000000000000000 ) ) ;
#5897 = DIRECTION ( 'NONE',  ( -0.000000000000000000, -1.000000000000000000, -0.000000000000000000 ) ) ;
#5896 = CARTESIAN_POINT ( 'NONE',  ( 9.199999999999999289, 0.000000000000000000, 0.000000000000000000 ) ) ;
#5898 = VECTOR ( 'NONE', #23066, 1000.000000000000000 ) ;
#5899 = EDGE_CURVE ( 'NONE', #33010, #5389, #3728, .T. ) ;
#5900 = LINE ( 'NONE', #29771, #32614 ) ;
#5901 = ORIENTED_EDGE ( 'NONE', *, *, #1334, .T. ) ;
#5902 = FACE_OUTER_BOUND ( 'NONE', #33652, .T. ) ;
#5903 = FILL_AREA_STYLE ('',( #17153 ) ) ;
#5904 = DIRECTION ( 'NONE',  ( -0.000000000000000000, 1.836970198721029934E-16, -1.000000000000000000 ) ) ;
#5906 = ORIENTED_EDGE ( 'NONE', *, *, #32593, .T. ) ;
#5905 = CIRCLE ( 'NONE', #29220, 1.155000000000000027 ) ;
#5907 = AXIS2_PLACEMENT_3D ( 'NONE', #27188, #23822, #29870 ) ;
#5908 = AXIS2_PLACEMENT_3D ( 'NONE', #5559, #10582, #21430 ) ;
#5909 = ORIENTED_EDGE ( 'NONE', *, *, #25026, .T. ) ;
#5910 = ORIENTED_EDGE ( 'NONE', *, *, #13345, .T. ) ;
#5911 = DIRECTION ( 'NONE',  ( 0.000000000000000000, -1.836970198721029688E-16, 1.000000000000000000 ) ) ;
#5912 = EDGE_LOOP ( 'NONE', ( #4819, #28442, #12506, #24370 ) ) ;
#5913 = EDGE_LOOP ( 'NONE', ( #10686, #15179, #10113, #25814 ) ) ;
#5914 = DIRECTION ( 'NONE',  ( 0.000000000000000000, 1.836970198721029441E-16, -1.000000000000000000 ) ) ;
#5915 = EDGE_CURVE ( 'NONE', #31908, #9042, #5876, .T. ) ;
#5916 = EDGE_CURVE ( 'NONE', #19893, #22114, #19617, .T. ) ;
#5917 = AXIS2_PLACEMENT_3D ( 'NONE', #773, #33337, #5734 ) ;
#5918 = VERTEX_POINT ( 'NONE', #34347 ) ;
#5919 = B_SPLINE_CURVE_WITH_KNOTS ( 'NONE', 3,
 ( #30819, #29151, #14463, #33657, #925, #20795 ),
 .UNSPECIFIED., .F., .F.,
 ( 4, 2, 4 ),
 ( 4.404817078296468374E-07, 0.001874269662699937699, 0.003748098843692045969 ),
 .UNSPECIFIED. ) ;
#5920 = FACE_OUTER_BOUND ( 'NONE', #13160, .T. ) ;
#5921 = DIRECTION ( 'NONE',  ( -1.000000000000000000, -0.000000000000000000, -0.000000000000000000 ) ) ;
#5922 = EDGE_LOOP ( 'NONE', ( #34253, #30940, #9654, #19471 ) ) ;
#5923 = EDGE_LOOP ( 'NONE', ( #25751, #25025, #5313, #18495, #10692, #5356, #6545, #9302 ) ) ;
#5924 = DIRECTION ( 'NONE',  ( -0.000000000000000000, -0.000000000000000000, -1.000000000000000000 ) ) ;
#5925 = FACE_OUTER_BOUND ( 'NONE', #26464, .T. ) ;
#5926 = CIRCLE ( 'NONE', #30951, 4.000000000000003553 ) ;
#5927 = CARTESIAN_POINT ( 'NONE',  ( 101.4955157918503375, -4.558675695222540902, -11.64123453730966951 ) ) ;
#5928 = CYLINDRICAL_SURFACE ( 'NONE', #33033, 4.000000000000003553 ) ;
#5929 = ORIENTED_EDGE ( 'NONE', *, *, #10301, .T. ) ;
#5930 = EDGE_LOOP ( 'NONE', ( #3414, #28127, #14004, #28219 ) ) ;
#5931 = DIRECTION ( 'NONE',  ( -0.000000000000000000, -0.000000000000000000, -1.000000000000000000 ) ) ;
#5932 = VECTOR ( 'NONE', #26570, 1000.000000000000114 ) ;
#5933 = VECTOR ( 'NONE', #23858, 1000.000000000000000 ) ;
#5934 = DIRECTION ( 'NONE',  ( 1.000000000000000000, 0.000000000000000000, 0.000000000000000000 ) ) ;
#5935 = ORIENTED_EDGE ( 'NONE', *, *, #32961, .T. ) ;
#5936 = CIRCLE ( 'NONE', #8234, 7.999999999999979572 ) ;
#5937 = DIRECTION ( 'NONE',  ( 0.000000000000000000, 0.000000000000000000, -1.000000000000000000 ) ) ;
#5938 = PLANE ( 'NONE',  #4101 ) ;
#5939 = DIRECTION ( 'NONE',  ( -0.000000000000000000, -0.000000000000000000, -1.000000000000000000 ) ) ;
#5940 = CARTESIAN_POINT ( 'NONE',  ( 0.000000000000000000, 2.296212748401288367E-15, 47.49999999999999289 ) ) ;
#5941 = ORIENTED_EDGE ( 'NONE', *, *, #10429, .F. ) ;
#5942 = CARTESIAN_POINT ( 'NONE',  ( 11.99999999999999645, 144.9999999999999716, 159.0000000000000000 ) ) ;
#5943 = ORIENTED_EDGE ( 'NONE', *, *, #18146, .T. ) ;
#5944 = DIRECTION ( 'NONE',  ( -0.000000000000000000, -0.000000000000000000, -1.000000000000000000 ) ) ;
#5945 = AXIS2_PLACEMENT_3D ( 'NONE', #13214, #4638, #1813 ) ;
#5946 = EDGE_LOOP ( 'NONE', ( #18306, #20248, #778, #16943 ) ) ;
#5947 = DIRECTION ( 'NONE',  ( 1.000000000000000000, 0.000000000000000000, 5.546364386991661285E-52 ) ) ;
#5948 = CARTESIAN_POINT ( 'NONE',  ( 2.783107553646922305, -30.82736387488650820, -1.618073722873514697 ) ) ;
#5949 = AXIS2_PLACEMENT_3D ( 'NONE', #350, #22407, #524 ) ;
#5950 = VERTEX_POINT ( 'NONE', #28829 ) ;
#5951 = EDGE_LOOP ( 'NONE', ( #30208, #21601, #14843, #18773, #29079, #1297 ) ) ;
#5952 = AXIS2_PLACEMENT_3D ( 'NONE', #18193, #26704, #7833 ) ;
#5953 = VECTOR ( 'NONE', #24547, 1000.000000000000000 ) ;
#5954 = ORIENTED_EDGE ( 'NONE', *, *, #29830, .T. ) ;
#5955 = FACE_OUTER_BOUND ( 'NONE', #5073, .T. ) ;
#5956 = DIRECTION ( 'NONE',  ( -1.000000000000000000, 0.000000000000000000, 0.000000000000000000 ) ) ;
#5957 = EDGE_LOOP ( 'NONE', ( #19222, #25936, #16658, #23581 ) ) ;
#5958 = ORIENTED_EDGE ( 'NONE', *, *, #17584, .F. ) ;
#5959 = CARTESIAN_POINT ( 'NONE',  ( 0.000000000000000000, 6.992329373473909019E-15, 49.43553178847298568 ) ) ;
#5960 = AXIS2_PLACEMENT_3D ( 'NONE', #11666, #27842, #11482 ) ;
#5961 = EDGE_CURVE ( 'NONE', #4608, #12639, #9905, .T. ) ;
#5962 = CARTESIAN_POINT ( 'NONE',  ( -7.218132304338721994, -1.866624223957557893, 5.429999999999999716 ) ) ;
#5963 = EDGE_CURVE ( 'NONE', #9255, #33691, #12307, .T. ) ;
#5964 = LINE ( 'NONE', #643, #15777 ) ;
#5965 = PLANE ( 'NONE',  #8015 ) ;
#5966 = ORIENTED_EDGE ( 'NONE', *, *, #31444, .T. ) ;
#5967 = ORIENTED_EDGE ( 'NONE', *, *, #14279, .T. ) ;
#5968 = DIRECTION ( 'NONE',  ( 1.000000000000000000, 0.000000000000000000, 0.000000000000000000 ) ) ;
#5969 = DIRECTION ( 'NONE',  ( -0.000000000000000000, 1.836970198721029934E-16, -1.000000000000000000 ) ) ;
#5970 = CARTESIAN_POINT ( 'NONE',  ( 0.000000000000000000, 0.000000000000000000, 0.000000000000000000 ) ) ;
#5971 = DIRECTION ( 'NONE',  ( 0.000000000000000000, -0.000000000000000000, 1.000000000000000000 ) ) ;
#5972 = DIRECTION ( 'NONE',  ( -1.000000000000000000, 0.000000000000000000, 0.000000000000000000 ) ) ;
#5973 = VECTOR ( 'NONE', #23319, 1000.000000000000000 ) ;
#5974 = CARTESIAN_POINT ( 'NONE',  ( -355.0000000000000000, -114.9999999999999858, 113.9999999999999858 ) ) ;
#5975 = DIRECTION ( 'NONE',  ( 1.000000000000000000, 0.000000000000000000, 0.000000000000000000 ) ) ;
#5976 = LINE ( 'NONE', #16876, #14165 ) ;
#5977 = ORIENTED_EDGE ( 'NONE', *, *, #13076, .T. ) ;
#5978 = AXIS2_PLACEMENT_3D ( 'NONE', #6644, #974, #17542 ) ;
#5979 = AXIS2_PLACEMENT_3D ( 'NONE', #28586, #1534, #22898 ) ;
#5980 = FACE_OUTER_BOUND ( 'NONE', #13419, .T. ) ;
#5981 = CARTESIAN_POINT ( 'NONE',  ( -5.021133111224679091, 26.05646109878476224, -67.50000000000000000 ) ) ;
#5982 = CARTESIAN_POINT ( 'NONE',  ( -349.0000000000000000, -125.0000000000000284, 166.9999999999999716 ) ) ;
#5983 = VERTEX_POINT ( 'NONE', #12650 ) ;
#5984 = B_SPLINE_CURVE_WITH_KNOTS ( 'NONE', 3,
 ( #1792, #6949, #17843, #3766 ),
 .UNSPECIFIED., .F., .F.,
 ( 4, 4 ),
 ( 0.005298349496164106269, 0.005985218188604198714 ),
 .UNSPECIFIED. ) ;
#5985 = APPLICATION_CONTEXT ( 'automotive_design' ) ;
#5986 = DIRECTION ( 'NONE',  ( -1.000000000000000000, 0.000000000000000000, 0.000000000000000000 ) ) ;
#5987 = ORIENTED_EDGE ( 'NONE', *, *, #231, .T. ) ;
#5988 = DIRECTION ( 'NONE',  ( 0.000000000000000000, -1.000000000000000000, -2.465190328815662439E-32 ) ) ;
#5990 = VECTOR ( 'NONE', #8937, 1000.000000000000000 ) ;
#5989 = CARTESIAN_POINT ( 'NONE',  ( -19.99999999999998934, -137.0000000000000000, 162.9999999999999716 ) ) ;
#5991 = VERTEX_POINT ( 'NONE', #4594 ) ;
#5992 = CARTESIAN_POINT ( 'NONE',  ( 1.395000000000002238, -1.891117961020238436, 34.36292081097831641 ) ) ;
#5993 = CARTESIAN_POINT ( 'NONE',  ( -12.00000000000001066, 136.9999999999999716, -175.0000000000000284 ) ) ;
#5994 = CARTESIAN_POINT ( 'NONE',  ( -418.0000000000000000, 105.0000000000000000, 135.9999999999999716 ) ) ;
#5995 = ORIENTED_EDGE ( 'NONE', *, *, #7093, .F. ) ;
#5996 = AXIS2_PLACEMENT_3D ( 'NONE', #14680, #1135, #12000 ) ;
#5997 = CARTESIAN_POINT ( 'NONE',  ( 833.9789710600518902, 1190.245311366547639, 1753.598338701303419 ) ) ;
#5998 = CARTESIAN_POINT ( 'NONE',  ( 19.99999999999996092, -145.0000000000000000, -186.9999999999999716 ) ) ;
#5999 = VERTEX_POINT ( 'NONE', #23488 ) ;
#6000 = VECTOR ( 'NONE', #441, 1000.000000000000000 ) ;
#6001 = CARTESIAN_POINT ( 'NONE',  ( 0.1859802741905670354, -24.34160354263086035, 21.20368514569409513 ) ) ;
#6002 = EDGE_CURVE ( 'NONE', #26019, #34152, #1950, .T. ) ;
#6003 = DIRECTION ( 'NONE',  ( 0.000000000000000000, 0.000000000000000000, -1.000000000000000000 ) ) ;
#6004 = FACE_OUTER_BOUND ( 'NONE', #3286, .T. ) ;
#6005 = CARTESIAN_POINT ( 'NONE',  ( -108.1236054928398573, -4.063426306576022995, 6.307665442424295499 ) ) ;
#6006 = ORIENTED_EDGE ( 'NONE', *, *, #16687, .T. ) ;
#6007 = EDGE_LOOP ( 'NONE', ( #2586, #1566 ) ) ;
#6008 = VERTEX_POINT ( 'NONE', #33830 ) ;
#6009 = EDGE_CURVE ( 'NONE', #10891, #18561, #14477, .T. ) ;
#6010 = DIRECTION ( 'NONE',  ( 3.697785493223492838E-32, 1.934419779023891545E-16, -1.000000000000000000 ) ) ;
#6011 = CIRCLE ( 'NONE', #35032, 1.799999999999999600 ) ;
#6012 = EDGE_CURVE ( 'NONE', #3630, #2071, #31163, .T. ) ;
#6013 = DIRECTION ( 'NONE',  ( 0.000000000000000000, 1.000000000000000000, 5.053935297177146739E-49 ) ) ;
#6014 = CARTESIAN_POINT ( 'NONE',  ( -15.99999999999998579, -112.9999999999999858, -155.0000000000000284 ) ) ;
#6015 = ORIENTED_EDGE ( 'NONE', *, *, #13544, .T. ) ;
#6016 = VERTEX_POINT ( 'NONE', #9791 ) ;
#6017 = EDGE_CURVE ( 'NONE', #31113, #24248, #30357, .T. ) ;
#6018 = EDGE_CURVE ( 'NONE', #34124, #32595, #4263, .T. ) ;
#6019 = CARTESIAN_POINT ( 'NONE',  ( -365.0000000000000000, -125.0000000000000284, 130.0000000000000000 ) ) ;
#6020 = ORIENTED_EDGE ( 'NONE', *, *, #9348, .T. ) ;
#6021 = DIRECTION ( 'NONE',  ( 0.000000000000000000, 0.000000000000000000, 1.000000000000000000 ) ) ;
#6022 = EDGE_CURVE ( 'NONE', #25655, #5400, #12830, .T. ) ;
#6023 = DIRECTION ( 'NONE',  ( 0.000000000000000000, 0.000000000000000000, 1.000000000000000000 ) ) ;
#6024 = ORIENTED_EDGE ( 'NONE', *, *, #30619, .T. ) ;
#6025 = ORIENTED_EDGE ( 'NONE', *, *, #8679, .F. ) ;
#6026 = AXIS2_PLACEMENT_3D ( 'NONE', #28667, #20143, #14805 ) ;
#6027 = CARTESIAN_POINT ( 'NONE',  ( 0.000000000000000000, 0.000000000000000000, 0.000000000000000000 ) ) ;
#6028 = CYLINDRICAL_SURFACE ( 'NONE', #2409, 7.999999999999979572 ) ;
#6029 = ORIENTED_EDGE ( 'NONE', *, *, #31658, .T. ) ;
#6030 = VECTOR ( 'NONE', #8217, 1000.000000000000000 ) ;
#6031 = CARTESIAN_POINT ( 'NONE',  ( -442.0000000000000000, -125.0000000000000000, 187.0000000000000000 ) ) ;
#6032 = SURFACE_SIDE_STYLE ('',( #33451 ) ) ;
#6033 = DIRECTION ( 'NONE',  ( 0.000000000000000000, 0.000000000000000000, 1.000000000000000000 ) ) ;
#6034 = FILL_AREA_STYLE_COLOUR ( '', #7718 ) ;
#6035 = CARTESIAN_POINT ( 'NONE',  ( -105.6811520247811558, -5.080615126163384510, 11.42114788619747046 ) ) ;
#6036 = CARTESIAN_POINT ( 'NONE',  ( 2.765921099433442443, 29.44518845714779332, -9.980709654879110104 ) ) ;
#6037 = CARTESIAN_POINT ( 'NONE',  ( 19.99999999999998934, 112.9999999999999574, -175.0000000000000284 ) ) ;
#6038 = VECTOR ( 'NONE', #29775, 1000.000000000000000 ) ;
#6039 = ORIENTED_EDGE ( 'NONE', *, *, #3918, .F. ) ;
#6040 = VERTEX_POINT ( 'NONE', #15323 ) ;
#6041 = CARTESIAN_POINT ( 'NONE',  ( 847.1182614860877038, 1067.446319375197845, 1753.598338701303192 ) ) ;
#6042 = ORIENTED_EDGE ( 'NONE', *, *, #1262, .F. ) ;
#6043 = EDGE_LOOP ( 'NONE', ( #23638, #30071, #13864, #31060 ) ) ;
#6044 = DIRECTION ( 'NONE',  ( 0.000000000000000000, 0.000000000000000000, -1.000000000000000000 ) ) ;
#6045 = AXIS2_PLACEMENT_3D ( 'NONE', #20829, #26336, #18181 ) ;
#6046 = DIRECTION ( 'NONE',  ( 0.000000000000000000, 1.000000000000000000, 1.224646799147353207E-16 ) ) ;
#6047 = SHAPE_DEFINITION_REPRESENTATION ( #6066, #19821 ) ;
#6048 = ORIENTED_EDGE ( 'NONE', *, *, #27311, .F. ) ;
#6049 = DIRECTION ( 'NONE',  ( 0.000000000000000000, 1.000000000000000000, 1.131431318426415506E-52 ) ) ;
#6050 = CARTESIAN_POINT ( 'NONE',  ( -109.9479883445679178, -1.339152422118500718, -12.43243648734289408 ) ) ;
#6051 = EDGE_CURVE ( 'NONE', #29779, #16703, #34345, .T. ) ;
#6053 = DIRECTION ( 'NONE',  ( -0.000000000000000000, -0.000000000000000000, -1.000000000000000000 ) ) ;
#6052 = CARTESIAN_POINT ( 'NONE',  ( 0.2989565185775198697, 0.000000000000000000, 0.000000000000000000 ) ) ;
#6054 = ORIENTED_EDGE ( 'NONE', *, *, #21261, .F. ) ;
#6055 = ORIENTED_EDGE ( 'NONE', *, *, #25131, .F. ) ;
#6056 = EDGE_CURVE ( 'NONE', #5551, #11743, #6763, .T. ) ;
#6057 = EDGE_CURVE ( 'NONE', #23099, #30505, #25986, .T. ) ;
#6058 = CARTESIAN_POINT ( 'NONE',  ( -5.527271473480783293, -1.747512292859696226, 3.930000000000000160 ) ) ;
#6059 = DIRECTION ( 'NONE',  ( 1.000000000000000000, 0.000000000000000000, 0.000000000000000000 ) ) ;
#6060 = CARTESIAN_POINT ( 'NONE',  ( -499.9999999999999432, -113.0000000000000000, -155.0000000000000000 ) ) ;
#6061 = DIRECTION ( 'NONE',  ( -1.000000000000000000, 0.000000000000000000, 0.000000000000000000 ) ) ;
#6062 = ORIENTED_EDGE ( 'NONE', *, *, #32625, .F. ) ;
#6063 = LINE ( 'NONE', #13924, #4981 ) ;
#6064 = DIRECTION ( 'NONE',  ( -2.530127506375325574E-80, 1.000000000000000000, 6.842277657836020854E-49 ) ) ;
#6065 = CARTESIAN_POINT ( 'NONE',  ( -7.433561145103738198E-15, 11.02739026146940304, 7.899999792244740249 ) ) ;
#6066 = PRODUCT_DEFINITION_SHAPE ( 'NONE', 'NONE',  #329 ) ;
#6067 = ORIENTED_EDGE ( 'NONE', *, *, #22211, .F. ) ;
#6068 = DIRECTION ( 'NONE',  ( 0.000000000000000000, 1.000000000000000000, 5.145227585319922065E-49 ) ) ;
#6069 = FACE_OUTER_BOUND ( 'NONE', #24835, .T. ) ;
#6070 = EDGE_CURVE ( 'NONE', #11447, #14721, #22973, .T. ) ;
#6071 = LINE ( 'NONE', #33849, #22931 ) ;
#6073 = CARTESIAN_POINT ( 'NONE',  ( 9.199999999999999289, 7.794228634059932048, -13.49999999999999822 ) ) ;
#6072 = DIRECTION ( 'NONE',  ( 1.000000000000000000, 0.000000000000000000, -0.000000000000000000 ) ) ;
#6074 = VECTOR ( 'NONE', #3531, 1000.000000000000000 ) ;
#6075 = AXIS2_PLACEMENT_3D ( 'NONE', #5188, #26915, #13408 ) ;
#6076 = UNCERTAINTY_MEASURE_WITH_UNIT (LENGTH_MEASURE( 1.000000000000000082E-05 ), #14562, 'distance_accuracy_value', 'NONE');
#6077 = CARTESIAN_POINT ( 'NONE',  ( 10.17231796313407344, -1.579009122040562207, -77.50000000000000000 ) ) ;
#6078 = ORIENTED_EDGE ( 'NONE', *, *, #15449, .T. ) ;
#6079 = CARTESIAN_POINT ( 'NONE',  ( -20.02113311122478123, 18.16264470403145026, -67.50000000000000000 ) ) ;
#6080 = EDGE_CURVE ( 'NONE', #14482, #29522, #13328, .T. ) ;
#6081 = EDGE_CURVE ( 'NONE', #12565, #8883, #23322, .T. ) ;
#6082 = VECTOR ( 'NONE', #29669, 1000.000000000000000 ) ;
#6083 = EDGE_CURVE ( 'NONE', #34030, #8526, #17824, .T. ) ;
#6084 = ORIENTED_EDGE ( 'NONE', *, *, #34966, .F. ) ;
#6085 = VECTOR ( 'NONE', #28786, 1000.000000000000000 ) ;
#6086 = EDGE_CURVE ( 'NONE', #4938, #1226, #6225, .T. ) ;
#6087 = ORIENTED_EDGE ( 'NONE', *, *, #6218, .T. ) ;
#6088 = AXIS2_PLACEMENT_3D ( 'NONE', #883, #9238, #705 ) ;
#6089 = EDGE_LOOP ( 'NONE', ( #5411, #29755, #24793, #32754 ) ) ;
#6090 = CARTESIAN_POINT ( 'NONE',  ( 14.70109753509668948, 34.88954974633765005, 68.31122994652405112 ) ) ;
#6091 = ORIENTED_EDGE ( 'NONE', *, *, #14811, .T. ) ;
#6092 = ORIENTED_EDGE ( 'NONE', *, *, #29545, .T. ) ;
#6093 = CARTESIAN_POINT ( 'NONE',  ( 36.86854689046325717, 8.645963718612074800, 68.31122994652405112 ) ) ;
#6094 = CONTEXT_DEPENDENT_SHAPE_REPRESENTATION ( #31912, #34492 ) ;
#6095 = VECTOR ( 'NONE', #4482, 1000.000000000000000 ) ;
#6096 = VECTOR ( 'NONE', #5370, 999.9999999999998863 ) ;
#6097 = ORIENTED_EDGE ( 'NONE', *, *, #15313, .T. ) ;
#6098 = CYLINDRICAL_SURFACE ( 'NONE', #18648, 2.524999999999999467 ) ;
#6099 = DIRECTION ( 'NONE',  ( 1.000000000000000000, 3.469446951953834515E-18, 0.000000000000000000 ) ) ;
#6100 = EDGE_LOOP ( 'NONE', ( #23228, #31203, #1076, #30690, #12698, #18855, #27814, #9487 ) ) ;
#6101 = ORIENTED_EDGE ( 'NONE', *, *, #34373, .T. ) ;
#6102 = EDGE_CURVE ( 'NONE', #14780, #24095, #31325, .T. ) ;
#6103 = CARTESIAN_POINT ( 'NONE',  ( -19.99999999999998934, 75.55999999999990280, 177.7400000000000091 ) ) ;
#6104 = DIRECTION ( 'NONE',  ( 0.000000000000000000, 1.836970198721029688E-16, -1.000000000000000000 ) ) ;
#6105 = CARTESIAN_POINT ( 'NONE',  ( 107.8902921054316124, -4.970825052104117070, -11.47130252761374081 ) ) ;
#6106 = CARTESIAN_POINT ( 'NONE',  ( 11.99999999999999645, 134.9999999999998863, 187.0000000000000000 ) ) ;
#6107 = LINE ( 'NONE', #966, #26174 ) ;
#6108 = VERTEX_POINT ( 'NONE', #20653 ) ;
#6109 = AXIS2_PLACEMENT_3D ( 'NONE', #26033, #10013, #23026 ) ;
#6110 = DIRECTION ( 'NONE',  ( 1.000000000000000000, 0.000000000000000000, 0.000000000000000000 ) ) ;
#6111 = CARTESIAN_POINT ( 'NONE',  ( 21.85761591200894216, 30.91355005303805825, 68.31122994652405112 ) ) ;
#6112 = ORIENTED_EDGE ( 'NONE', *, *, #11608, .F. ) ;
#6113 = LINE ( 'NONE', #17013, #26515 ) ;
#6114 = DIRECTION ( 'NONE',  ( -0.000000000000000000, 1.000000000000000000, 0.000000000000000000 ) ) ;
#6115 = CARTESIAN_POINT ( 'NONE',  ( 22.89764159710615132, -5.651112684911597128, -77.50000000000000000 ) ) ;
#6116 = CARTESIAN_POINT ( 'NONE',  ( 99.26191511054632599, -4.118294838564020743E-16, -7.500000000000000000 ) ) ;
#6117 = PRESENTATION_STYLE_ASSIGNMENT (( #22868 ) ) ;
#6118 = CIRCLE ( 'NONE', #19790, 1.155000000000000027 ) ;
#6119 = DIRECTION ( 'NONE',  ( 0.000000000000000000, 0.000000000000000000, 1.000000000000000000 ) ) ;
#6120 = ORIENTED_EDGE ( 'NONE', *, *, #1495, .T. ) ;
#6121 = LINE ( 'NONE', #5287, #19000 ) ;
#6123 = CARTESIAN_POINT ( 'NONE',  ( -27.76765758629847980, -16.97532223688792996, 68.31122994652405112 ) ) ;
#6122 = DIRECTION ( 'NONE',  ( -1.000000000000000000, -0.000000000000000000, -0.000000000000000000 ) ) ;
#6124 = EDGE_CURVE ( 'NONE', #29370, #13424, #10681, .T. ) ;
#6125 = AXIS2_PLACEMENT_3D ( 'NONE', #5614, #11512, #16512 ) ;
#6126 = EDGE_CURVE ( 'NONE', #35, #34661, #21532, .T. ) ;
#6127 = ORIENTED_EDGE ( 'NONE', *, *, #27207, .T. ) ;
#6128 = LINE ( 'NONE', #11317, #21171 ) ;
#6129 = LINE ( 'NONE', #28034, #19992 ) ;
#6130 = EDGE_LOOP ( 'NONE', ( #487, #2381, #33524, #1051, #34952, #25371 ) ) ;
#6131 = VECTOR ( 'NONE', #33165, 1000.000000000000000 ) ;
#6132 = ADVANCED_FACE ( 'NONE', ( #15680 ), #2825, .F. ) ;
#6133 = ORIENTED_EDGE ( 'NONE', *, *, #12186, .T. ) ;
#6134 = CARTESIAN_POINT ( 'NONE',  ( -20.02113311122478123, 18.16264470403145026, -67.50000000000000000 ) ) ;
#6135 = ORIENTED_EDGE ( 'NONE', *, *, #30246, .F. ) ;
#6136 = ORIENTED_EDGE ( 'NONE', *, *, #635, .T. ) ;
#6137 = DIRECTION ( 'NONE',  ( -0.000000000000000000, 1.836970198721029934E-16, -1.000000000000000000 ) ) ;
#6138 = PLANE ( 'NONE',  #28383 ) ;
#6139 = AXIS2_PLACEMENT_3D ( 'NONE', #28319, #3914, #11602 ) ;
#6140 = DIRECTION ( 'NONE',  ( 0.000000000000000000, 0.000000000000000000, 1.000000000000000000 ) ) ;
#6141 = CARTESIAN_POINT ( 'NONE',  ( 0.002098586324980263994, 27.86175707474580321, -12.86217335695010533 ) ) ;
#6142 = ORIENTED_EDGE ( 'NONE', *, *, #6018, .T. ) ;
#6143 = ORIENTED_EDGE ( 'NONE', *, *, #30049, .F. ) ;
#6144 = PLANE ( 'NONE',  #34423 ) ;
#6145 = CYLINDRICAL_SURFACE ( 'NONE', #28870, 1.154999999999999805 ) ;
#6146 = DIRECTION ( 'NONE',  ( -1.000000000000000000, -0.000000000000000000, -0.000000000000000000 ) ) ;
#6147 = CARTESIAN_POINT ( 'NONE',  ( 0.7181323043387221050, -1.866624223957557893, -0.7500000000000000000 ) ) ;
#6148 = DIRECTION ( 'NONE',  ( 0.000000000000000000, 0.000000000000000000, -1.000000000000000000 ) ) ;
#6149 = AXIS2_PLACEMENT_3D ( 'NONE', #32681, #8302, #16685 ) ;
#6150 = DIRECTION ( 'NONE',  ( 0.000000000000000000, 1.836970198721029441E-16, -1.000000000000000000 ) ) ;
#6152 = VECTOR ( 'NONE', #16384, 1000.000000000000000 ) ;
#6151 = DIRECTION ( 'NONE',  ( 0.000000000000000000, -7.888609052210118054E-31, -1.000000000000000000 ) ) ;
#6153 = ORIENTED_EDGE ( 'NONE', *, *, #19154, .T. ) ;
#6154 = EDGE_CURVE ( 'NONE', #19647, #2206, #24091, .T. ) ;
#6155 = DIRECTION ( 'NONE',  ( -0.000000000000000000, -0.000000000000000000, 1.000000000000000000 ) ) ;
#6156 = LINE ( 'NONE', #28590, #30800 ) ;
#6157 = VECTOR ( 'NONE', #20359, 1000.000000000000000 ) ;
#6158 = CARTESIAN_POINT ( 'NONE',  ( 2.789999999999999147, -11.07880054387200985, -29.04985141099774637 ) ) ;
#6159 = ORIENTED_EDGE ( 'NONE', *, *, #26308, .F. ) ;
#6160 = DIRECTION ( 'NONE',  ( 1.000000000000000000, 3.469446951953834515E-18, 0.000000000000000000 ) ) ;
#6161 = VERTEX_POINT ( 'NONE', #34700 ) ;
#6162 = LINE ( 'NONE', #17062, #30417 ) ;
#6163 = LINE ( 'NONE', #17063, #11476 ) ;
#6164 = ADVANCED_FACE ( 'NONE', ( #29712 ), #13692, .T. ) ;
#6165 = EDGE_CURVE ( 'NONE', #28037, #17552, #2502, .T. ) ;
#6166 = EDGE_CURVE ( 'NONE', #30767, #27908, #24708, .T. ) ;
#6167 = CIRCLE ( 'NONE', #26071, 15.00000000000000000 ) ;
#6168 = EDGE_LOOP ( 'NONE', ( #10986, #30418, #14003, #26658 ) ) ;
#6169 = PLANE ( 'NONE',  #22266 ) ;
#6170 = DIRECTION ( 'NONE',  ( 1.000000000000000000, 3.040835319149746090E-31, 1.232595164407830946E-32 ) ) ;
#6171 = CARTESIAN_POINT ( 'NONE',  ( 145.0000000000000568, 87.50000000000000000, 65.00000000000000000 ) ) ;
#6172 = ORIENTED_EDGE ( 'NONE', *, *, #18618, .T. ) ;
#6173 = DIRECTION ( 'NONE',  ( 2.631201909438060585E-14, -5.396010391056496978E-16, 1.000000000000000000 ) ) ;
#6174 = FACE_OUTER_BOUND ( 'NONE', #12972, .T. ) ;
#6175 = ORIENTED_EDGE ( 'NONE', *, *, #8693, .T. ) ;
#6176 = CARTESIAN_POINT ( 'NONE',  ( 187.4264068711928530, -12.50000000000001066, 1.224646799147353217E-14 ) ) ;
#6177 = VECTOR ( 'NONE', #11170, 1000.000000000000000 ) ;
#6178 = PRESENTATION_STYLE_ASSIGNMENT (( #17074 ) ) ;
#6179 = B_SPLINE_CURVE_WITH_KNOTS ( 'NONE', 3,
 ( #18835, #32866, #27530, #24853 ),
 .UNSPECIFIED., .F., .F.,
 ( 4, 4 ),
 ( 4.608367445541797598E-07, 0.0006881987313283725351 ),
 .UNSPECIFIED. ) ;
#6180 = DIRECTION ( 'NONE',  ( 0.3193015301359797276, -0.9476531711828024562, 0.000000000000000000 ) ) ;
#6181 = CARTESIAN_POINT ( 'NONE',  ( 12.73347502555019162, -33.69708579775584667, 49.43553178847298568 ) ) ;
#6182 = CONTEXT_DEPENDENT_SHAPE_REPRESENTATION ( #12413, #23694 ) ;
#6183 = ORIENTED_EDGE ( 'NONE', *, *, #382, .F. ) ;
#6184 = ORIENTED_EDGE ( 'NONE', *, *, #9000, .F. ) ;
#6185 = ORIENTED_EDGE ( 'NONE', *, *, #19899, .T. ) ;
#6186 = LINE ( 'NONE', #17617, #8041 ) ;
#6187 = DIRECTION ( 'NONE',  ( 0.000000000000000000, 0.000000000000000000, -1.000000000000000000 ) ) ;
#6188 = VECTOR ( 'NONE', #27293, 1000.000000000000000 ) ;
#6189 = CARTESIAN_POINT ( 'NONE',  ( -5.210000000000000853, 0.000000000000000000, 0.000000000000000000 ) ) ;
#6190 = ORIENTED_EDGE ( 'NONE', *, *, #7737, .T. ) ;
#6191 = ORIENTED_EDGE ( 'NONE', *, *, #24749, .F. ) ;
#6192 = DIRECTION ( 'NONE',  ( -1.000000000000000000, -0.000000000000000000, -0.000000000000000000 ) ) ;
#6193 = ORIENTED_EDGE ( 'NONE', *, *, #5711, .F. ) ;
#6194 = DIRECTION ( 'NONE',  ( -3.469446951953832974E-18, -1.000000000000000000, -7.888609052210116302E-31 ) ) ;
#6195 = CARTESIAN_POINT ( 'NONE',  ( -6.500000000000000000, 0.000000000000000000, 3.180000000000000160 ) ) ;
#6196 = EDGE_LOOP ( 'NONE', ( #9973, #31628, #6229, #28424 ) ) ;
#6197 = CIRCLE ( 'NONE', #16449, 2.000000000000001776 ) ;
#6198 = ORIENTED_EDGE ( 'NONE', *, *, #657, .F. ) ;
#6199 = DIRECTION ( 'NONE',  ( -0.000000000000000000, -1.836970198721029688E-16, 1.000000000000000000 ) ) ;
#6200 = EDGE_CURVE ( 'NONE', #14410, #34772, #4780, .T. ) ;
#6201 = DIRECTION ( 'NONE',  ( 0.000000000000000000, 1.000000000000000000, -1.224646799147353207E-16 ) ) ;
#6202 = VERTEX_POINT ( 'NONE', #32369 ) ;
#6203 = LINE ( 'NONE', #891, #14674 ) ;
#6204 = EDGE_CURVE ( 'NONE', #5237, #20827, #2655, .T. ) ;
#6205 = CARTESIAN_POINT ( 'NONE',  ( 27.99209646187092559, 25.49206711720156093, 68.31122994652405112 ) ) ;
#6206 = AXIS2_PLACEMENT_3D ( 'NONE', #23593, #26430, #12569 ) ;
#6207 = CARTESIAN_POINT ( 'NONE',  ( -365.0000000000000000, -119.0000000000000000, 110.0000000000000000 ) ) ;
#6208 = EDGE_CURVE ( 'NONE', #34376, #8985, #13523, .T. ) ;
#6209 = FACE_OUTER_BOUND ( 'NONE', #17421, .T. ) ;
#6210 = DIRECTION ( 'NONE',  ( 0.000000000000000000, 0.000000000000000000, 1.000000000000000000 ) ) ;
#6212 = EDGE_CURVE ( 'NONE', #1742, #22309, #11650, .T. ) ;
#6211 =( NAMED_UNIT ( * ) PLANE_ANGLE_UNIT ( ) SI_UNIT ( $, .RADIAN. ) );
#6213 = ORIENTED_EDGE ( 'NONE', *, *, #31835, .F. ) ;
#6214 = EDGE_LOOP ( 'NONE', ( #8870, #26253, #3248, #28580 ) ) ;
#6215 = DIRECTION ( 'NONE',  ( 0.1063910735368947813, -0.9943243633099144718, -3.335902418024520312E-15 ) ) ;
#6216 = VERTEX_POINT ( 'NONE', #29367 ) ;
#6217 = ORIENTED_EDGE ( 'NONE', *, *, #22597, .T. ) ;
#6218 = EDGE_CURVE ( 'NONE', #11399, #12523, #32102, .T. ) ;
#6219 = ADVANCED_FACE ( 'NONE', ( #23840 ), #10315, .T. ) ;
#6220 = FACE_OUTER_BOUND ( 'NONE', #19856, .T. ) ;
#6221 = ORIENTED_EDGE ( 'NONE', *, *, #28520, .F. ) ;
#6222 = LINE ( 'NONE', #911, #895 ) ;
#6223 = CARTESIAN_POINT ( 'NONE',  ( 0.000000000000000000, 0.000000000000000000, -0.7500000000000000000 ) ) ;
#6224 = VECTOR ( 'NONE', #31383, 1000.000000000000000 ) ;
#6225 = B_SPLINE_CURVE_WITH_KNOTS ( 'NONE', 3,
 ( #1773, #18177, #20479, #29003, #15494, #34526 ),
 .UNSPECIFIED., .F., .F.,
 ( 4, 2, 4 ),
 ( 2.120780580243931197E-07, 0.001873410385593401008, 0.003746608693128777694 ),
 .UNSPECIFIED. ) ;
#6227 = DIRECTION ( 'NONE',  ( 0.000000000000000000, 0.000000000000000000, 1.000000000000000000 ) ) ;
#6226 = DIRECTION ( 'NONE',  ( -0.7960930657056433102, -0.6051742151937656855, -0.000000000000000000 ) ) ;
#6228 = ORIENTED_EDGE ( 'NONE', *, *, #11773, .T. ) ;
#6229 = ORIENTED_EDGE ( 'NONE', *, *, #3023, .F. ) ;
#6230 = CARTESIAN_POINT ( 'NONE',  ( 145.0000000000000568, -12.50000000000000888, -14.99999999999998757 ) ) ;
#6231 = DIRECTION ( 'NONE',  ( 0.000000000000000000, 1.836970198721029688E-16, -1.000000000000000000 ) ) ;
#6232 = LINE ( 'NONE', #921, #2327 ) ;
#6233 = FACE_OUTER_BOUND ( 'NONE', #14124, .T. ) ;
#6234 = ORIENTED_EDGE ( 'NONE', *, *, #12997, .F. ) ;
#6235 = DIRECTION ( 'NONE',  ( 0.000000000000000000, 0.000000000000000000, 1.000000000000000000 ) ) ;
#6236 = LINE ( 'NONE', #31639, #19124 ) ;
#6237 = CARTESIAN_POINT ( 'NONE',  ( 1.532562817202168803, 32.50931595846692801, 49.43553178847298568 ) ) ;
#6238 =( REPRESENTATION_RELATIONSHIP ('NONE','NONE', #23037, #28231 ) REPRESENTATION_RELATIONSHIP_WITH_TRANSFORMATION ( #21962 )SHAPE_REPRESENTATION_RELATIONSHIP( ) );
#6239 = VERTEX_POINT ( 'NONE', #5490 ) ;
#6240 = CARTESIAN_POINT ( 'NONE',  ( 1.040000000000000924, 0.000000000000000000, 0.000000000000000000 ) ) ;
#6241 = DIRECTION ( 'NONE',  ( -1.000000000000000000, 0.000000000000000000, 1.232595164407831220E-32 ) ) ;
#6242 = DIRECTION ( 'NONE',  ( 0.000000000000000000, 0.000000000000000000, -1.000000000000000000 ) ) ;
#6244 = LINE ( 'NONE', #3583, #3739 ) ;
#6243 = LINE ( 'NONE', #11803, #26397 ) ;
#6245 = LINE ( 'NONE', #14297, #22421 ) ;
#6246 = DIRECTION ( 'NONE',  ( 1.000000000000000000, 0.000000000000000000, 0.000000000000000000 ) ) ;
#6247 = ORIENTED_EDGE ( 'NONE', *, *, #14778, .F. ) ;
#6248 = DIRECTION ( 'NONE',  ( -0.000000000000000000, -1.836970198721029688E-16, 1.000000000000000000 ) ) ;
#6250 = EDGE_CURVE ( 'NONE', #13120, #15487, #5136, .T. ) ;
#6249 = CARTESIAN_POINT ( 'NONE',  ( -418.0000000000000000, -124.9999999999999858, -69.99999999999998579 ) ) ;
#6251 = ADVANCED_FACE ( 'NONE', ( #4960 ), #15857, .F. ) ;
#6252 = TOROIDAL_SURFACE ( 'NONE', #33532, 30.47050528711511674, 8.000000000000000000 ) ;
#6253 = ORIENTED_EDGE ( 'NONE', *, *, #8008, .T. ) ;
#6254 = ADVANCED_FACE ( 'NONE', ( #7987 ), #10501, .F. ) ;
#6255 = EDGE_CURVE ( 'NONE', #25547, #17261, #13354, .T. ) ;
#6256 =( NAMED_UNIT ( * ) PLANE_ANGLE_UNIT ( ) SI_UNIT ( $, .RADIAN. ) );
#6257 = VERTEX_POINT ( 'NONE', #30597 ) ;
#6258 = VECTOR ( 'NONE', #8785, 1000.000000000000000 ) ;
#6259 = VERTEX_POINT ( 'NONE', #16555 ) ;
#6260 = DIRECTION ( 'NONE',  ( 1.000000000000000000, 0.000000000000000000, 0.000000000000000000 ) ) ;
#6261 = ORIENTED_EDGE ( 'NONE', *, *, #1841, .F. ) ;
#6262 = ORIENTED_EDGE ( 'NONE', *, *, #11143, .F. ) ;
#6263 = FACE_OUTER_BOUND ( 'NONE', #26371, .T. ) ;
#6264 = EDGE_CURVE ( 'NONE', #4827, #27012, #16793, .T. ) ;
#6265 = CONTEXT_DEPENDENT_SHAPE_REPRESENTATION ( #4420, #9174 ) ;
#6266 = ORIENTED_EDGE ( 'NONE', *, *, #14682, .T. ) ;
#6267 = DIRECTION ( 'NONE',  ( 1.000000000000000000, 0.000000000000000000, 0.000000000000000000 ) ) ;
#6268 = PLANE ( 'NONE',  #6334 ) ;
#6269 = ORIENTED_EDGE ( 'NONE', *, *, #17400, .T. ) ;
#6270 = ORIENTED_EDGE ( 'NONE', *, *, #29153, .T. ) ;
#6271 = CARTESIAN_POINT ( 'NONE',  ( 2.765921099433442887, -26.45933846664205902, 16.32596387352436551 ) ) ;
#6273 = DIRECTION ( 'NONE',  ( -1.000000000000000000, 6.792721752314501023E-48, -3.697785493223492838E-32 ) ) ;
#6272 = AXIS2_PLACEMENT_3D ( 'NONE', #2388, #13971, #32981 ) ;
#6274 = CARTESIAN_POINT ( 'NONE',  ( -5.781867695661277118, -1.866624223957557893, 5.429999999999999716 ) ) ;
#6275 = DIRECTION ( 'NONE',  ( -1.000000000000000000, 0.000000000000000000, 0.000000000000000000 ) ) ;
#6276 = CARTESIAN_POINT ( 'NONE',  ( 2.630124765083918348, -1.866624223957557893, 5.429999999999999716 ) ) ;
#6277 = VERTEX_POINT ( 'NONE', #8353 ) ;
#6278 = AXIS2_PLACEMENT_3D ( 'NONE', #19178, #16152, #5443 ) ;
#6279 = EDGE_CURVE ( 'NONE', #8432, #10891, #283, .T. ) ;
#6280 = CARTESIAN_POINT ( 'NONE',  ( -14.49673343639653744, 34.98409864655521773, 68.31122994652405112 ) ) ;
#6281 = ADVANCED_FACE ( 'NONE', ( #17083 ), #27916, .T. ) ;
#6282 = DIRECTION ( 'NONE',  ( 0.000000000000000000, 0.000000000000000000, -1.000000000000000000 ) ) ;
#6283 = VERTEX_POINT ( 'NONE', #16914 ) ;
#6284 = PLANE ( 'NONE',  #2078 ) ;
#6285 = CARTESIAN_POINT ( 'NONE',  ( -35.00000000000000000, 0.000000000000000000, 0.000000000000000000 ) ) ;
#6286 = PLANE ( 'NONE',  #30301 ) ;
#6287 = DIRECTION ( 'NONE',  ( 2.891205793294675861E-16, 0.000000000000000000, -1.000000000000000000 ) ) ;
#6288 = DIRECTION ( 'NONE',  ( -0.8835120444460231592, 0.4684084406997895966, 0.000000000000000000 ) ) ;
#6289 = VECTOR ( 'NONE', #18396, 1000.000000000000000 ) ;
#6290 = VECTOR ( 'NONE', #6246, 1000.000000000000000 ) ;
#6291 = LINE ( 'NONE', #796, #8735 ) ;
#6293 = ORIENTED_EDGE ( 'NONE', *, *, #5264, .T. ) ;
#6292 = VECTOR ( 'NONE', #3632, 1000.000000000000000 ) ;
#6294 = CYLINDRICAL_SURFACE ( 'NONE', #28637, 16.19999999999999574 ) ;
#6296 = CARTESIAN_POINT ( 'NONE',  ( -20.02113311122478123, 14.09580098603202458, -67.50000000000000000 ) ) ;
#6295 = DIRECTION ( 'NONE',  ( 0.000000000000000000, 0.000000000000000000, 1.000000000000000000 ) ) ;
#6297 = EDGE_LOOP ( 'NONE', ( #30395, #7999, #9613, #2501 ) ) ;
#6298 = ADVANCED_FACE ( 'NONE', ( #8873 ), #30068, .T. ) ;
#6299 = EDGE_CURVE ( 'NONE', #21605, #12335, #31338, .T. ) ;
#6300 = DIRECTION ( 'NONE',  ( -1.000000000000000000, 0.000000000000000000, 0.000000000000000000 ) ) ;
#6301 = DIRECTION ( 'NONE',  ( 0.000000000000000000, 3.374343856708137958E-53, -1.000000000000000000 ) ) ;
#6302 = ORIENTED_EDGE ( 'NONE', *, *, #27872, .F. ) ;
#6303 = EDGE_CURVE ( 'NONE', #1235, #639, #19749, .T. ) ;
#6304 = ORIENTED_EDGE ( 'NONE', *, *, #10010, .T. ) ;
#6305 = VECTOR ( 'NONE', #24797, 1000.000000000000114 ) ;
#6306 = VERTEX_POINT ( 'NONE', #11207 ) ;
#6307 = DIRECTION ( 'NONE',  ( -0.1617819965527638459, -0.9868265225415262520, 0.000000000000000000 ) ) ;
#6308 = ORIENTED_EDGE ( 'NONE', *, *, #23622, .F. ) ;
#6309 = EDGE_LOOP ( 'NONE', ( #5149, #24298, #16187, #26347, #3356, #27566 ) ) ;
#6310 = FACE_BOUND ( 'NONE', #6100, .T. ) ;
#6311 = PRODUCT_DEFINITION_SHAPE ( 'NONE', 'NONE',  #35171 ) ;
#6312 = DIRECTION ( 'NONE',  ( -0.000000000000000000, 0.8660254037844383745, 0.5000000000000005551 ) ) ;
#6313 = CARTESIAN_POINT ( 'NONE',  ( -449.9999999999999432, 104.9999999999999858, -187.0000000000000000 ) ) ;
#6314 = AXIS2_PLACEMENT_3D ( 'NONE', #14281, #24931, #11421 ) ;
#6315 = CARTESIAN_POINT ( 'NONE',  ( 1.040000000000002034, 28.00026196654299326, -20.00929742917092824 ) ) ;
#6316 = VERTEX_POINT ( 'NONE', #14052 ) ;
#6317 = ORIENTED_EDGE ( 'NONE', *, *, #14527, .T. ) ;
#6318 = VECTOR ( 'NONE', #12498, 1000.000000000000000 ) ;
#6319 = DIRECTION ( 'NONE',  ( 0.000000000000000000, 0.000000000000000000, -1.000000000000000000 ) ) ;
#6320 = DIRECTION ( 'NONE',  ( 3.697785493223492838E-32, 1.934419779023891545E-16, -1.000000000000000000 ) ) ;
#6321 = AXIS2_PLACEMENT_3D ( 'NONE', #24738, #13378, #29567 ) ;
#6322 = CIRCLE ( 'NONE', #28518, 7.999999999999979572 ) ;
#6323 = DIRECTION ( 'NONE',  ( 1.000000000000000000, 0.000000000000000000, 0.000000000000000000 ) ) ;
#6324 = LINE ( 'NONE', #1697, #11322 ) ;
#6325 = CYLINDRICAL_SURFACE ( 'NONE', #31365, 4.750000000000004441 ) ;
#6326 = ADVANCED_FACE ( 'NONE', ( #11560 ), #25056, .T. ) ;
#6327 = EDGE_CURVE ( 'NONE', #11423, #31622, #9388, .T. ) ;
#6328 = CARTESIAN_POINT ( 'NONE',  ( -10.00000000000000000, 0.000000000000000000, 0.000000000000000000 ) ) ;
#6329 = PLANE ( 'NONE',  #11343 ) ;
#6330 = ORIENTED_EDGE ( 'NONE', *, *, #2919, .T. ) ;
#6331 = CARTESIAN_POINT ( 'NONE',  ( 11.99999999999999645, -115.0000000000000142, 162.9999999999999716 ) ) ;
#6332 = ADVANCED_FACE ( 'NONE', ( #3706 ), #30764, .F. ) ;
#6333 = CARTESIAN_POINT ( 'NONE',  ( -12.00000000000001066, 144.9999999999999716, -190.9999999999999432 ) ) ;
#6334 = AXIS2_PLACEMENT_3D ( 'NONE', #11645, #17169, #27999 ) ;
#6335 = CARTESIAN_POINT ( 'NONE',  ( -20.00000000000007461, 144.9999999999999716, -162.9999999999999716 ) ) ;
#6336 = VERTEX_POINT ( 'NONE', #6014 ) ;
#6337 = EDGE_CURVE ( 'NONE', #18108, #26418, #11376, .T. ) ;
#6338 = EDGE_CURVE ( 'NONE', #6590, #9496, #28683, .T. ) ;
#6339 = CARTESIAN_POINT ( 'NONE',  ( -499.9999999999999432, 140.9999999999999716, -162.9999999999999716 ) ) ;
#6340 = ORIENTED_EDGE ( 'NONE', *, *, #23149, .F. ) ;
#6341 = PRESENTATION_STYLE_ASSIGNMENT (( #30740 ) ) ;
#6342 = CARTESIAN_POINT ( 'NONE',  ( -101.1521832138544994, 3.386225727737903313, 12.03506400121763065 ) ) ;
#6343 = VECTOR ( 'NONE', #10831, 1000.000000000000000 ) ;
#6345 = VERTEX_POINT ( 'NONE', #1049 ) ;
#6344 = VECTOR ( 'NONE', #25559, 1000.000000000000000 ) ;
#6346 = AXIS2_PLACEMENT_3D ( 'NONE', #25396, #1028, #11895 ) ;
#6347 = CARTESIAN_POINT ( 'NONE',  ( 0.02407890056655695096, -8.112136323389137260, 30.01377904834206589 ) ) ;
#6348 = AXIS2_PLACEMENT_3D ( 'NONE', #6189, #17450, #12274 ) ;
#6349 = DIRECTION ( 'NONE',  ( 0.000000000000000000, 1.310824597558155437E-49, 1.000000000000000000 ) ) ;
#6350 = FACE_OUTER_BOUND ( 'NONE', #28169, .T. ) ;
#6351 = VECTOR ( 'NONE', #11934, 1000.000000000000000 ) ;
#6352 = ORIENTED_EDGE ( 'NONE', *, *, #11580, .F. ) ;
#6353 = DIRECTION ( 'NONE',  ( 0.1063910735369155841, -0.9943243633099125844, -3.335902418025060287E-15 ) ) ;
#6354 = CARTESIAN_POINT ( 'NONE',  ( 0.000000000000000000, 3.524919873834583163E-15, 68.31122994652405112 ) ) ;
#6355 = EDGE_CURVE ( 'NONE', #21781, #13694, #16482, .T. ) ;
#6356 = ORIENTED_EDGE ( 'NONE', *, *, #25539, .F. ) ;
#6357 = PLANE ( 'NONE',  #22949 ) ;
#6358 = CARTESIAN_POINT ( 'NONE',  ( -414.0000000000000568, 104.9999999999999858, -162.9999999999999716 ) ) ;
#6359 = DIRECTION ( 'NONE',  ( -1.000000000000000000, -0.000000000000000000, -0.000000000000000000 ) ) ;
#6360 = DIRECTION ( 'NONE',  ( -0.000000000000000000, 0.000000000000000000, -1.000000000000000000 ) ) ;
#6361 = ITEM_DEFINED_TRANSFORMATION ( 'NONE', 'NONE', #26342,  #28566 ) ;
#6362 = ORIENTED_EDGE ( 'NONE', *, *, #11901, .F. ) ;
#6363 = ORIENTED_EDGE ( 'NONE', *, *, #18028, .F. ) ;
#6364 = ORIENTED_EDGE ( 'NONE', *, *, #22218, .T. ) ;
#6365 = PRODUCT_DEFINITION_SHAPE ( 'NONE', 'NONE',  #35099 ) ;
#6366 = EDGE_CURVE ( 'NONE', #5175, #13611, #5836, .T. ) ;
#6367 = LINE ( 'NONE', #3872, #10304 ) ;
#6368 = ADVANCED_FACE ( 'NONE', ( #19571 ), #30416, .F. ) ;
#6369 = EDGE_CURVE ( 'NONE', #1848, #27507, #23290, .T. ) ;
#6370 = DIRECTION ( 'NONE',  ( 0.000000000000000000, 1.000000000000000000, 1.224646799147353207E-16 ) ) ;
#6371 = LINE ( 'NONE', #1050, #10265 ) ;
#6373 = VERTEX_POINT ( 'NONE', #26122 ) ;
#6372 = VECTOR ( 'NONE', #16839, 1000.000000000000000 ) ;
#6374 = ORIENTED_EDGE ( 'NONE', *, *, #3857, .F. ) ;
#6375 = DIRECTION ( 'NONE',  ( 0.000000000000000000, 0.000000000000000000, -1.000000000000000000 ) ) ;
#6376 = AXIS2_PLACEMENT_3D ( 'NONE', #29826, #27316, #24640 ) ;
#6377 = DIRECTION ( 'NONE',  ( -1.000000000000000000, -0.000000000000000000, -0.000000000000000000 ) ) ;
#6378 = ORIENTED_EDGE ( 'NONE', *, *, #12545, .F. ) ;
#6379 = DIRECTION ( 'NONE',  ( 0.000000000000000000, 0.000000000000000000, -1.000000000000000000 ) ) ;
#6380 = CARTESIAN_POINT ( 'NONE',  ( 110.1470437452871920, 2.564129753321950478, 12.23925059504672674 ) ) ;
#6381 = EDGE_LOOP ( 'NONE', ( #3221, #22225, #34631, #10297 ) ) ;
#6382 = ORIENTED_EDGE ( 'NONE', *, *, #20035, .T. ) ;
#6383 = CARTESIAN_POINT ( 'NONE',  ( -499.9999999999999432, 136.9999999999999432, 194.9999999999999716 ) ) ;
#6384 = LINE ( 'NONE', #9763, #19506 ) ;
#6385 = ORIENTED_EDGE ( 'NONE', *, *, #3405, .T. ) ;
#6386 = LINE ( 'NONE', #17281, #22618 ) ;
#6387 = CARTESIAN_POINT ( 'NONE',  ( -1.307386931792819285, 32.51914993179678959, 68.31122994652405112 ) ) ;
#6388 = FACE_OUTER_BOUND ( 'NONE', #28269, .T. ) ;
#6389 = CARTESIAN_POINT ( 'NONE',  ( -103.6615931442450602, -4.948512067686756666, 11.47900473831605161 ) ) ;
#6390 = DIRECTION ( 'NONE',  ( -1.000000000000000000, -0.000000000000000000, -0.000000000000000000 ) ) ;
#6391 = CARTESIAN_POINT ( 'NONE',  ( 1.040000000000001590, -33.26546734453813059, -8.820166447042128155 ) ) ;
#6392 = ORIENTED_EDGE ( 'NONE', *, *, #9137, .F. ) ;
#6393 = CIRCLE ( 'NONE', #21163, 11.79999999999999893 ) ;
#6394 = ORIENTED_EDGE ( 'NONE', *, *, #2611, .T. ) ;
#6395 = VECTOR ( 'NONE', #14779, 1000.000000000000000 ) ;
#6396 = PRESENTATION_LAYER_ASSIGNMENT (  '', '', ( #17237 ) ) ;
#6397 = CARTESIAN_POINT ( 'NONE',  ( 836.0535958641626166, 1170.855996841597289, 1753.598338701303419 ) ) ;
#6398 = VERTEX_POINT ( 'NONE', #28623 ) ;
#6399 = ORIENTED_EDGE ( 'NONE', *, *, #11262, .F. ) ;
#6400 = CARTESIAN_POINT ( 'NONE',  ( 2.719010730813550047, 12.21472555652470326, 29.24628546289466868 ) ) ;
#6401 = CARTESIAN_POINT ( 'NONE',  ( 3.235562306570555532E-30, 14.09580098603202636, -87.50000000000000000 ) ) ;
#6402 = VERTEX_POINT ( 'NONE', #28279 ) ;
#6403 = DIRECTION ( 'NONE',  ( 0.000000000000000000, 1.000000000000000000, 2.465190328815662439E-32 ) ) ;
#6404 = EDGE_CURVE ( 'NONE', #28665, #20300, #33230, .T. ) ;
#6405 = EDGE_CURVE ( 'NONE', #19566, #34661, #21870, .T. ) ;
#6407 = DIRECTION ( 'NONE',  ( -0.9868265225415260300, 0.1617819965527648174, 0.000000000000000000 ) ) ;
#6406 = CARTESIAN_POINT ( 'NONE',  ( -12.00000000000001066, -124.9999999999999432, -154.9999999999999716 ) ) ;
#6408 = EDGE_LOOP ( 'NONE', ( #2110, #32877, #26075, #21112 ) ) ;
#6409 = VERTEX_POINT ( 'NONE', #31633 ) ;
#6410 = DIRECTION ( 'NONE',  ( -0.000000000000000000, 1.000000000000000000, -0.000000000000000000 ) ) ;
#6411 = ADVANCED_FACE ( 'NONE', ( #25954 ), #23123, .T. ) ;
#6412 = FACE_OUTER_BOUND ( 'NONE', #33615, .T. ) ;
#6413 = CARTESIAN_POINT ( 'NONE',  ( -32.32899628990712415, -3.747048406849356361, 15.81122994652406355 ) ) ;
#6414 = DIRECTION ( 'NONE',  ( 0.8276889981568901211, 0.5611870653623829419, 0.000000000000000000 ) ) ;
#6415 = ORIENTED_EDGE ( 'NONE', *, *, #26079, .T. ) ;
#6416 =( GEOMETRIC_REPRESENTATION_CONTEXT ( 3 ) GLOBAL_UNCERTAINTY_ASSIGNED_CONTEXT ( ( #12114 ) ) GLOBAL_UNIT_ASSIGNED_CONTEXT ( ( #20850, #12680, #7306 ) ) REPRESENTATION_CONTEXT ( 'NONE', 'WORKASPACE' ) );
#6417 = DIRECTION ( 'NONE',  ( -0.000000000000000000, 1.836970198721029934E-16, -1.000000000000000000 ) ) ;
#6418 = CARTESIAN_POINT ( 'NONE',  ( 22.10765473302597073, -14.55883922869198166, -87.50000000000000000 ) ) ;
#6419 = VECTOR ( 'NONE', #6518, 1000.000000000000000 ) ;
#6420 = VECTOR ( 'NONE', #16754, 1000.000000000000000 ) ;
#6421 = AXIS2_PLACEMENT_3D ( 'NONE', #22118, #29595, #21936 ) ;
#6422 = ORIENTED_EDGE ( 'NONE', *, *, #5189, .T. ) ;
#6423 = DIRECTION ( 'NONE',  ( 1.000000000000000000, 0.000000000000000000, 0.000000000000000000 ) ) ;
#6424 = PLANE ( 'NONE',  #19433 ) ;
#6425 = EDGE_CURVE ( 'NONE', #22922, #16360, #9752, .T. ) ;
#6426 = DIRECTION ( 'NONE',  ( -1.000000000000000000, 0.000000000000000000, 0.000000000000000000 ) ) ;
#6428 = CARTESIAN_POINT ( 'NONE',  ( -410.0000000000000568, -105.0000000000001279, 132.0000000000000000 ) ) ;
#6427 = CARTESIAN_POINT ( 'NONE',  ( 12.00000000000001066, -134.9999999999999716, 187.0000000000000000 ) ) ;
#6429 = DIRECTION ( 'NONE',  ( 0.000000000000000000, 0.000000000000000000, 1.000000000000000000 ) ) ;
#6430 = FACE_OUTER_BOUND ( 'NONE', #21986, .T. ) ;
#6431 = ORIENTED_EDGE ( 'NONE', *, *, #30379, .F. ) ;
#6432 = DIRECTION ( 'NONE',  ( 0.000000000000000000, 0.000000000000000000, 1.000000000000000000 ) ) ;
#6433 = DIRECTION ( 'NONE',  ( 0.000000000000000000, 0.000000000000000000, 1.000000000000000000 ) ) ;
#6434 = VECTOR ( 'NONE', #29766, 1000.000000000000000 ) ;
#6435 = VERTEX_POINT ( 'NONE', #18147 ) ;
#6436 = ORIENTED_EDGE ( 'NONE', *, *, #19742, .F. ) ;
#6437 = AXIS2_PLACEMENT_3D ( 'NONE', #15842, #16012, #1935 ) ;
#6438 = AXIS2_PLACEMENT_3D ( 'NONE', #33185, #11311, #22161 ) ;
#6439 = AXIS2_PLACEMENT_3D ( 'NONE', #16797, #6426, #25475 ) ;
#6440 = ORIENTED_EDGE ( 'NONE', *, *, #12810, .T. ) ;
#6441 = DIRECTION ( 'NONE',  ( -0.000000000000000000, -1.836970198721029688E-16, 1.000000000000000000 ) ) ;
#6442 = ORIENTED_EDGE ( 'NONE', *, *, #30901, .F. ) ;
#6443 = ORIENTED_EDGE ( 'NONE', *, *, #24356, .F. ) ;
#6444 = CARTESIAN_POINT ( 'NONE',  ( -418.0000000000000000, 137.0000000000000000, -155.0000000000000000 ) ) ;
#6445 = EDGE_CURVE ( 'NONE', #18794, #11635, #6725, .T. ) ;
#6446 = CONTEXT_DEPENDENT_SHAPE_REPRESENTATION ( #3075, #9861 ) ;
#6447 = ORIENTED_EDGE ( 'NONE', *, *, #15359, .F. ) ;
#6448 = CARTESIAN_POINT ( 'NONE',  ( 15.99999999999998579, 112.9999999999999574, -155.0000000000000000 ) ) ;
#6449 = LINE ( 'NONE', #22495, #1193 ) ;
#6450 = EDGE_LOOP ( 'NONE', ( #28105, #26436, #33959, #10670 ) ) ;
#6451 = ORIENTED_EDGE ( 'NONE', *, *, #21013, .T. ) ;
#6452 =( REPRESENTATION_RELATIONSHIP ('NONE','NONE', #23037, #15767 ) REPRESENTATION_RELATIONSHIP_WITH_TRANSFORMATION ( #1213 )SHAPE_REPRESENTATION_RELATIONSHIP( ) );
#6453 = LINE ( 'NONE', #3957, #913 ) ;
#6454 = CARTESIAN_POINT ( 'NONE',  ( -8.499999999999998224, 0.000000000000000000, 3.930000000000000160 ) ) ;
#6455 = EDGE_CURVE ( 'NONE', #32595, #4812, #1574, .T. ) ;
#6456 = EDGE_CURVE ( 'NONE', #32399, #7575, #25591, .T. ) ;
#6457 = LINE ( 'NONE', #21403, #3354 ) ;
#6458 = CARTESIAN_POINT ( 'NONE',  ( -20.00000000000004619, -137.0000000000000000, -187.0000000000000000 ) ) ;
#6459 = FACE_BOUND ( 'NONE', #25958, .T. ) ;
#6460 = VERTEX_POINT ( 'NONE', #4559 ) ;
#6461 = CARTESIAN_POINT ( 'NONE',  ( 9.199999999999999289, 7.794228634059932048, -13.49999999999999822 ) ) ;
#6462 = CIRCLE ( 'NONE', #33171, 8.000000000000007105 ) ;
#6463 = EDGE_CURVE ( 'NONE', #16235, #33086, #26413, .T. ) ;
#6464 = EDGE_CURVE ( 'NONE', #17403, #7548, #9417, .T. ) ;
#6465 = FACE_OUTER_BOUND ( 'NONE', #9531, .T. ) ;
#6466 = ORIENTED_EDGE ( 'NONE', *, *, #8929, .T. ) ;
#6467 = CARTESIAN_POINT ( 'NONE',  ( 0.8386200322165776599, 14.95253250404440237, 1.101454001170010244 ) ) ;
#6468 = DIRECTION ( 'NONE',  ( 1.000000000000000000, 3.040835319149746528E-31, 1.232595164407830946E-32 ) ) ;
#6469 = PLANE ( 'NONE',  #4720 ) ;
#6470 = ADVANCED_FACE ( 'NONE', ( #7242 ), #31289, .T. ) ;
#6471 = AXIS2_PLACEMENT_3D ( 'NONE', #29125, #7225, #7756 ) ;
#6472 = CARTESIAN_POINT ( 'NONE',  ( 102.0984371113816991, 4.963291960430601613, -5.628698742319545367 ) ) ;
#6473 = FILL_AREA_STYLE_COLOUR ( '', #16236 ) ;
#6474 = CIRCLE ( 'NONE', #34328, 2.525000000000000355 ) ;
#6475 = AXIS2_PLACEMENT_3D ( 'NONE', #23983, #10994, #7787 ) ;
#6476 = DIRECTION ( 'NONE',  ( 0.000000000000000000, 0.000000000000000000, -1.000000000000000000 ) ) ;
#6477 = ORIENTED_EDGE ( 'NONE', *, *, #33441, .F. ) ;
#6478 = DIRECTION ( 'NONE',  ( -1.000000000000000000, 0.000000000000000000, -0.000000000000000000 ) ) ;
#6480 = DIRECTION ( 'NONE',  ( 1.000000000000000000, 0.000000000000000000, 0.000000000000000000 ) ) ;
#6479 = LINE ( 'NONE', #17378, #27416 ) ;
#6481 = AXIS2_PLACEMENT_3D ( 'NONE', #13079, #15571, #26409 ) ;
#6482 = ORIENTED_EDGE ( 'NONE', *, *, #23666, .T. ) ;
#6483 = LINE ( 'NONE', #3294, #8612 ) ;
#6484 = ORIENTED_EDGE ( 'NONE', *, *, #28737, .F. ) ;
#6485 = ORIENTED_EDGE ( 'NONE', *, *, #3056, .F. ) ;
#6486 = AXIS2_PLACEMENT_3D ( 'NONE', #3644, #5603, #19694 ) ;
#6487 = ORIENTED_EDGE ( 'NONE', *, *, #23617, .F. ) ;
#6488 = DIRECTION ( 'NONE',  ( -1.000000000000000000, 0.000000000000000000, 0.000000000000000000 ) ) ;
#6489 = ORIENTED_EDGE ( 'NONE', *, *, #25794, .T. ) ;
#6490 = VERTEX_POINT ( 'NONE', #6552 ) ;
#6491 = DIRECTION ( 'NONE',  ( 0.000000000000000000, 0.000000000000000000, 1.000000000000000000 ) ) ;
#6492 = AXIS2_PLACEMENT_3D ( 'NONE', #25629, #17655, #12477 ) ;
#6493 = CARTESIAN_POINT ( 'NONE',  ( 1.532562817202168137, 32.50931595846690669, 68.31122994652405112 ) ) ;
#6494 = CARTESIAN_POINT ( 'NONE',  ( 0.000000000000000000, 3.524919873834583163E-15, 68.31122994652405112 ) ) ;
#6495 = VECTOR ( 'NONE', #30656, 1000.000000000000000 ) ;
#6496 = CARTESIAN_POINT ( 'NONE',  ( 2.789999999999999147, 13.51972826729810961, 27.27250221666296071 ) ) ;
#6497 = CARTESIAN_POINT ( 'NONE',  ( -349.0000000000000000, -125.0000000000000284, 130.0000000000000000 ) ) ;
#6498 = VERTEX_POINT ( 'NONE', #6892 ) ;
#6499 = ORIENTED_EDGE ( 'NONE', *, *, #23373, .F. ) ;
#6500 = AXIS2_PLACEMENT_3D ( 'NONE', #18556, #1797, #31690 ) ;
#6501 = LINE ( 'NONE', #1004, #32710 ) ;
#6502 = FACE_OUTER_BOUND ( 'NONE', #5892, .T. ) ;
#6503 = DIRECTION ( 'NONE',  ( -1.000000000000000000, 0.000000000000000000, -1.300283923313630633E-47 ) ) ;
#6504 = CIRCLE ( 'NONE', #32089, 7.999999999999952038 ) ;
#6505 = CARTESIAN_POINT ( 'NONE',  ( -130.6469666100234406, 6.000000000000000000, 57.49999999999999289 ) ) ;
#6506 = CARTESIAN_POINT ( 'NONE',  ( 2.789999999999999147, -30.43331811787860275, -0.6209492052235439097 ) ) ;
#6507 = CARTESIAN_POINT ( 'NONE',  ( -355.0000000000000000, 132.9999999999999716, 126.0000000000000000 ) ) ;
#6508 = EDGE_CURVE ( 'NONE', #24429, #33545, #26295, .T. ) ;
#6509 = EDGE_CURVE ( 'NONE', #34482, #30531, #17306, .T. ) ;
#6510 = CARTESIAN_POINT ( 'NONE',  ( 2.789999999999999147, 28.29688452313417812, -12.88099432405573630 ) ) ;
#6511 = ORIENTED_EDGE ( 'NONE', *, *, #24255, .F. ) ;
#6512 = B_SPLINE_CURVE_WITH_KNOTS ( 'NONE', 3,
 ( #4517, #26952, #21442, #34443 ),
 .UNSPECIFIED., .F., .F.,
 ( 4, 4 ),
 ( 0.005298346188946806770, 0.005985214897255182465 ),
 .UNSPECIFIED. ) ;
#6513 = CARTESIAN_POINT ( 'NONE',  ( 0.02407890056655695096, 30.61125888652961891, 5.439165181699118889 ) ) ;
#6514 = DIRECTION ( 'NONE',  ( 0.000000000000000000, 1.000000000000000000, 0.000000000000000000 ) ) ;
#6515 = DIRECTION ( 'NONE',  ( 1.000000000000000000, -0.000000000000000000, -0.000000000000000000 ) ) ;
#6516 = VERTEX_POINT ( 'NONE', #1738 ) ;
#6517 = VECTOR ( 'NONE', #17914, 1000.000000000000000 ) ;
#6518 = DIRECTION ( 'NONE',  ( 1.000000000000000000, -0.000000000000000000, -0.000000000000000000 ) ) ;
#6519 = ORIENTED_EDGE ( 'NONE', *, *, #10665, .T. ) ;
#6520 = CARTESIAN_POINT ( 'NONE',  ( 11.99999999999999645, -141.0000000000000000, 174.9999999999999432 ) ) ;
#6521 = VECTOR ( 'NONE', #28447, 1000.000000000000000 ) ;
#6522 = LINE ( 'NONE', #27887, #22214 ) ;
#6523 = EDGE_CURVE ( 'NONE', #20123, #12309, #12610, .T. ) ;
#6524 = DIRECTION ( 'NONE',  ( 0.02168945059047637514, 0.9997647561967180074, -6.640585699268911402E-15 ) ) ;
#6525 = AXIS2_PLACEMENT_3D ( 'NONE', #9807, #31518, #14651 ) ;
#6526 = ORIENTED_EDGE ( 'NONE', *, *, #3732, .T. ) ;
#6527 = AXIS2_PLACEMENT_3D ( 'NONE', #17471, #6210, #1241 ) ;
#6528 = CYLINDRICAL_SURFACE ( 'NONE', #1233, 3.999999999999976019 ) ;
#6529 = FACE_OUTER_BOUND ( 'NONE', #21562, .T. ) ;
#6530 = CARTESIAN_POINT ( 'NONE',  ( -410.0000000000000568, 104.9999999999999858, -187.0000000000000000 ) ) ;
#6531 = EDGE_CURVE ( 'NONE', #1296, #10318, #17449, .T. ) ;
#6532 = ORIENTED_EDGE ( 'NONE', *, *, #33927, .T. ) ;
#6533 = EDGE_CURVE ( 'NONE', #16288, #6803, #9935, .T. ) ;
#6534 = EDGE_CURVE ( 'NONE', #27049, #1376, #7772, .T. ) ;
#6535 = CARTESIAN_POINT ( 'NONE',  ( 782.9713044643401645, 1094.157880131287357, 1753.598338701303419 ) ) ;
#6536 = DIRECTION ( 'NONE',  ( -1.000000000000000000, 0.000000000000000000, 0.000000000000000000 ) ) ;
#6537 = ORIENTED_EDGE ( 'NONE', *, *, #12360, .F. ) ;
#6538 = LINE ( 'NONE', #17437, #3638 ) ;
#6539 = EDGE_CURVE ( 'NONE', #10340, #7014, #34372, .T. ) ;
#6540 = PLANE ( 'NONE',  #23252 ) ;
#6541 = VECTOR ( 'NONE', #27992, 1000.000000000000000 ) ;
#6542 = LINE ( 'NONE', #23443, #27694 ) ;
#6543 = DIRECTION ( 'NONE',  ( 0.000000000000000000, 0.000000000000000000, 1.000000000000000000 ) ) ;
#6544 = ORIENTED_EDGE ( 'NONE', *, *, #9052, .T. ) ;
#6545 = ORIENTED_EDGE ( 'NONE', *, *, #3165, .F. ) ;
#6546 = ORIENTED_EDGE ( 'NONE', *, *, #15233, .F. ) ;
#6547 = AXIS2_PLACEMENT_3D ( 'NONE', #23087, #24278, #7735 ) ;
#6548 = CARTESIAN_POINT ( 'NONE',  ( -20.02113311122478123, 14.09580098603202813, -87.50000000000000000 ) ) ;
#6549 = VECTOR ( 'NONE', #3488, 1000.000000000000000 ) ;
#6550 = CARTESIAN_POINT ( 'NONE',  ( 29.82459402470855281, 33.69708579775584667, -36.68877005347593467 ) ) ;
#6551 = ORIENTED_EDGE ( 'NONE', *, *, #17155, .T. ) ;
#6552 = CARTESIAN_POINT ( 'NONE',  ( 30.69344702212033127, -10.82204614554912325, 49.43553178847298568 ) ) ;
#6553 = DIRECTION ( 'NONE',  ( 0.000000000000000000, -0.000000000000000000, 1.000000000000000000 ) ) ;
#6554 = ORIENTED_EDGE ( 'NONE', *, *, #1990, .F. ) ;
#6555 = EDGE_CURVE ( 'NONE', #34864, #26182, #18491, .T. ) ;
#6556 = VECTOR ( 'NONE', #6349, 1000.000000000000000 ) ;
#6557 = CARTESIAN_POINT ( 'NONE',  ( 15.99999999999998579, 144.9999999999999716, 162.9999999999999716 ) ) ;
#6558 = DIRECTION ( 'NONE',  ( 0.000000000000000000, 1.000000000000000000, 1.224646799147353207E-16 ) ) ;
#6559 = VERTEX_POINT ( 'NONE', #34666 ) ;
#6560 = AXIS2_PLACEMENT_3D ( 'NONE', #18245, #28739, #20903 ) ;
#6561 = FACE_OUTER_BOUND ( 'NONE', #1719, .T. ) ;
#6562 = CARTESIAN_POINT ( 'NONE',  ( 8.000000000000000000, 0.000000000000000000, 0.000000000000000000 ) ) ;
#6563 = ORIENTED_EDGE ( 'NONE', *, *, #15615, .F. ) ;
#6564 = CARTESIAN_POINT ( 'NONE',  ( 2.719010706573971703, -24.04031276246385929, 20.65449384219750684 ) ) ;
#6565 = EDGE_LOOP ( 'NONE', ( #11510, #6692, #3131, #10627 ) ) ;
#6566 = CARTESIAN_POINT ( 'NONE',  ( -99.88497961182919482, 6.264410040187948829E-16, -12.50000000000000000 ) ) ;
#6567 = CARTESIAN_POINT ( 'NONE',  ( -15.99999999999998579, -137.0000000000000000, -155.0000000000000284 ) ) ;
#6568 = CARTESIAN_POINT ( 'NONE',  ( 11.99999999999999645, -115.0000000000000142, 162.9999999999999716 ) ) ;
#6569 = VECTOR ( 'NONE', #12475, 1000.000000000000000 ) ;
#6570 = CARTESIAN_POINT ( 'NONE',  ( -108.8497219713561179, -3.384384043357604899, 12.03563115889556201 ) ) ;
#6571 = CARTESIAN_POINT ( 'NONE',  ( -442.0000000000000000, 105.0000000000000142, 155.0000000000000000 ) ) ;
#6572 = DIRECTION ( 'NONE',  ( 0.000000000000000000, 0.000000000000000000, 1.000000000000000000 ) ) ;
#6573 = VECTOR ( 'NONE', #14149, 1000.000000000000000 ) ;
#6574 = VERTEX_POINT ( 'NONE', #15636 ) ;
#6575 = EDGE_CURVE ( 'NONE', #17921, #24256, #7414, .T. ) ;
#6576 = EDGE_CURVE ( 'NONE', #28395, #17757, #19007, .T. ) ;
#6577 = ORIENTED_EDGE ( 'NONE', *, *, #1243, .F. ) ;
#6578 = CARTESIAN_POINT ( 'NONE',  ( 779.5135964574884611, 1126.473404339538547, 1753.598338701302964 ) ) ;
#6579 = ORIENTED_EDGE ( 'NONE', *, *, #35041, .T. ) ;
#6580 = VECTOR ( 'NONE', #11975, 1000.000000000000114 ) ;
#6581 = LINE ( 'NONE', #33463, #15254 ) ;
#6582 = CARTESIAN_POINT ( 'NONE',  ( 1.749999999999999778, 0.000000000000000000, 0.000000000000000000 ) ) ;
#6583 = ORIENTED_EDGE ( 'NONE', *, *, #14966, .F. ) ;
#6584 = DIRECTION ( 'NONE',  ( 0.000000000000000000, 0.000000000000000000, 1.000000000000000000 ) ) ;
#6585 = CARTESIAN_POINT ( 'NONE',  ( -108.3801912069810101, -3.853301823223607592, -11.89378582241139171 ) ) ;
#6586 = CONTEXT_DEPENDENT_SHAPE_REPRESENTATION ( #4218, #28905 ) ;
#6587 = AXIS2_PLACEMENT_3D ( 'NONE', #5740, #27652, #5570 ) ;
#6589 = PLANE ( 'NONE',  #5025 ) ;
#6588 = LINE ( 'NONE', #20137, #33797 ) ;
#6590 = VERTEX_POINT ( 'NONE', #21656 ) ;
#6591 = ORIENTED_EDGE ( 'NONE', *, *, #11112, .T. ) ;
#6592 = LINE ( 'NONE', #17659, #5468 ) ;
#6593 = CIRCLE ( 'NONE', #919, 2.524999999999999911 ) ;
#6594 = DIRECTION ( 'NONE',  ( 1.000000000000000000, 0.000000000000000000, 0.000000000000000000 ) ) ;
#6595 = DIRECTION ( 'NONE',  ( 1.000000000000000000, 0.000000000000000000, 0.000000000000000000 ) ) ;
#6596 = ORIENTED_EDGE ( 'NONE', *, *, #872, .T. ) ;
#6597 = CARTESIAN_POINT ( 'NONE',  ( 2.719051674741964852, 29.95509811880031492, 10.35390711157494081 ) ) ;
#6598 = LINE ( 'NONE', #30472, #8990 ) ;
#6599 = ORIENTED_EDGE ( 'NONE', *, *, #1120, .T. ) ;
#6600 = VECTOR ( 'NONE', #17102, 1000.000000000000000 ) ;
#6601 = DIRECTION ( 'NONE',  ( -0.000000000000000000, 1.000000000000000000, -0.000000000000000000 ) ) ;
#6602 = LINE ( 'NONE', #22650, #15444 ) ;
#6603 = CARTESIAN_POINT ( 'NONE',  ( 0.1835381450695051930, 32.14582644238494424, 2.841494734165256109 ) ) ;
#6605 = CARTESIAN_POINT ( 'NONE',  ( 19.99999999999998934, -115.0000000000000000, 162.9999999999999716 ) ) ;
#6604 = CARTESIAN_POINT ( 'NONE',  ( -365.0000000000000000, -119.0000000000000000, 126.0000000000000000 ) ) ;
#6606 = CARTESIAN_POINT ( 'NONE',  ( 0.7561992064972459238, 13.95859842408671447, -30.90949138205555968 ) ) ;
#6607 = CARTESIAN_POINT ( 'NONE',  ( 2.715598927533382057, 28.97026656347592777, 12.96367524219944833 ) ) ;
#6608 = ORIENTED_EDGE ( 'NONE', *, *, #3397, .T. ) ;
#6609 = DIRECTION ( 'NONE',  ( 0.000000000000000000, -2.309213040847544338E-50, -1.000000000000000000 ) ) ;
#6610 = CARTESIAN_POINT ( 'NONE',  ( 15.99999999999998579, -55.00000000000002132, 162.9999999999999716 ) ) ;
#6611 = PRODUCT_DEFINITION_SHAPE ( 'NONE', 'NONE',  #35128 ) ;
#6612 = EDGE_CURVE ( 'NONE', #7619, #20342, #24143, .T. ) ;
#6613 = ADVANCED_FACE ( 'NONE', ( #4921 ), #15986, .T. ) ;
#6614 = VECTOR ( 'NONE', #19095, 1000.000000000000000 ) ;
#6615 = ADVANCED_FACE ( 'NONE', ( #29329 ), #31806, .T. ) ;
#6616 = ORIENTED_EDGE ( 'NONE', *, *, #23864, .F. ) ;
#6617 = PRODUCT_RELATED_PRODUCT_CATEGORY ( 'part', '', ( #14046 ) ) ;
#6618 = VECTOR ( 'NONE', #18623, 1000.000000000000000 ) ;
#6619 = ORIENTED_EDGE ( 'NONE', *, *, #33489, .T. ) ;
#6620 = DIRECTION ( 'NONE',  ( -1.000000000000000000, 0.000000000000000000, 0.000000000000000000 ) ) ;
#6621 = ORIENTED_EDGE ( 'NONE', *, *, #10961, .F. ) ;
#6622 = ORIENTED_EDGE ( 'NONE', *, *, #30430, .T. ) ;
#6623 = ORIENTED_EDGE ( 'NONE', *, *, #13076, .F. ) ;
#6624 = CARTESIAN_POINT ( 'NONE',  ( -19.99999999999998934, 144.9999999999999716, -162.9999999999999432 ) ) ;
#6625 = AXIS2_PLACEMENT_3D ( 'NONE', #7346, #10210, #28729 ) ;
#6626 = ITEM_DEFINED_TRANSFORMATION ( 'NONE', 'NONE', #20116,  #28566 ) ;
#6627 = ORIENTED_EDGE ( 'NONE', *, *, #14795, .T. ) ;
#6628 = DIRECTION ( 'NONE',  ( 1.000000000000000000, 0.000000000000000000, 0.000000000000000000 ) ) ;
#6629 = FACE_BOUND ( 'NONE', #9584, .T. ) ;
#6630 = ORIENTED_EDGE ( 'NONE', *, *, #28256, .F. ) ;
#6631 = ORIENTED_EDGE ( 'NONE', *, *, #22348, .F. ) ;
#6632 = LINE ( 'NONE', #17532, #32202 ) ;
#6633 = CARTESIAN_POINT ( 'NONE',  ( -12.25939112814508825, 30.14816249862104058, -36.68877005347593467 ) ) ;
#6634 = VECTOR ( 'NONE', #22644, 1000.000000000000000 ) ;
#6635 = DIRECTION ( 'NONE',  ( -0.000000000000000000, -0.000000000000000000, -1.000000000000000000 ) ) ;
#6636 = CARTESIAN_POINT ( 'NONE',  ( -500.0000000000000000, -145.0000000000000000, 162.9999999999999716 ) ) ;
#6637 = DIRECTION ( 'NONE',  ( -0.7960930657056433102, -0.6051742151937656855, -0.000000000000000000 ) ) ;
#6638 = ORIENTED_EDGE ( 'NONE', *, *, #11580, .T. ) ;
#6640 = VECTOR ( 'NONE', #30947, 1000.000000000000114 ) ;
#6639 = CARTESIAN_POINT ( 'NONE',  ( 9.199999999999999289, 0.000000000000000000, -13.50000000000000000 ) ) ;
#6641 = CARTESIAN_POINT ( 'NONE',  ( -35.00000000000000000, 16.36947364650383818, 36.69637551990492597 ) ) ;
#6642 = CARTESIAN_POINT ( 'NONE',  ( -30.58418286738120884, -22.31615353445080174, 68.31122994652405112 ) ) ;
#6643 = VERTEX_POINT ( 'NONE', #23808 ) ;
#6644 = CARTESIAN_POINT ( 'NONE',  ( -355.0000000000000000, 116.9999999999999858, 126.0000000000000000 ) ) ;
#6645 = FACE_OUTER_BOUND ( 'NONE', #12953, .T. ) ;
#6646 = PLANE ( 'NONE',  #18380 ) ;
#6647 = CARTESIAN_POINT ( 'NONE',  ( 102.4136796593249130, 5.135442232304142429, -5.469792608531489186 ) ) ;
#6649 =( NAMED_UNIT ( * ) PLANE_ANGLE_UNIT ( ) SI_UNIT ( $, .RADIAN. ) );
#6648 = DIRECTION ( 'NONE',  ( 0.000000000000000000, 1.000000000000000000, 5.145227585319922065E-49 ) ) ;
#6650 = ADVANCED_FACE ( 'NONE', ( #32164 ), #13134, .T. ) ;
#6651 = VECTOR ( 'NONE', #14581, 999.9999999999998863 ) ;
#6652 = DIRECTION ( 'NONE',  ( -1.000000000000000000, -0.000000000000000000, 0.000000000000000000 ) ) ;
#6653 = ORIENTED_EDGE ( 'NONE', *, *, #27300, .T. ) ;
#6654 = DIRECTION ( 'NONE',  ( 0.000000000000000000, 1.000000000000000000, 1.131431318426415506E-52 ) ) ;
#6656 = DIRECTION ( 'NONE',  ( -1.000000000000000000, -0.000000000000000000, -0.000000000000000000 ) ) ;
#6655 = FACE_OUTER_BOUND ( 'NONE', #20955, .T. ) ;
#6657 = ADVANCED_FACE ( 'NONE', ( #2433 ), #26650, .T. ) ;
#6658 = ORIENTED_EDGE ( 'NONE', *, *, #9863, .F. ) ;
#6659 = PRODUCT_DEFINITION_SHAPE ( 'NONE', 'NONE',  #35107 ) ;
#6660 = DIRECTION ( 'NONE',  ( -0.000000000000000000, -0.000000000000000000, -1.000000000000000000 ) ) ;
#6661 = EDGE_CURVE ( 'NONE', #9347, #14830, #29142, .T. ) ;
#6662 = ORIENTED_EDGE ( 'NONE', *, *, #2830, .T. ) ;
#6663 = CIRCLE ( 'NONE', #22587, 32.54542015209057126 ) ;
#6664 = CIRCLE ( 'NONE', #29969, 7.999999999999979572 ) ;
#6665 = EDGE_CURVE ( 'NONE', #17833, #8779, #7590, .T. ) ;
#6666 = APPLICATION_CONTEXT ( 'automotive_design' ) ;
#6667 = ORIENTED_EDGE ( 'NONE', *, *, #28306, .F. ) ;
#6668 = FACE_OUTER_BOUND ( 'NONE', #27881, .T. ) ;
#6669 = VERTEX_POINT ( 'NONE', #10104 ) ;
#6670 = ORIENTED_EDGE ( 'NONE', *, *, #21764, .F. ) ;
#6671 = LINE ( 'NONE', #17394, #6517 ) ;
#6672 = EDGE_CURVE ( 'NONE', #3550, #1172, #21492, .T. ) ;
#6673 = ADVANCED_FACE ( 'NONE', ( #12964 ), #4251, .T. ) ;
#6675 = CARTESIAN_POINT ( 'NONE',  ( 2.261199747612499422, 21.87231946537488270, 25.22857168675692563 ) ) ;
#6674 = AXIS2_PLACEMENT_3D ( 'NONE', #26120, #1907, #20442 ) ;
#6676 = DIRECTION ( 'NONE',  ( 0.000000000000000000, 0.000000000000000000, -1.000000000000000000 ) ) ;
#6677 = CARTESIAN_POINT ( 'NONE',  ( 0.02407890056655695096, 30.61125888652969707, -5.439165181698684570 ) ) ;
#6678 = ORIENTED_EDGE ( 'NONE', *, *, #34837, .F. ) ;
#6679 = ORIENTED_EDGE ( 'NONE', *, *, #4467, .T. ) ;
#6680 = DIRECTION ( 'NONE',  ( -1.000000000000000000, 0.000000000000000000, 0.000000000000000000 ) ) ;
#6681 = LINE ( 'NONE', #25549, #15219 ) ;
#6682 = DIRECTION ( 'NONE',  ( 0.000000000000000000, 0.000000000000000000, -1.000000000000000000 ) ) ;
#6683 = DIRECTION ( 'NONE',  ( 3.469446951953832974E-18, 1.000000000000000000, 7.888609052210116302E-31 ) ) ;
#6684 = CYLINDRICAL_SURFACE ( 'NONE', #20583, 1.155000000000000027 ) ;
#6685 = DIRECTION ( 'NONE',  ( -0.000000000000000000, -0.000000000000000000, -1.000000000000000000 ) ) ;
#6686 = CIRCLE ( 'NONE', #17519, 14.77500000000000036 ) ;
#6687 = CARTESIAN_POINT ( 'NONE',  ( -499.9999999999998863, -109.0000000000000142, -162.9999999999999716 ) ) ;
#6688 = ORIENTED_EDGE ( 'NONE', *, *, #23302, .T. ) ;
#6689 = DIRECTION ( 'NONE',  ( -1.000000000000000000, -0.000000000000000000, -0.000000000000000000 ) ) ;
#6690 = DIRECTION ( 'NONE',  ( -1.000000000000000000, 0.000000000000000000, -1.300283923313630633E-47 ) ) ;
#6691 = DIRECTION ( 'NONE',  ( 0.000000000000000000, 0.000000000000000000, -1.000000000000000000 ) ) ;
#6692 = ORIENTED_EDGE ( 'NONE', *, *, #5280, .F. ) ;
#6693 = AXIS2_PLACEMENT_3D ( 'NONE', #8337, #29531, #5125 ) ;
#6694 = AXIS2_PLACEMENT_3D ( 'NONE', #3370, #19239, #19588 ) ;
#6695 = DIRECTION ( 'NONE',  ( -0.8835120444460227151, -0.4684084406997905403, -8.604523463949019211E-17 ) ) ;
#6696 = ORIENTED_EDGE ( 'NONE', *, *, #13553, .T. ) ;
#6697 = CARTESIAN_POINT ( 'NONE',  ( -12.00000000000001066, -124.9999999999999432, -154.9999999999999716 ) ) ;
#6698 = LINE ( 'NONE', #15962, #6855 ) ;
#6699 = CIRCLE ( 'NONE', #27150, 7.999999999999979572 ) ;
#6700 = ORIENTED_EDGE ( 'NONE', *, *, #21011, .F. ) ;
#6701 = CARTESIAN_POINT ( 'NONE',  ( 0.02407890056655695096, -21.56796757982795043, -22.39322359481629476 ) ) ;
#6702 = LINE ( 'NONE', #23434, #12275 ) ;
#6703 = CARTESIAN_POINT ( 'NONE',  ( 2.789999999999999147, 29.44518845714764765, 9.980709654879525772 ) ) ;
#6704 = ADVANCED_FACE ( 'NONE', ( #5269 ), #21134, .T. ) ;
#6705 = ORIENTED_EDGE ( 'NONE', *, *, #14218, .T. ) ;
#6706 = EDGE_CURVE ( 'NONE', #23628, #16142, #12801, .T. ) ;
#6707 = ADVANCED_FACE ( 'NONE', ( #17229 ), #32685, .T. ) ;
#6708 = CARTESIAN_POINT ( 'NONE',  ( 789.8867204780439124, 1029.526831714783839, 1753.598338701303419 ) ) ;
#6709 = DIRECTION ( 'NONE',  ( 0.000000000000000000, 0.000000000000000000, 1.000000000000000000 ) ) ;
#6710 = ORIENTED_EDGE ( 'NONE', *, *, #19615, .T. ) ;
#6711 = FACE_OUTER_BOUND ( 'NONE', #11643, .T. ) ;
#6712 = CARTESIAN_POINT ( 'NONE',  ( 127.4999999999999147, 0.000000000000000000, 0.000000000000000000 ) ) ;
#6713 = VECTOR ( 'NONE', #20126, 1000.000000000000000 ) ;
#6714 = DIRECTION ( 'NONE',  ( -0.000000000000000000, -0.000000000000000000, -1.000000000000000000 ) ) ;
#6715 = DIRECTION ( 'NONE',  ( -0.000000000000000000, 1.000000000000000000, -0.000000000000000000 ) ) ;
#6716 = CONTEXT_DEPENDENT_SHAPE_REPRESENTATION ( #13077, #28800 ) ;
#6717 = VERTEX_POINT ( 'NONE', #22017 ) ;
#6719 = ORIENTED_EDGE ( 'NONE', *, *, #13733, .T. ) ;
#6718 =( REPRESENTATION_RELATIONSHIP ('NONE','NONE', #23037, #28231 ) REPRESENTATION_RELATIONSHIP_WITH_TRANSFORMATION ( #22675 )SHAPE_REPRESENTATION_RELATIONSHIP( ) );
#6720 = ORIENTED_EDGE ( 'NONE', *, *, #34835, .T. ) ;
#6721 = DIRECTION ( 'NONE',  ( 0.000000000000000000, 3.374343856708137958E-53, -1.000000000000000000 ) ) ;
#6722 = ADVANCED_FACE ( 'NONE', ( #27873 ), #17050, .T. ) ;
#6723 = FACE_BOUND ( 'NONE', #34036, .T. ) ;
#6724 = VECTOR ( 'NONE', #32768, 1000.000000000000000 ) ;
#6725 = LINE ( 'NONE', #17618, #8220 ) ;
#6726 = DIRECTION ( 'NONE',  ( 1.000000000000000000, 0.000000000000000000, -1.232595164407831220E-32 ) ) ;
#6727 = CARTESIAN_POINT ( 'NONE',  ( -418.0000000000000000, 109.0000000000000142, -175.0000000000000000 ) ) ;
#6728 = DIRECTION ( 'NONE',  ( 0.000000000000000000, 1.000000000000000000, 1.224646799147353207E-16 ) ) ;
#6729 = ORIENTED_EDGE ( 'NONE', *, *, #5576, .F. ) ;
#6730 = EDGE_CURVE ( 'NONE', #28532, #26055, #832, .T. ) ;
#6731 = CARTESIAN_POINT ( 'NONE',  ( 109.5450345215125196, 3.507529710008592705, 11.99873639479134546 ) ) ;
#6732 = AXIS2_PLACEMENT_3D ( 'NONE', #11381, #11213, #30241 ) ;
#6734 = EDGE_CURVE ( 'NONE', #14082, #11787, #19353, .T. ) ;
#6733 = ORIENTED_EDGE ( 'NONE', *, *, #29169, .T. ) ;
#6735 = PLANE ( 'NONE',  #27115 ) ;
#6736 = AXIS2_PLACEMENT_3D ( 'NONE', #8916, #33118, #8734 ) ;
#6737 = EDGE_CURVE ( 'NONE', #19775, #3490, #14195, .T. ) ;
#6738 = CARTESIAN_POINT ( 'NONE',  ( -418.0000000000000000, -105.0000000000000142, 132.0000000000000000 ) ) ;
#6739 = EDGE_LOOP ( 'NONE', ( #1477, #6443, #9689, #18085 ) ) ;
#6740 = CARTESIAN_POINT ( 'NONE',  ( -5.823698994896893133, -1.505030548027689319, -0.7520000000000004459 ) ) ;
#6741 = CARTESIAN_POINT ( 'NONE',  ( -355.0000000000000000, -131.0000000000000000, 130.0000000000000000 ) ) ;
#6742 = EDGE_CURVE ( 'NONE', #34333, #17794, #305, .T. ) ;
#6743 = DIRECTION ( 'NONE',  ( 0.000000000000000000, 0.000000000000000000, -1.000000000000000000 ) ) ;
#6744 = VECTOR ( 'NONE', #24515, 1000.000000000000000 ) ;
#6745 = CARTESIAN_POINT ( 'NONE',  ( -101.1547991473559449, -3.377194313163046857, 12.03587146382073847 ) ) ;
#6746 = UNCERTAINTY_MEASURE_WITH_UNIT (LENGTH_MEASURE( 1.000000000000000082E-05 ), #22080, 'distance_accuracy_value', 'NONE');
#6747 = DIRECTION ( 'NONE',  ( 1.000000000000000000, 3.469446951953834515E-18, 0.000000000000000000 ) ) ;
#6748 = CARTESIAN_POINT ( 'NONE',  ( -9.978866888775733912, -15.68591377522703745, -67.50000000000000000 ) ) ;
#6749 = VERTEX_POINT ( 'NONE', #9019 ) ;
#6750 = AXIS2_PLACEMENT_3D ( 'NONE', #22899, #25556, #33751 ) ;
#6751 = ORIENTED_EDGE ( 'NONE', *, *, #4751, .F. ) ;
#6752 = EDGE_CURVE ( 'NONE', #27456, #32641, #655, .T. ) ;
#6753 = EDGE_CURVE ( 'NONE', #33261, #22350, #4831, .T. ) ;
#6754 = DIRECTION ( 'NONE',  ( -7.893605728314050488E-14, 1.618803117314786135E-15, 0.9999999999999998890 ) ) ;
#6755 = ORIENTED_EDGE ( 'NONE', *, *, #21763, .F. ) ;
#6756 = DIRECTION ( 'NONE',  ( 0.000000000000000000, 0.000000000000000000, 1.000000000000000000 ) ) ;
#6757 = CIRCLE ( 'NONE', #15887, 30.47050528711511674 ) ;
#6758 = DIRECTION ( 'NONE',  ( -1.000000000000000000, 0.000000000000000000, 0.000000000000000000 ) ) ;
#6759 = ORIENTED_EDGE ( 'NONE', *, *, #20942, .F. ) ;
#6760 = CARTESIAN_POINT ( 'NONE',  ( 3.235562306570555532E-30, -15.68591377522703745, -67.50000000000000000 ) ) ;
#6761 = CARTESIAN_POINT ( 'NONE',  ( -106.3384068557549256, -4.948512067686755778, -11.47900473831604806 ) ) ;
#6762 = VECTOR ( 'NONE', #8821, 1000.000000000000000 ) ;
#6764 = DIRECTION ( 'NONE',  ( -1.000000000000000000, -0.000000000000000000, -0.000000000000000000 ) ) ;
#6763 = LINE ( 'NONE', #25810, #11057 ) ;
#6765 = ORIENTED_EDGE ( 'NONE', *, *, #24038, .F. ) ;
#6766 = EDGE_LOOP ( 'NONE', ( #13472, #19921, #33190, #17211, #8108, #18893 ) ) ;
#6767 = FACE_OUTER_BOUND ( 'NONE', #5491, .T. ) ;
#6768 = CARTESIAN_POINT ( 'NONE',  ( -15.99999999999998579, -124.9999999999999432, -186.9999999999999716 ) ) ;
#6769 = DIRECTION ( 'NONE',  ( 0.000000000000000000, 2.465190328815661892E-32, 1.000000000000000000 ) ) ;
#6770 = ORIENTED_EDGE ( 'NONE', *, *, #25841, .T. ) ;
#6771 = VECTOR ( 'NONE', #14334, 1000.000000000000114 ) ;
#6772 = EDGE_CURVE ( 'NONE', #16556, #6917, #16874, .T. ) ;
#6773 = EDGE_CURVE ( 'NONE', #33264, #31774, #24482, .T. ) ;
#6774 = DIRECTION ( 'NONE',  ( 0.000000000000000000, 1.000000000000000000, -0.000000000000000000 ) ) ;
#6775 = ORIENTED_EDGE ( 'NONE', *, *, #22145, .T. ) ;
#6776 = CARTESIAN_POINT ( 'NONE',  ( -14.84098889165989377, 28.96462362251113376, -36.68877005347593467 ) ) ;
#6777 = FACE_OUTER_BOUND ( 'NONE', #13202, .T. ) ;
#6778 = EDGE_CURVE ( 'NONE', #15484, #28564, #124, .T. ) ;
#6779 = LINE ( 'NONE', #31683, #25200 ) ;
#6781 = DIRECTION ( 'NONE',  ( 0.5155538571770231782, 0.8568571761675883858, -0.000000000000000000 ) ) ;
#6780 = DIRECTION ( 'NONE',  ( 0.000000000000000000, 0.000000000000000000, -1.000000000000000000 ) ) ;
#6782 = VECTOR ( 'NONE', #26036, 1000.000000000000000 ) ;
#6784 = EDGE_CURVE ( 'NONE', #9096, #8875, #1448, .T. ) ;
#6783 = FACE_OUTER_BOUND ( 'NONE', #31838, .T. ) ;
#6785 = DIRECTION ( 'NONE',  ( 0.000000000000000000, 1.000000000000000000, 5.145227585319922065E-49 ) ) ;
#6786 = VERTEX_POINT ( 'NONE', #21829 ) ;
#6787 = CARTESIAN_POINT ( 'NONE',  ( 19.99999999999998224, -55.00000000000000711, -158.9999999999999716 ) ) ;
#6788 = PLANE ( 'NONE',  #25742 ) ;
#6789 = ORIENTED_EDGE ( 'NONE', *, *, #2836, .T. ) ;
#6790 =( LENGTH_UNIT ( ) NAMED_UNIT ( * ) SI_UNIT ( .MILLI., .METRE. ) );
#6791 = ORIENTED_EDGE ( 'NONE', *, *, #21853, .F. ) ;
#6792 = VECTOR ( 'NONE', #30176, 1000.000000000000000 ) ;
#6793 = CARTESIAN_POINT ( 'NONE',  ( 0.000000000000000000, 17.98401995359632011, 24.59729088254965035 ) ) ;
#6794 = ORIENTED_EDGE ( 'NONE', *, *, #25399, .T. ) ;
#6795 = EDGE_LOOP ( 'NONE', ( #1895, #13308, #6191, #10098, #5320, #31122, #7485, #14753 ) ) ;
#6796 = ORIENTED_EDGE ( 'NONE', *, *, #1677, .F. ) ;
#6797 = EDGE_CURVE ( 'NONE', #34550, #8996, #27698, .T. ) ;
#6798 = DIRECTION ( 'NONE',  ( 1.000000000000000000, 3.469446951953834515E-18, 0.000000000000000000 ) ) ;
#6799 = ITEM_DEFINED_TRANSFORMATION ( 'NONE', 'NONE', #32028,  #28566 ) ;
#6800 = EDGE_LOOP ( 'NONE', ( #824, #27580, #34472, #3677, #29955, #10962 ) ) ;
#6801 = DIRECTION ( 'NONE',  ( 0.000000000000000000, 0.000000000000000000, -1.000000000000000000 ) ) ;
#6802 = DIRECTION ( 'NONE',  ( 0.000000000000000000, 0.000000000000000000, 1.000000000000000000 ) ) ;
#6803 = VERTEX_POINT ( 'NONE', #16515 ) ;
#6804 = VERTEX_POINT ( 'NONE', #24847 ) ;
#6805 = DIRECTION ( 'NONE',  ( 2.736911063134582149E-48, -7.888609052210118054E-31, -1.000000000000000000 ) ) ;
#6806 = CARTESIAN_POINT ( 'NONE',  ( 32.30227131129397833, -3.970848902647440060, 68.31122994652405112 ) ) ;
#6807 = ADVANCED_FACE ( 'NONE', ( #27341 ), #14528, .T. ) ;
#6808 = DIRECTION ( 'NONE',  ( -1.000000000000000000, 0.000000000000000000, 0.000000000000000000 ) ) ;
#6809 = DIRECTION ( 'NONE',  ( -0.2149704402110243773, -0.9766205557100865464, -0.000000000000000000 ) ) ;
#6810 = DIRECTION ( 'NONE',  ( -1.848892746611746419E-32, -6.842277657836020854E-49, 1.000000000000000000 ) ) ;
#6811 = ORIENTED_EDGE ( 'NONE', *, *, #8034, .F. ) ;
#6812 = EDGE_CURVE ( 'NONE', #11236, #2088, #16690, .T. ) ;
#6813 = LINE ( 'NONE', #28543, #21465 ) ;
#6814 = CARTESIAN_POINT ( 'NONE',  ( -365.0000000000000000, 134.9999999999999716, 126.0000000000000000 ) ) ;
#6815 = EDGE_CURVE ( 'NONE', #13866, #2454, #31276, .T. ) ;
#6816 = B_SPLINE_CURVE_WITH_KNOTS ( 'NONE', 3,
 ( #30477, #27449, #8572, #220, #32780, #5539 ),
 .UNSPECIFIED., .F., .F.,
 ( 4, 2, 4 ),
 ( 1.978042196653065176E-07, 0.001873396096185922770, 0.003746594388152190303 ),
 .UNSPECIFIED. ) ;
#6817 = CARTESIAN_POINT ( 'NONE',  ( -430.0000000000000000, -119.0000000000000000, 113.9999999999999858 ) ) ;
#6818 = ORIENTED_EDGE ( 'NONE', *, *, #24185, .T. ) ;
#6819 = CARTESIAN_POINT ( 'NONE',  ( 19.99999999999998224, 144.9999999999999716, -186.9999999999999716 ) ) ;
#6820 = LINE ( 'NONE', #3444, #18342 ) ;
#6821 = DIRECTION ( 'NONE',  ( -0.000000000000000000, -0.000000000000000000, -1.000000000000000000 ) ) ;
#6822 = CARTESIAN_POINT ( 'NONE',  ( 0.02407890056655695096, 20.99477179376825120, 22.93149026599753526 ) ) ;
#6824 = CARTESIAN_POINT ( 'NONE',  ( -418.0000000000000000, -125.0000000000000000, -101.9999999999999858 ) ) ;
#6823 = DIRECTION ( 'NONE',  ( 0.000000000000000000, 0.000000000000000000, 1.000000000000000000 ) ) ;
#6825 = CARTESIAN_POINT ( 'NONE',  ( 1.394999999999999574, -24.90160365674885057, 23.75493189058332533 ) ) ;
#6826 = EDGE_LOOP ( 'NONE', ( #21832, #10796 ) ) ;
#6827 = CARTESIAN_POINT ( 'NONE',  ( 10.17231796313411429, 15.60017778382161246, -77.50000000000000000 ) ) ;
#6829 = DIRECTION ( 'NONE',  ( 0.000000000000000000, 0.000000000000000000, -1.000000000000000000 ) ) ;
#6828 = LINE ( 'NONE', #28558, #12096 ) ;
#6830 = ORIENTED_EDGE ( 'NONE', *, *, #9360, .T. ) ;
#6831 = DIRECTION ( 'NONE',  ( -1.000000000000000000, -0.000000000000000000, -0.000000000000000000 ) ) ;
#6832 = ORIENTED_EDGE ( 'NONE', *, *, #12805, .F. ) ;
#6833 = VERTEX_POINT ( 'NONE', #23414 ) ;
#6834 = CARTESIAN_POINT ( 'NONE',  ( 109.5174362172994620, -3.557362730766958858, -6.611294427798556583 ) ) ;
#6835 = ORIENTED_EDGE ( 'NONE', *, *, #11062, .F. ) ;
#6836 = VERTEX_POINT ( 'NONE', #33564 ) ;
#6837 = CIRCLE ( 'NONE', #23342, 3.999999999999948042 ) ;
#6838 = CARTESIAN_POINT ( 'NONE',  ( -20.02113311122498729, -5.758675521474012626, -87.50000000000000000 ) ) ;
#6839 = FACE_OUTER_BOUND ( 'NONE', #15655, .T. ) ;
#6840 = DIRECTION ( 'NONE',  ( 0.000000000000000000, 0.000000000000000000, -1.000000000000000000 ) ) ;
#6841 = CARTESIAN_POINT ( 'NONE',  ( -449.9999999999999432, -105.0000000000000142, -101.9999999999999858 ) ) ;
#6842 = ORIENTED_EDGE ( 'NONE', *, *, #1334, .F. ) ;
#6843 = EDGE_LOOP ( 'NONE', ( #30038, #3681, #30506, #7916 ) ) ;
#6844 = ADVANCED_FACE ( 'NONE', ( #12055 ), #23253, .T. ) ;
#6845 = LINE ( 'NONE', #26076, #25888 ) ;
#6846 = DIRECTION ( 'NONE',  ( -1.000000000000000000, -0.000000000000000000, -0.000000000000000000 ) ) ;
#6847 = CARTESIAN_POINT ( 'NONE',  ( 8.000000000000000000, 0.000000000000000000, 0.000000000000000000 ) ) ;
#6848 = EDGE_CURVE ( 'NONE', #763, #9401, #7201, .T. ) ;
#6849 = DIRECTION ( 'NONE',  ( 0.000000000000000000, 1.000000000000000000, 5.145227585319922065E-49 ) ) ;
#6850 = DIRECTION ( 'NONE',  ( 1.000000000000000000, 0.000000000000000000, 0.000000000000000000 ) ) ;
#6851 = DIRECTION ( 'NONE',  ( 0.000000000000000000, 0.000000000000000000, 1.000000000000000000 ) ) ;
#6852 = ADVANCED_FACE ( 'NONE', ( #20409 ), #25378, .F. ) ;
#6853 = CARTESIAN_POINT ( 'NONE',  ( 0.1835381660689911765, -18.30111164264862111, -26.58002197185247439 ) ) ;
#6854 = VERTEX_POINT ( 'NONE', #1702 ) ;
#6855 = VECTOR ( 'NONE', #24287, 1000.000000000000000 ) ;
#6856 = EDGE_CURVE ( 'NONE', #17691, #2320, #33926, .T. ) ;
#6857 = CARTESIAN_POINT ( 'NONE',  ( 2.719051659378652896, -11.11627562454391338, -29.68062877649334652 ) ) ;
#6858 = CARTESIAN_POINT ( 'NONE',  ( 0.7561992259563318219, 31.33438324387140383, -12.97673134914391824 ) ) ;
#6859 = DIRECTION ( 'NONE',  ( 0.000000000000000000, 0.000000000000000000, -1.000000000000000000 ) ) ;
#6860 = VERTEX_POINT ( 'NONE', #34094 ) ;
#6861 = PLANE ( 'NONE',  #23473 ) ;
#6862 = ORIENTED_EDGE ( 'NONE', *, *, #16343, .T. ) ;
#6863 = AXIS2_PLACEMENT_3D ( 'NONE', #21268, #18101, #18615 ) ;
#6865 = CARTESIAN_POINT ( 'NONE',  ( -19.99999999999998934, -141.0000000000000000, 162.9999999999999716 ) ) ;
#6864 = FILL_AREA_STYLE_COLOUR ( '', #24478 ) ;
#6866 = CARTESIAN_POINT ( 'NONE',  ( -3.250000000000000000, 5.404196845913421754, 5.429999999999999716 ) ) ;
#6867 = ADVANCED_FACE ( 'NONE', ( #4004 ), #32690, .T. ) ;
#6868 = VECTOR ( 'NONE', #28045, 1000.000000000000000 ) ;
#6869 = VERTEX_POINT ( 'NONE', #11881 ) ;
#6870 = LINE ( 'NONE', #28602, #12624 ) ;
#6871 = CARTESIAN_POINT ( 'NONE',  ( 2.790000000000080416, -14.96425809615007907, 26.76330950827329147 ) ) ;
#6872 = VERTEX_POINT ( 'NONE', #17748 ) ;
#6873 = AXIS2_PLACEMENT_3D ( 'NONE', #10149, #2300, #26339 ) ;
#6874 = DIRECTION ( 'NONE',  ( 2.631201909438060585E-14, -5.396010391056496978E-16, 1.000000000000000000 ) ) ;
#6875 = AXIS2_PLACEMENT_3D ( 'NONE', #22252, #8719, #14614 ) ;
#6876 = VECTOR ( 'NONE', #3287, 1000.000000000000000 ) ;
#6877 = DIRECTION ( 'NONE',  ( 1.000000000000000000, 0.000000000000000000, 0.000000000000000000 ) ) ;
#6878 = VERTEX_POINT ( 'NONE', #28238 ) ;
#6879 = AXIS2_PLACEMENT_3D ( 'NONE', #14649, #22815, #9288 ) ;
#6880 = CARTESIAN_POINT ( 'NONE',  ( -500.0000000000000000, -113.0000000000000000, 162.9999999999999716 ) ) ;
#6881 = DIRECTION ( 'NONE',  ( 1.000000000000000000, 0.000000000000000000, 0.000000000000000000 ) ) ;
#6882 = CARTESIAN_POINT ( 'NONE',  ( -442.0000000000000000, -137.0000000000000000, -175.0000000000000000 ) ) ;
#6883 = DIRECTION ( 'NONE',  ( -1.000000000000000000, -0.000000000000000000, -0.000000000000000000 ) ) ;
#6884 = EDGE_LOOP ( 'NONE', ( #7265, #19306, #12856, #30916 ) ) ;
#6885 = EDGE_LOOP ( 'NONE', ( #5966, #29158, #14846, #24386 ) ) ;
#6886 = VERTEX_POINT ( 'NONE', #14552 ) ;
#6887 = AXIS2_PLACEMENT_3D ( 'NONE', #26909, #8039, #30110 ) ;
#6888 = PLANE ( 'NONE',  #26569 ) ;
#6889 = EDGE_CURVE ( 'NONE', #13897, #14045, #15109, .T. ) ;
#6891 = AXIS2_PLACEMENT_3D ( 'NONE', #17693, #7320, #4642 ) ;
#6890 = DIRECTION ( 'NONE',  ( -1.000000000000000000, 0.000000000000000000, 0.000000000000000000 ) ) ;
#6892 = CARTESIAN_POINT ( 'NONE',  ( -499.9999999999999432, 104.9999999999999858, -187.0000000000000000 ) ) ;
#6893 = DIRECTION ( 'NONE',  ( -0.1617819965527614312, 0.9868265225415265851, 0.000000000000000000 ) ) ;
#6894 = LINE ( 'NONE', #23125, #6074 ) ;
#6895 = CARTESIAN_POINT ( 'NONE',  ( -414.0000000000000568, 105.0000000000000000, -77.99999999999997158 ) ) ;
#6896 = ORIENTED_EDGE ( 'NONE', *, *, #1922, .F. ) ;
#6897 = EDGE_CURVE ( 'NONE', #14920, #18737, #9189, .T. ) ;
#6898 = PRODUCT_DEFINITION_SHAPE ( 'NONE', 'NONE',  #35149 ) ;
#6899 = EDGE_CURVE ( 'NONE', #22009, #199, #18522, .T. ) ;
#6900 = CARTESIAN_POINT ( 'NONE',  ( 1.040000000000002034, 32.09669216789253454, -12.41728656686340315 ) ) ;
#6901 = ORIENTED_EDGE ( 'NONE', *, *, #31218, .F. ) ;
#6902 = AXIS2_PLACEMENT_3D ( 'NONE', #14201, #3145, #22373 ) ;
#6903 = ADVANCED_FACE ( 'NONE', ( #22730 ), #20576, .F. ) ;
#6904 = ADVANCED_FACE ( 'NONE', ( #17929, #1179, #20062 ), #28755, .F. ) ;
#6905 = VECTOR ( 'NONE', #18847, 1000.000000000000000 ) ;
#6906 = DIRECTION ( 'NONE',  ( 0.000000000000000000, 0.000000000000000000, 1.000000000000000000 ) ) ;
#6907 = ORIENTED_EDGE ( 'NONE', *, *, #26043, .T. ) ;
#6908 = VECTOR ( 'NONE', #27016, 1000.000000000000000 ) ;
#6909 = CARTESIAN_POINT ( 'NONE',  ( 2.765921099433441999, -23.70329957282570632, -20.11932597908854703 ) ) ;
#6910 = PLANE ( 'NONE',  #5326 ) ;
#6911 = DIRECTION ( 'NONE',  ( 0.000000000000000000, 0.000000000000000000, -1.000000000000000000 ) ) ;
#6912 = CARTESIAN_POINT ( 'NONE',  ( -1.030735741678193484, 1.713938105891546826, -0.7500000000000000000 ) ) ;
#6913 = CARTESIAN_POINT ( 'NONE',  ( 11.99999999999999645, -145.0000000000000000, -190.9999999999999432 ) ) ;
#6915 = EDGE_CURVE ( 'NONE', #5282, #23190, #11753, .T. ) ;
#6914 = ORIENTED_EDGE ( 'NONE', *, *, #27258, .T. ) ;
#6916 = VECTOR ( 'NONE', #13650, 1000.000000000000000 ) ;
#6917 = VERTEX_POINT ( 'NONE', #9886 ) ;
#6918 = DIRECTION ( 'NONE',  ( -7.893605728314050488E-14, 1.618803117314786135E-15, 0.9999999999999998890 ) ) ;
#6919 =( REPRESENTATION_RELATIONSHIP ('NONE','NONE', #23037, #15767 ) REPRESENTATION_RELATIONSHIP_WITH_TRANSFORMATION ( #18303 )SHAPE_REPRESENTATION_RELATIONSHIP( ) );
#6920 = EDGE_LOOP ( 'NONE', ( #14207, #24959, #21602, #28473 ) ) ;
#6921 = AXIS2_PLACEMENT_3D ( 'NONE', #18163, #5292, #12814 ) ;
#6922 = DIRECTION ( 'NONE',  ( 1.000000000000000000, 0.000000000000000000, 0.000000000000000000 ) ) ;
#6923 = EDGE_CURVE ( 'NONE', #1214, #13897, #31597, .T. ) ;
#6924 = ADVANCED_FACE ( 'NONE', ( #33748 ), #34400, .T. ) ;
#6925 = AXIS2_PLACEMENT_3D ( 'NONE', #13977, #13617, #21623 ) ;
#6926 = CARTESIAN_POINT ( 'NONE',  ( 44.94043929807611448, -20.15143121711728469, 20.00000000000000000 ) ) ;
#6927 = AXIS2_PLACEMENT_3D ( 'NONE', #15795, #26623, #10431 ) ;
#6928 = EDGE_LOOP ( 'NONE', ( #17966, #30775, #4998, #10249, #22700, #868, #21703, #20860 ) ) ;
#6929 = CIRCLE ( 'NONE', #30157, 1.155000000000000027 ) ;
#6930 = PLANE ( 'NONE',  #15081 ) ;
#6931 = CARTESIAN_POINT ( 'NONE',  ( 17.27856612038524631, 33.69708579775584667, 68.31122994652405112 ) ) ;
#6932 = B_SPLINE_CURVE_WITH_KNOTS ( 'NONE', 3,
 ( #2191, #26572, #7169, #31564, #13241, #12535 ),
 .UNSPECIFIED., .F., .F.,
 ( 4, 2, 4 ),
 ( 4.404817046727483726E-07, 0.001874269636018133147, 0.003748098790331593627 ),
 .UNSPECIFIED. ) ;
#6934 = DIRECTION ( 'NONE',  ( 0.000000000000000000, 0.000000000000000000, 1.000000000000000000 ) ) ;
#6933 = CARTESIAN_POINT ( 'NONE',  ( -361.0000000000000000, -125.0000000000000284, 185.0000000000000000 ) ) ;
#6935 = VERTEX_POINT ( 'NONE', #1360 ) ;
#6936 = ORIENTED_EDGE ( 'NONE', *, *, #19698, .F. ) ;
#6937 = PLANE ( 'NONE',  #25937 ) ;
#6938 = DIRECTION ( 'NONE',  ( 0.000000000000000000, 0.000000000000000000, 1.000000000000000000 ) ) ;
#6939 = CARTESIAN_POINT ( 'NONE',  ( 0.000000000000000000, 3.524919873834583163E-15, 68.31122994652405112 ) ) ;
#6940 = VERTEX_POINT ( 'NONE', #12235 ) ;
#6941 = CARTESIAN_POINT ( 'NONE',  ( 2.630124765083918348, -1.866624223957557893, 5.429999999999999716 ) ) ;
#6942 = EDGE_CURVE ( 'NONE', #13175, #25965, #26603, .T. ) ;
#6943 = EDGE_CURVE ( 'NONE', #16123, #5041, #22467, .T. ) ;
#6944 = ORIENTED_EDGE ( 'NONE', *, *, #593, .F. ) ;
#6945 = LINE ( 'NONE', #28674, #14077 ) ;
#6946 = CARTESIAN_POINT ( 'NONE',  ( 1.394999999999999574, 34.17636915695680244, 4.045051921974837761 ) ) ;
#6947 = CARTESIAN_POINT ( 'NONE',  ( -430.0000000000000000, -114.9999999999999858, 113.9999999999999858 ) ) ;
#6950 = DIRECTION ( 'NONE',  ( -0.000000000000000000, -0.000000000000000000, -1.000000000000000000 ) ) ;
#6949 = CARTESIAN_POINT ( 'NONE',  ( 2.789999999999999147, -7.837340408379732892, -29.64303704467405964 ) ) ;
#6948 = AXIS2_PLACEMENT_3D ( 'NONE', #16892, #2979, #330 ) ;
#6951 = VECTOR ( 'NONE', #536, 1000.000000000000000 ) ;
#6952 = CIRCLE ( 'NONE', #14940, 2.033421858999711951 ) ;
#6953 = AXIS2_PLACEMENT_3D ( 'NONE', #28762, #23774, #4704 ) ;
#6954 = PLANE ( 'NONE',  #30360 ) ;
#6955 = CARTESIAN_POINT ( 'NONE',  ( -430.0000000000000000, -119.0000000000000000, 109.9999999999999858 ) ) ;
#6956 = PLANE ( 'NONE',  #7053 ) ;
#6957 =( NAMED_UNIT ( * ) SI_UNIT ( $, .STERADIAN. ) SOLID_ANGLE_UNIT ( ) );
#6958 = EDGE_CURVE ( 'NONE', #32277, #4182, #29461, .T. ) ;
#6959 = ORIENTED_EDGE ( 'NONE', *, *, #29422, .T. ) ;
#6960 =( NAMED_UNIT ( * ) SI_UNIT ( $, .STERADIAN. ) SOLID_ANGLE_UNIT ( ) );
#6961 = EDGE_LOOP ( 'NONE', ( #6719, #4435, #33462, #26506 ) ) ;
#6963 = ORIENTED_EDGE ( 'NONE', *, *, #23432, .T. ) ;
#6962 = EDGE_CURVE ( 'NONE', #4948, #20279, #15950, .T. ) ;
#6964 = EDGE_CURVE ( 'NONE', #7371, #27008, #23766, .T. ) ;
#6965 = EDGE_CURVE ( 'NONE', #29430, #29579, #12925, .T. ) ;
#6966 = CYLINDRICAL_SURFACE ( 'NONE', #28413, 16.19999999999999574 ) ;
#6967 = EDGE_LOOP ( 'NONE', ( #10488, #18063 ) ) ;
#6968 = VERTEX_POINT ( 'NONE', #10065 ) ;
#6969 = VERTEX_POINT ( 'NONE', #15589 ) ;
#6970 = DIRECTION ( 'NONE',  ( -1.232595164407830946E-32, -7.496237820289040735E-63, 1.000000000000000000 ) ) ;
#6971 = EDGE_CURVE ( 'NONE', #14721, #14210, #26428, .T. ) ;
#6973 = AXIS2_PLACEMENT_3D ( 'NONE', #6041, #14622, #378 ) ;
#6972 = ITEM_DEFINED_TRANSFORMATION ( 'NONE', 'NONE', #33746,  #28566 ) ;
#6974 = VERTEX_POINT ( 'NONE', #26956 ) ;
#6975 = DIRECTION ( 'NONE',  ( -1.000000000000000000, 0.000000000000000000, 0.000000000000000000 ) ) ;
#6976 = AXIS2_PLACEMENT_3D ( 'NONE', #24494, #10991, #30037 ) ;
#6977 = DIRECTION ( 'NONE',  ( 0.000000000000000000, -1.000000000000000000, 0.000000000000000000 ) ) ;
#6978 = ORIENTED_EDGE ( 'NONE', *, *, #24789, .F. ) ;
#6979 = CIRCLE ( 'NONE', #1306, 7.999999999999979572 ) ;
#6980 = ORIENTED_EDGE ( 'NONE', *, *, #24747, .T. ) ;
#6981 = AXIS2_PLACEMENT_3D ( 'NONE', #12531, #24774, #13934 ) ;
#6982 = DIRECTION ( 'NONE',  ( 0.000000000000000000, 0.000000000000000000, -1.000000000000000000 ) ) ;
#6983 = CARTESIAN_POINT ( 'NONE',  ( -130.6469666100234406, -6.000000000000000000, 62.49999999999999289 ) ) ;
#6984 = FACE_OUTER_BOUND ( 'NONE', #3945, .T. ) ;
#6985 = DIRECTION ( 'NONE',  ( 0.000000000000000000, 1.131431318426415506E-52, 1.000000000000000000 ) ) ;
#6986 = FACE_OUTER_BOUND ( 'NONE', #14256, .T. ) ;
#6987 = ORIENTED_EDGE ( 'NONE', *, *, #2036, .T. ) ;
#6988 = CARTESIAN_POINT ( 'NONE',  ( 19.99999999999998934, -137.0000000000000000, -155.0000000000000284 ) ) ;
#6989 = FACE_OUTER_BOUND ( 'NONE', #8560, .T. ) ;
#6990 = FACE_OUTER_BOUND ( 'NONE', #14129, .T. ) ;
#6991 = ORIENTED_EDGE ( 'NONE', *, *, #11533, .T. ) ;
#6992 = CYLINDRICAL_SURFACE ( 'NONE', #34996, 2.033421858999711951 ) ;
#6993 = CARTESIAN_POINT ( 'NONE',  ( 32.81769769215650712, 18.87860345536239137, 49.43553178847298568 ) ) ;
#6994 = FACE_OUTER_BOUND ( 'NONE', #13567, .T. ) ;
#6995 = CARTESIAN_POINT ( 'NONE',  ( 110.5282433365937607, 1.549642152983123244, -7.340597171393927312 ) ) ;
#6997 = CARTESIAN_POINT ( 'NONE',  ( -103.6344077460457385, 4.941456866685308036, -5.642756420309244625 ) ) ;
#6996 = DIRECTION ( 'NONE',  ( -0.000000000000000000, 0.000000000000000000, 1.000000000000000000 ) ) ;
#6998 = AXIS2_PLACEMENT_3D ( 'NONE', #21794, #16656, #26964 ) ;
#6999 = DIRECTION ( 'NONE',  ( -0.000000000000000000, 1.000000000000000000, -0.000000000000000000 ) ) ;
#7000 = ORIENTED_EDGE ( 'NONE', *, *, #8513, .F. ) ;
#7001 = CARTESIAN_POINT ( 'NONE',  ( 110.5497257000961042, 1.507575458593801265, -12.41447922803858894 ) ) ;
#7003 = FACE_OUTER_BOUND ( 'NONE', #3637, .T. ) ;
#7002 = DIRECTION ( 'NONE',  ( 0.000000000000000000, 0.000000000000000000, 1.000000000000000000 ) ) ;
#7004 = AXIS2_PLACEMENT_3D ( 'NONE', #2458, #21347, #2116 ) ;
#7005 = ORIENTED_EDGE ( 'NONE', *, *, #27817, .F. ) ;
#7006 = AXIS2_PLACEMENT_3D ( 'NONE', #13194, #32559, #184 ) ;
#7007 = CARTESIAN_POINT ( 'NONE',  ( -15.99999999999998579, 112.9999999999999574, -155.0000000000000000 ) ) ;
#7008 = ORIENTED_EDGE ( 'NONE', *, *, #13779, .T. ) ;
#7009 = EDGE_CURVE ( 'NONE', #5551, #17531, #4522, .T. ) ;
#7010 = ADVANCED_FACE ( 'NONE', ( #20919 ), #7374, .F. ) ;
#7011 = ORIENTED_EDGE ( 'NONE', *, *, #34592, .F. ) ;
#7012 = DIRECTION ( 'NONE',  ( 1.000000000000000000, 0.000000000000000000, 0.000000000000000000 ) ) ;
#7013 = VERTEX_POINT ( 'NONE', #29103 ) ;
#7014 = VERTEX_POINT ( 'NONE', #4695 ) ;
#7015 = FACE_OUTER_BOUND ( 'NONE', #32100, .T. ) ;
#7016 = VECTOR ( 'NONE', #6061, 1000.000000000000000 ) ;
#7017 = CARTESIAN_POINT ( 'NONE',  ( 12.00000000000001066, -134.9999999999999716, 155.0000000000000000 ) ) ;
#7018 = CARTESIAN_POINT ( 'NONE',  ( -410.0000000000000568, 105.0000000000000000, 132.0000000000000000 ) ) ;
#7019 = ORIENTED_EDGE ( 'NONE', *, *, #3159, .T. ) ;
#7020 = ORIENTED_EDGE ( 'NONE', *, *, #8826, .T. ) ;
#7021 = CARTESIAN_POINT ( 'NONE',  ( 0.000000000000000000, 0.000000000000000000, 0.000000000000000000 ) ) ;
#7022 = DIRECTION ( 'NONE',  ( 0.000000000000000000, -1.000000000000000000, 0.000000000000000000 ) ) ;
#7023 = CYLINDRICAL_SURFACE ( 'NONE', #464, 2.000000000000001776 ) ;
#7024 = CARTESIAN_POINT ( 'NONE',  ( -20.00000000000007461, -113.0000000000000000, -155.0000000000000000 ) ) ;
#7025 = CARTESIAN_POINT ( 'NONE',  ( -418.0000000000000000, -124.9999999999999716, 135.9999999999999716 ) ) ;
#7026 = ORIENTED_EDGE ( 'NONE', *, *, #28804, .F. ) ;
#7027 = AXIS2_PLACEMENT_3D ( 'NONE', #4903, #2417, #28952 ) ;
#7028 = DIRECTION ( 'NONE',  ( 0.6473862847818285804, 0.7621620551276356847, 0.000000000000000000 ) ) ;
#7029 = VECTOR ( 'NONE', #5236, 1000.000000000000000 ) ;
#7030 = AXIS2_PLACEMENT_3D ( 'NONE', #33365, #28386, #31228 ) ;
#7031 = LINE ( 'NONE', #7202, #24958 ) ;
#7032 = ORIENTED_EDGE ( 'NONE', *, *, #15211, .F. ) ;
#7033 = FACE_OUTER_BOUND ( 'NONE', #18283, .T. ) ;
#7034 = CARTESIAN_POINT ( 'NONE',  ( 0.02407890056655868569, -8.112136323388726922, -30.01377904834218668 ) ) ;
#7035 = DIRECTION ( 'NONE',  ( -0.3701381553399134550, 0.9289767198167918627, 0.000000000000000000 ) ) ;
#7036 = ORIENTED_EDGE ( 'NONE', *, *, #6737, .T. ) ;
#7037 = CARTESIAN_POINT ( 'NONE',  ( -1.307386931792819285, 37.83772838912469894, 68.31122994652405112 ) ) ;
#7038 = ORIENTED_EDGE ( 'NONE', *, *, #8514, .F. ) ;
#7040 = DIRECTION ( 'NONE',  ( -1.232595164407830946E-32, 0.000000000000000000, -1.000000000000000000 ) ) ;
#7039 = DIRECTION ( 'NONE',  ( 0.000000000000000000, 0.000000000000000000, 1.000000000000000000 ) ) ;
#7041 = CYLINDRICAL_SURFACE ( 'NONE', #34147, 3.999999999999976019 ) ;
#7042 = CIRCLE ( 'NONE', #20708, 7.999999999999979572 ) ;
#7043 = ORIENTED_EDGE ( 'NONE', *, *, #2471, .T. ) ;
#7044 = CYLINDRICAL_SURFACE ( 'NONE', #9762, 9.999999999999996447 ) ;
#7045 = DIRECTION ( 'NONE',  ( 0.6876994588534236508, 0.7259954919231305093, -0.000000000000000000 ) ) ;
#7046 = VECTOR ( 'NONE', #8163, 1000.000000000000114 ) ;
#7047 = EDGE_CURVE ( 'NONE', #32367, #10757, #15774, .T. ) ;
#7048 = ORIENTED_EDGE ( 'NONE', *, *, #7445, .F. ) ;
#7049 = AXIS2_PLACEMENT_3D ( 'NONE', #17930, #1869, #15418 ) ;
#7050 = EDGE_CURVE ( 'NONE', #19630, #13520, #19076, .T. ) ;
#7051 = VECTOR ( 'NONE', #1795, 1000.000000000000000 ) ;
#7052 = CARTESIAN_POINT ( 'NONE',  ( 854.7252191011612013, 996.3521661170475454, 1753.598338701303419 ) ) ;
#7053 = AXIS2_PLACEMENT_3D ( 'NONE', #17847, #28681, #4282 ) ;
#7054 = ORIENTED_EDGE ( 'NONE', *, *, #11010, .F. ) ;
#7055 = CARTESIAN_POINT ( 'NONE',  ( 99.30043414807218483, -0.7644170489479770181, 12.48218521077886400 ) ) ;
#7056 = PRODUCT_RELATED_PRODUCT_CATEGORY ( 'part', '', ( #22877 ) ) ;
#7057 = ORIENTED_EDGE ( 'NONE', *, *, #10691, .T. ) ;
#7058 = DIRECTION ( 'NONE',  ( -0.000000000000000000, 1.836970198721029934E-16, -1.000000000000000000 ) ) ;
#7059 = CIRCLE ( 'NONE', #13337, 3.999999999999976019 ) ;
#7060 = DIRECTION ( 'NONE',  ( 0.000000000000000000, -1.000000000000000000, -3.017235169886638201E-16 ) ) ;
#7061 = CARTESIAN_POINT ( 'NONE',  ( -5.021133111224886036, 8.235406450278430768, -87.50000000000000000 ) ) ;
#7062 = DIRECTION ( 'NONE',  ( 0.8835120444460231592, -0.4684084406997896521, -0.000000000000000000 ) ) ;
#7063 = ORIENTED_EDGE ( 'NONE', *, *, #9331, .F. ) ;
#7064 = ORIENTED_EDGE ( 'NONE', *, *, #10997, .T. ) ;
#7065 = ORIENTED_EDGE ( 'NONE', *, *, #25835, .T. ) ;
#7066 = DIRECTION ( 'NONE',  ( -0.000000000000000000, -1.000000000000000000, -0.000000000000000000 ) ) ;
#7067 = CARTESIAN_POINT ( 'NONE',  ( -6.500000000000000000, 0.000000000000000000, 0.000000000000000000 ) ) ;
#7068 = AXIS2_PLACEMENT_3D ( 'NONE', #21433, #1856, #2034 ) ;
#7069 = DIRECTION ( 'NONE',  ( 1.000000000000000000, 0.000000000000000000, 0.000000000000000000 ) ) ;
#7070 = FACE_BOUND ( 'NONE', #30489, .T. ) ;
#7071 = CARTESIAN_POINT ( 'NONE',  ( -8.149999999999998579, 2.020667218593132508E-16, -0.7520000000000004459 ) ) ;
#7072 = SURFACE_STYLE_USAGE ( .BOTH. , #18150 ) ;
#7073 = VERTEX_POINT ( 'NONE', #7914 ) ;
#7074 = AXIS2_PLACEMENT_3D ( 'NONE', #3067, #27214, #19050 ) ;
#7075 = LINE ( 'NONE', #9239, #10341 ) ;
#7076 = EDGE_LOOP ( 'NONE', ( #4118, #718, #12932, #31672 ) ) ;
#7077 = ORIENTED_EDGE ( 'NONE', *, *, #23302, .F. ) ;
#7078 = CIRCLE ( 'NONE', #1409, 2.524999999999999467 ) ;
#7079 = AXIS2_PLACEMENT_3D ( 'NONE', #10524, #2674, #11228 ) ;
#7080 = DIRECTION ( 'NONE',  ( 0.000000000000000000, 0.000000000000000000, -1.000000000000000000 ) ) ;
#7081 = VERTEX_POINT ( 'NONE', #34803 ) ;
#7083 = VECTOR ( 'NONE', #19383, 1000.000000000000000 ) ;
#7082 = DIRECTION ( 'NONE',  ( 0.000000000000000000, 0.000000000000000000, 1.000000000000000000 ) ) ;
#7084 = DIRECTION ( 'NONE',  ( 0.000000000000000000, -1.000000000000000000, -2.465190328815662439E-32 ) ) ;
#7085 = DIRECTION ( 'NONE',  ( -0.000000000000000000, -1.836970198721029688E-16, 1.000000000000000000 ) ) ;
#7086 = DIRECTION ( 'NONE',  ( 1.000000000000000000, 0.000000000000000000, 0.000000000000000000 ) ) ;
#7087 = LINE ( 'NONE', #17807, #25118 ) ;
#7088 = EDGE_CURVE ( 'NONE', #33693, #9482, #7550, .T. ) ;
#7089 = VERTEX_POINT ( 'NONE', #10409 ) ;
#7090 = VECTOR ( 'NONE', #12302, 1000.000000000000000 ) ;
#7091 = VERTEX_POINT ( 'NONE', #21271 ) ;
#7092 = DIRECTION ( 'NONE',  ( -7.893605728314050488E-14, 1.618803117314786135E-15, 0.9999999999999998890 ) ) ;
#7093 = EDGE_CURVE ( 'NONE', #11385, #31447, #18617, .T. ) ;
#7094 = VERTEX_POINT ( 'NONE', #2392 ) ;
#7095 = VECTOR ( 'NONE', #2223, 1000.000000000000000 ) ;
#7096 = CARTESIAN_POINT ( 'NONE',  ( 0.000000000000000000, -44.99999999999993605, -85.22165320886810491 ) ) ;
#7097 = CARTESIAN_POINT ( 'NONE',  ( 8.000000000000000000, 0.000000000000000000, -11.22499999999999787 ) ) ;
#7098 = FACE_OUTER_BOUND ( 'NONE', #33930, .T. ) ;
#7099 = EDGE_CURVE ( 'NONE', #20342, #4500, #13269, .T. ) ;
#7100 = CONTEXT_DEPENDENT_SHAPE_REPRESENTATION ( #18554, #4341 ) ;
#7101 = AXIS2_PLACEMENT_3D ( 'NONE', #12422, #31616, #12586 ) ;
#7102 = ORIENTED_EDGE ( 'NONE', *, *, #4940, .T. ) ;
#7103 = FACE_OUTER_BOUND ( 'NONE', #32827, .T. ) ;
#7104 = DIRECTION ( 'NONE',  ( 0.000000000000000000, 0.9822872507286906085, -0.1873813145857145812 ) ) ;
#7105 = AXIS2_PLACEMENT_3D ( 'NONE', #25164, #8801, #27665 ) ;
#7106 = EDGE_CURVE ( 'NONE', #4812, #32414, #34986, .T. ) ;
#7108 = PLANE ( 'NONE',  #15268 ) ;
#7107 = CARTESIAN_POINT ( 'NONE',  ( -6.500000000000000000, 0.000000000000000000, 5.429999999999999716 ) ) ;
#7109 = ORIENTED_EDGE ( 'NONE', *, *, #21557, .T. ) ;
#7110 = EDGE_LOOP ( 'NONE', ( #14791, #1818 ) ) ;
#7111 = DIRECTION ( 'NONE',  ( 0.000000000000000000, 1.000000000000000000, 1.224646799147353207E-16 ) ) ;
#7112 = ORIENTED_EDGE ( 'NONE', *, *, #5379, .T. ) ;
#7113 = CARTESIAN_POINT ( 'NONE',  ( 2.261199756163084551, 20.68324032934681966, -26.21226347405724155 ) ) ;
#7114 = CARTESIAN_POINT ( 'NONE',  ( 2.789999999999999147, 23.28319895603611300, -21.86437915510192909 ) ) ;
#7115 = VERTEX_POINT ( 'NONE', #12749 ) ;
#7116 = VECTOR ( 'NONE', #25192, 1000.000000000000000 ) ;
#7117 = DIRECTION ( 'NONE',  ( -0.000000000000000000, 1.000000000000000000, -0.000000000000000000 ) ) ;
#7118 = ORIENTED_EDGE ( 'NONE', *, *, #24948, .F. ) ;
#7119 = VECTOR ( 'NONE', #18584, 1000.000000000000227 ) ;
#7120 = DIRECTION ( 'NONE',  ( 1.000000000000000000, 0.000000000000000000, 0.000000000000000000 ) ) ;
#7121 = DIRECTION ( 'NONE',  ( 1.000000000000000000, -0.000000000000000000, -0.000000000000000000 ) ) ;
#7122 = CARTESIAN_POINT ( 'NONE',  ( -27.84632068199329780, 25.66368763279036358, -36.68877005347593467 ) ) ;
#7124 = CYLINDRICAL_SURFACE ( 'NONE', #7131, 2.033421858999711951 ) ;
#7123 = CARTESIAN_POINT ( 'NONE',  ( 2.606461801040218074, 31.84255742294090652, 5.242117949250861386 ) ) ;
#7125 =( REPRESENTATION_RELATIONSHIP ('NONE','NONE', #23037, #15767 ) REPRESENTATION_RELATIONSHIP_WITH_TRANSFORMATION ( #11948 )SHAPE_REPRESENTATION_RELATIONSHIP( ) );
#7126 = CARTESIAN_POINT ( 'NONE',  ( -410.0000000000000568, -105.0000000000000142, -174.9999999999999432 ) ) ;
#7127 = DIRECTION ( 'NONE',  ( 0.000000000000000000, 1.836970198721029441E-16, -1.000000000000000000 ) ) ;
#7128 = B_SPLINE_CURVE_WITH_KNOTS ( 'NONE', 3,
 ( #20700, #23200, #33875, #28704, #4305, #34044 ),
 .UNSPECIFIED., .F., .F.,
 ( 4, 2, 4 ),
 ( 0.01435361776844886611, 0.01829828670248722505, 0.02224295563652558400 ),
 .UNSPECIFIED. ) ;
#7129 = CARTESIAN_POINT ( 'NONE',  ( 4.979875012683822710, -33.69708579775584667, 68.31122994652405112 ) ) ;
#7130 = LINE ( 'NONE', #18027, #28595 ) ;
#7131 = AXIS2_PLACEMENT_3D ( 'NONE', #18365, #12151, #34191 ) ;
#7132 = EDGE_LOOP ( 'NONE', ( #17614, #9652, #23679, #3538 ) ) ;
#7133 = VERTEX_POINT ( 'NONE', #32289 ) ;
#7134 = ORIENTED_EDGE ( 'NONE', *, *, #31070, .T. ) ;
#7135 = EDGE_CURVE ( 'NONE', #3925, #13528, #21619, .T. ) ;
#7136 = EDGE_CURVE ( 'NONE', #13528, #26514, #5225, .T. ) ;
#7137 = DIRECTION ( 'NONE',  ( 0.05413890858541753337, 0.9985334138511239299, 1.834276123671687566E-16 ) ) ;
#7138 = EDGE_CURVE ( 'NONE', #7094, #25411, #4298, .T. ) ;
#7139 = VERTEX_POINT ( 'NONE', #17009 ) ;
#7140 = VERTEX_POINT ( 'NONE', #785 ) ;
#7141 = ORIENTED_EDGE ( 'NONE', *, *, #22646, .T. ) ;
#7142 = LINE ( 'NONE', #26896, #23053 ) ;
#7143 = ORIENTED_EDGE ( 'NONE', *, *, #26142, .F. ) ;
#7144 = CARTESIAN_POINT ( 'NONE',  ( 0.000000000000000000, 3.524919873834583163E-15, 68.31122994652405112 ) ) ;
#7145 = DIRECTION ( 'NONE',  ( 0.000000000000000000, 0.000000000000000000, 1.000000000000000000 ) ) ;
#7146 = ORIENTED_EDGE ( 'NONE', *, *, #10323, .F. ) ;
#7147 = ORIENTED_EDGE ( 'NONE', *, *, #4740, .T. ) ;
#7148 = DIRECTION ( 'NONE',  ( 0.000000000000000000, 0.000000000000000000, 1.000000000000000000 ) ) ;
#7149 = CARTESIAN_POINT ( 'NONE',  ( -5.021133111224886036, 4.168562732279008642, -87.50000000000000000 ) ) ;
#7150 = CARTESIAN_POINT ( 'NONE',  ( -12.00000000000001066, -145.0000000000000000, 187.0000000000000000 ) ) ;
#7152 = EDGE_CURVE ( 'NONE', #20668, #9976, #14555, .T. ) ;
#7151 = CARTESIAN_POINT ( 'NONE',  ( -363.0000000000000000, -125.0000000000000284, 126.0000000000000000 ) ) ;
#7153 = LINE ( 'NONE', #34224, #19417 ) ;
#7154 = VERTEX_POINT ( 'NONE', #2743 ) ;
#7155 = CARTESIAN_POINT ( 'NONE',  ( -20.63749999999999574, 0.000000000000000000, 0.000000000000000000 ) ) ;
#7157 = AXIS2_PLACEMENT_3D ( 'NONE', #14719, #25903, #6676 ) ;
#7156 = CYLINDRICAL_SURFACE ( 'NONE', #27609, 2.500000000000002220 ) ;
#7158 = AXIS2_PLACEMENT_3D ( 'NONE', #29451, #28917, #2212 ) ;
#7159 = DIRECTION ( 'NONE',  ( 0.000000000000000000, 0.000000000000000000, 1.000000000000000000 ) ) ;
#7160 = EDGE_LOOP ( 'NONE', ( #34385, #13685 ) ) ;
#7161 = DIRECTION ( 'NONE',  ( 0.000000000000000000, 1.000000000000000000, 0.000000000000000000 ) ) ;
#7162 = EDGE_CURVE ( 'NONE', #20346, #2324, #24620, .T. ) ;
#7163 = CARTESIAN_POINT ( 'NONE',  ( -442.0000000000000000, -105.0000000000000142, 159.0000000000000000 ) ) ;
#7164 = LINE ( 'NONE', #26050, #26882 ) ;
#7166 = FACE_OUTER_BOUND ( 'NONE', #18705, .T. ) ;
#7165 = CYLINDRICAL_SURFACE ( 'NONE', #27539, 11.99999999999998934 ) ;
#7167 = EDGE_CURVE ( 'NONE', #29943, #2443, #8841, .T. ) ;
#7168 = CIRCLE ( 'NONE', #1521, 4.750000000000004441 ) ;
#7169 = CARTESIAN_POINT ( 'NONE',  ( 2.261199745677082262, 26.55216317045652730, -20.24504431679611116 ) ) ;
#7170 = VERTEX_POINT ( 'NONE', #22325 ) ;
#7171 = CARTESIAN_POINT ( 'NONE',  ( 100.4549654784875088, 3.507529710008591373, -11.99873639479134368 ) ) ;
#7173 = CARTESIAN_POINT ( 'NONE',  ( -499.9999999999999432, 112.9999999999999574, 162.9999999999999716 ) ) ;
#7172 = CARTESIAN_POINT ( 'NONE',  ( 18.63894936814906345, 26.67946662374789213, 68.31122994652405112 ) ) ;
#7174 = AXIS2_PLACEMENT_3D ( 'NONE', #16697, #9553, #28933 ) ;
#7175 = ADVANCED_FACE ( 'NONE', ( #11656 ), #22507, .F. ) ;
#7176 = ORIENTED_EDGE ( 'NONE', *, *, #22098, .T. ) ;
#7177 = DIRECTION ( 'NONE',  ( -1.000000000000000000, 0.000000000000000000, 0.000000000000000000 ) ) ;
#7178=STYLED_ITEM('',(#35254),#1117);
#7179 = VERTEX_POINT ( 'NONE', #24806 ) ;
#7180 = EDGE_CURVE ( 'NONE', #4182, #12655, #33354, .T. ) ;
#7181 = EDGE_CURVE ( 'NONE', #7314, #17657, #11470, .T. ) ;
#7182 = EDGE_LOOP ( 'NONE', ( #33208, #33502, #15644, #7955 ) ) ;
#7183 = CARTESIAN_POINT ( 'NONE',  ( 0.02407890056655825201, -17.95514392185434360, 25.38201125280350468 ) ) ;
#7184 = ORIENTED_EDGE ( 'NONE', *, *, #24341, .T. ) ;
#7185 = ORIENTED_EDGE ( 'NONE', *, *, #26292, .F. ) ;
#7186 = DIRECTION ( 'NONE',  ( 0.000000000000000000, 1.000000000000000000, 2.465190328815662439E-32 ) ) ;
#7187 = PRODUCT_DEFINITION_SHAPE ( 'NONE', 'NONE',  #35135 ) ;
#7188 = VECTOR ( 'NONE', #31512, 1000.000000000000000 ) ;
#7189 = VECTOR ( 'NONE', #23971, 1000.000000000000227 ) ;
#7190 = DIRECTION ( 'NONE',  ( -0.000000000000000000, 1.836970198721029934E-16, -1.000000000000000000 ) ) ;
#7191 = FACE_OUTER_BOUND ( 'NONE', #18202, .T. ) ;
#7192 = ORIENTED_EDGE ( 'NONE', *, *, #31346, .F. ) ;
#7193 = VERTEX_POINT ( 'NONE', #14330 ) ;
#7194 = DIRECTION ( 'NONE',  ( -0.2675283385292208105, -0.9635499925192230197, -1.770012621235684061E-16 ) ) ;
#7195 = DIRECTION ( 'NONE',  ( 0.000000000000000000, 0.000000000000000000, -1.000000000000000000 ) ) ;
#7196 = DIRECTION ( 'NONE',  ( -1.000000000000000000, 0.000000000000000000, 0.000000000000000000 ) ) ;
#7197 = PLANE ( 'NONE',  #30658 ) ;
#7198 = CARTESIAN_POINT ( 'NONE',  ( 0.02407890056655738464, -27.96208973699912548, 13.59246946040177129 ) ) ;
#7199 = VERTEX_POINT ( 'NONE', #27130 ) ;
#7200 = EDGE_LOOP ( 'NONE', ( #20587, #27812, #31721, #12380 ) ) ;
#7201 = LINE ( 'NONE', #4358, #12269 ) ;
#7202 = CARTESIAN_POINT ( 'NONE',  ( 21.85761591200894216, 30.91355005303805825, 68.31122994652405112 ) ) ;
#7203 = VERTEX_POINT ( 'NONE', #13612 ) ;
#7204 = VECTOR ( 'NONE', #15036, 1000.000000000000000 ) ;
#7205 = CARTESIAN_POINT ( 'NONE',  ( -5.527271473480783293, -1.747512292859696226, 5.429999999999999716 ) ) ;
#7206 = CARTESIAN_POINT ( 'NONE',  ( 2.783128773493238395, -7.987145637396467990, 29.81833655972095087 ) ) ;
#7207 = EDGE_CURVE ( 'NONE', #29809, #21836, #24442, .T. ) ;
#7208 = DIRECTION ( 'NONE',  ( 0.000000000000000000, 0.000000000000000000, -1.000000000000000000 ) ) ;
#7209 = EDGE_LOOP ( 'NONE', ( #3298, #12875, #26189, #1422 ) ) ;
#7210 = EDGE_CURVE ( 'NONE', #15103, #28398, #19314, .T. ) ;
#7211 = FACE_OUTER_BOUND ( 'NONE', #11152, .T. ) ;
#7212 = ORIENTED_EDGE ( 'NONE', *, *, #18421, .F. ) ;
#7214 = CARTESIAN_POINT ( 'NONE',  ( 1.394999999999999574, -18.21166265554768415, -29.20140402659759715 ) ) ;
#7213 = CARTESIAN_POINT ( 'NONE',  ( 10.17231796313411429, 13.56412600238610366, -87.50000000000000000 ) ) ;
#7215 = CARTESIAN_POINT ( 'NONE',  ( -110.1150203881707910, 0.3368795255050305859, 12.50000000000000178 ) ) ;
#7216 = AXIS2_PLACEMENT_3D ( 'NONE', #8707, #20109, #33974 ) ;
#7217 = AXIS2_PLACEMENT_3D ( 'NONE', #12613, #15822, #23637 ) ;
#7218 = AXIS2_PLACEMENT_3D ( 'NONE', #29382, #31850, #23683 ) ;
#7219 = ORIENTED_EDGE ( 'NONE', *, *, #2504, .T. ) ;
#7220 = CYLINDRICAL_SURFACE ( 'NONE', #13760, 7.999999999999979572 ) ;
#7221 = EDGE_CURVE ( 'NONE', #22677, #11706, #13973, .T. ) ;
#7222 = LINE ( 'NONE', #31272, #316 ) ;
#7223 = ORIENTED_EDGE ( 'NONE', *, *, #12244, .T. ) ;
#7224 = AXIS2_PLACEMENT_3D ( 'NONE', #33026, #25374, #27868 ) ;
#7225 = DIRECTION ( 'NONE',  ( -7.893605728314051750E-14, 1.618803117314786530E-15, 1.000000000000000000 ) ) ;
#7226 = ORIENTED_EDGE ( 'NONE', *, *, #28366, .T. ) ;
#7227 = CARTESIAN_POINT ( 'NONE',  ( -500.0000000000000000, -145.0000000000000000, 162.9999999999999716 ) ) ;
#7228 = ORIENTED_EDGE ( 'NONE', *, *, #14075, .F. ) ;
#7229 = CARTESIAN_POINT ( 'NONE',  ( -499.9999999999999432, 112.9999999999999574, -162.9999999999999716 ) ) ;
#7230 = CARTESIAN_POINT ( 'NONE',  ( -1.030735741678193484, 1.713938105891546826, 0.000000000000000000 ) ) ;
#7231 = CIRCLE ( 'NONE', #33955, 2.033421858999711507 ) ;
#7232 = CARTESIAN_POINT ( 'NONE',  ( -110.1150203881707910, 3.829664765295703645E-16, -7.500000000000000000 ) ) ;
#7233 = LINE ( 'NONE', #4732, #25032 ) ;
#7234 = ORIENTED_EDGE ( 'NONE', *, *, #15256, .F. ) ;
#7235 = ORIENTED_EDGE ( 'NONE', *, *, #21337, .F. ) ;
#7236 = VERTEX_POINT ( 'NONE', #10941 ) ;
#7237 = PRODUCT_DEFINITION_SHAPE ( 'NONE', 'NONE',  #35125 ) ;
#7238 = EDGE_CURVE ( 'NONE', #29888, #25980, #21788, .T. ) ;
#7239 = DIRECTION ( 'NONE',  ( -1.000000000000000000, -0.000000000000000000, -0.000000000000000000 ) ) ;
#7240 = DIRECTION ( 'NONE',  ( 0.000000000000000000, 1.836970198721029441E-16, -1.000000000000000000 ) ) ;
#7241 = VECTOR ( 'NONE', #13229, 1000.000000000000000 ) ;
#7242 = FACE_OUTER_BOUND ( 'NONE', #30227, .T. ) ;
#7243 = DIRECTION ( 'NONE',  ( 1.000000000000000000, 0.000000000000000000, 0.000000000000000000 ) ) ;
#7244 = CARTESIAN_POINT ( 'NONE',  ( 0.006871144406695839368, -27.79352918700758934, 13.43306967213398906 ) ) ;
#7245 = CARTESIAN_POINT ( 'NONE',  ( 11.99999999999999645, 124.9999999999999716, 187.0000000000000000 ) ) ;
#7246 = VERTEX_POINT ( 'NONE', #5577 ) ;
#7247 = EDGE_CURVE ( 'NONE', #890, #11445, #8264, .T. ) ;
#7248 = CARTESIAN_POINT ( 'NONE',  ( 14.70109753509668948, 34.88954974633765005, 68.31122994652405112 ) ) ;
#7249 = DIRECTION ( 'NONE',  ( 0.000000000000000000, -1.131431318426415506E-52, -1.000000000000000000 ) ) ;
#7250 = VECTOR ( 'NONE', #961, 1000.000000000000000 ) ;
#7251 = EDGE_CURVE ( 'NONE', #1893, #33296, #16473, .T. ) ;
#7252 = DIRECTION ( 'NONE',  ( 0.000000000000000000, 7.888609052210118054E-31, 1.000000000000000000 ) ) ;
#7253 = VERTEX_POINT ( 'NONE', #24977 ) ;
#7254 = EDGE_CURVE ( 'NONE', #17151, #23603, #261, .T. ) ;
#7255 = DIRECTION ( 'NONE',  ( 0.000000000000000000, 0.000000000000000000, 1.000000000000000000 ) ) ;
#7256 = VERTEX_POINT ( 'NONE', #19144 ) ;
#7257 = DIRECTION ( 'NONE',  ( 1.000000000000000000, 3.040835319149746090E-31, 1.232595164407830946E-32 ) ) ;
#7258 = CARTESIAN_POINT ( 'NONE',  ( 0.1859802529459479992, -16.26694784591012777, -27.88362116434760551 ) ) ;
#7259 = AXIS2_PLACEMENT_3D ( 'NONE', #32972, #13780, #32805 ) ;
#7260 = CARTESIAN_POINT ( 'NONE',  ( 50.00050000000000239, 0.000000000000000000, 3.000000000000000000 ) ) ;
#7261 = CARTESIAN_POINT ( 'NONE',  ( 2.765921099433441110, 14.63235270440936731, 27.43224275967444470 ) ) ;
#7262 = DIRECTION ( 'NONE',  ( -1.000000000000000000, 0.000000000000000000, 0.000000000000000000 ) ) ;
#7263 = ORIENTED_EDGE ( 'NONE', *, *, #8238, .F. ) ;
#7264 = AXIS2_PLACEMENT_3D ( 'NONE', #26871, #10328, #24372 ) ;
#7265 = ORIENTED_EDGE ( 'NONE', *, *, #17058, .T. ) ;
#7266 = CARTESIAN_POINT ( 'NONE',  ( 780.8966796602292106, 1113.547194656238389, 1753.598338701303192 ) ) ;
#7267 = VERTEX_POINT ( 'NONE', #30516 ) ;
#7268 = CIRCLE ( 'NONE', #10708, 10.00000000000000000 ) ;
#7269 = CARTESIAN_POINT ( 'NONE',  ( -18.45373714011839539, 26.80790850550480897, 68.31122994652405112 ) ) ;
#7270 = FACE_OUTER_BOUND ( 'NONE', #17750, .T. ) ;
#7271 = CARTESIAN_POINT ( 'NONE',  ( 99.46260833598724105, -1.553728400065965687, 7.347407880389961399 ) ) ;
#7272 = CONTEXT_DEPENDENT_SHAPE_REPRESENTATION ( #22166, #34246 ) ;
#7273 = ORIENTED_EDGE ( 'NONE', *, *, #20238, .F. ) ;
#7274 = CARTESIAN_POINT ( 'NONE',  ( -9.978866888775426602, 18.16264470403145026, -67.50000000000000000 ) ) ;
#7276 = CARTESIAN_POINT ( 'NONE',  ( 15.04122381213380244, 28.86114964982165887, 68.31122994652405112 ) ) ;
#7275 = DIRECTION ( 'NONE',  ( 0.05413890858541543089, 0.9985334138511240409, 0.000000000000000000 ) ) ;
#7277 = AXIS2_PLACEMENT_3D ( 'NONE', #18909, #16247, #27079 ) ;
#7278 = ORIENTED_EDGE ( 'NONE', *, *, #27033, .T. ) ;
#7279 = ORIENTED_EDGE ( 'NONE', *, *, #426, .F. ) ;
#7280 = CARTESIAN_POINT ( 'NONE',  ( 0.02407890056655608360, 4.286445725888036407, 30.79383171238946204 ) ) ;
#7281 = EDGE_CURVE ( 'NONE', #23878, #9326, #23633, .T. ) ;
#7282 = VERTEX_POINT ( 'NONE', #21974 ) ;
#7283 = EDGE_CURVE ( 'NONE', #12207, #32312, #8441, .T. ) ;
#7284 = CARTESIAN_POINT ( 'NONE',  ( -355.0000000000000000, 130.9999999999999716, 109.9999999999999858 ) ) ;
#7285 = DIRECTION ( 'NONE',  ( 0.000000000000000000, 0.000000000000000000, -1.000000000000000000 ) ) ;
#7286 = EDGE_LOOP ( 'NONE', ( #35031, #34623, #13433, #34456 ) ) ;
#7287 = AXIS2_PLACEMENT_3D ( 'NONE', #3864, #24875, #14406 ) ;
#7288 = LINE ( 'NONE', #13015, #17481 ) ;
#7289 = EDGE_CURVE ( 'NONE', #28866, #33527, #20194, .T. ) ;
#7290 = PRODUCT_DEFINITION_SHAPE ( 'NONE', 'NONE',  #35229 ) ;
#7291 = ORIENTED_EDGE ( 'NONE', *, *, #7902, .F. ) ;
#7292 = EDGE_CURVE ( 'NONE', #9877, #7307, #18547, .T. ) ;
#7293 = LINE ( 'NONE', #7467, #28304 ) ;
#7294 = FACE_OUTER_BOUND ( 'NONE', #20368, .T. ) ;
#7295 = CARTESIAN_POINT ( 'NONE',  ( 11.99999999999999645, -145.0000000000000000, -186.9999999999999716 ) ) ;
#7296 = AXIS2_PLACEMENT_3D ( 'NONE', #16518, #13836, #24669 ) ;
#7298 = CARTESIAN_POINT ( 'NONE',  ( -21.41424479178918361, -24.50784553716280101, 68.31122994652405112 ) ) ;
#7297 = CARTESIAN_POINT ( 'NONE',  ( 9.199999999999999289, 13.50000000000000178, 0.000000000000000000 ) ) ;
#7299 = DIRECTION ( 'NONE',  ( 0.000000000000000000, -1.000000000000000000, 0.000000000000000000 ) ) ;
#7300 = CARTESIAN_POINT ( 'NONE',  ( 0.1149164202474758090, 13.01099471650157824, -4.464296094009046811 ) ) ;
#7301 = CARTESIAN_POINT ( 'NONE',  ( -130.6469666100234406, 6.000000000000000000, -57.49999999999999289 ) ) ;
#7302 = DIRECTION ( 'NONE',  ( 0.000000000000000000, 3.374343856708137958E-53, -1.000000000000000000 ) ) ;
#7303 = EDGE_CURVE ( 'NONE', #18637, #2425, #31044, .T. ) ;
#7304 = VECTOR ( 'NONE', #11879, 1000.000000000000000 ) ;
#7305 = EDGE_LOOP ( 'NONE', ( #26522, #4521, #22234, #31960 ) ) ;
#7306 =( NAMED_UNIT ( * ) SI_UNIT ( $, .STERADIAN. ) SOLID_ANGLE_UNIT ( ) );
#7307 = VERTEX_POINT ( 'NONE', #20530 ) ;
#7308 = ORIENTED_EDGE ( 'NONE', *, *, #25454, .T. ) ;
#7309 = AXIS2_PLACEMENT_3D ( 'NONE', #18480, #34656, #113 ) ;
#7310 = PLANE ( 'NONE',  #30127 ) ;
#7311 = DIRECTION ( 'NONE',  ( 0.1063910735369155841, -0.9943243633099125844, -3.335902418025060287E-15 ) ) ;
#7312 = VERTEX_POINT ( 'NONE', #23369 ) ;
#7313 = VERTEX_POINT ( 'NONE', #17881 ) ;
#7314 = VERTEX_POINT ( 'NONE', #8975 ) ;
#7315 = B_SPLINE_CURVE_WITH_KNOTS ( 'NONE', 3,
 ( #29229, #16385, #13870, #24710 ),
 .UNSPECIFIED., .F., .F.,
 ( 4, 4 ),
 ( 0.005298349227682424070, 0.005985217865144619280 ),
 .UNSPECIFIED. ) ;
#7316 = CARTESIAN_POINT ( 'NONE',  ( -418.0000000000000000, -141.0000000000000000, -155.0000000000000000 ) ) ;
#7317 = VECTOR ( 'NONE', #19315, 1000.000000000000000 ) ;
#7318 = ORIENTED_EDGE ( 'NONE', *, *, #16987, .F. ) ;
#7319 = CARTESIAN_POINT ( 'NONE',  ( 2.765921099433443331, 14.63235270440974922, -27.43224275967423509 ) ) ;
#7320 = DIRECTION ( 'NONE',  ( 0.000000000000000000, 1.310824597558155437E-49, 1.000000000000000000 ) ) ;
#7321 = ORIENTED_EDGE ( 'NONE', *, *, #15287, .T. ) ;
#7322 = VERTEX_POINT ( 'NONE', #1317 ) ;
#7323 = DIRECTION ( 'NONE',  ( -0.7621620551276362399, -0.6473862847818278032, 0.000000000000000000 ) ) ;
#7324 = DIRECTION ( 'NONE',  ( 0.000000000000000000, 0.000000000000000000, 1.000000000000000000 ) ) ;
#7325 = DIRECTION ( 'NONE',  ( 0.000000000000000000, 0.000000000000000000, 1.000000000000000000 ) ) ;
#7326 = PLANE ( 'NONE',  #619 ) ;
#7327 = CARTESIAN_POINT ( 'NONE',  ( 29.44023756548695658, 13.87360028845404969, 49.43553178847298568 ) ) ;
#7328 = EDGE_LOOP ( 'NONE', ( #27246, #4750, #25702, #12958 ) ) ;
#7329 = CARTESIAN_POINT ( 'NONE',  ( 145.0000000000000568, -85.49999999999998579, 65.00000000000000000 ) ) ;
#7330 = CARTESIAN_POINT ( 'NONE',  ( -499.9999999999999432, -141.0000000000000000, -162.9999999999999716 ) ) ;
#7331 = CIRCLE ( 'NONE', #10199, 3.999999999999976019 ) ;
#7332 = VERTEX_POINT ( 'NONE', #6814 ) ;
#7333 = EDGE_CURVE ( 'NONE', #25265, #29943, #23209, .T. ) ;
#7334 = DIRECTION ( 'NONE',  ( 0.000000000000000000, 0.000000000000000000, 1.000000000000000000 ) ) ;
#7335 = LINE ( 'NONE', #31390, #4149 ) ;
#7336 = EDGE_CURVE ( 'NONE', #1054, #28789, #25689, .T. ) ;
#7337 = CARTESIAN_POINT ( 'NONE',  ( 108.7790296513208119, 4.332787265952012135, -6.129206022554251732 ) ) ;
#7339 = DIRECTION ( 'NONE',  ( 0.000000000000000000, 0.000000000000000000, 1.000000000000000000 ) ) ;
#7338 = CARTESIAN_POINT ( 'NONE',  ( -418.0000000000000000, 105.0000000000000000, -77.99999999999997158 ) ) ;
#7340 = EDGE_CURVE ( 'NONE', #20827, #28866, #33525, .T. ) ;
#7341 = ADVANCED_FACE ( 'NONE', ( #25335 ), #20366, .T. ) ;
#7342 = CARTESIAN_POINT ( 'NONE',  ( -445.9999999999999432, -112.9999999999999858, 155.0000000000000000 ) ) ;
#7343 = ORIENTED_EDGE ( 'NONE', *, *, #27360, .F. ) ;
#7344 = CARTESIAN_POINT ( 'NONE',  ( 108.7969789446760132, 4.317991217963451867, -11.73376546078468508 ) ) ;
#7346 = CARTESIAN_POINT ( 'NONE',  ( 0.000000000000000000, 0.000000000000000000, 4.679999999999999716 ) ) ;
#7345 =( NAMED_UNIT ( * ) PLANE_ANGLE_UNIT ( ) SI_UNIT ( $, .RADIAN. ) );
#7347 = AXIS2_PLACEMENT_3D ( 'NONE', #1659, #18062, #20532 ) ;
#7348 = ORIENTED_EDGE ( 'NONE', *, *, #28057, .F. ) ;
#7349 = CARTESIAN_POINT ( 'NONE',  ( -500.0000000000000000, -141.0000000000000000, 187.0000000000000000 ) ) ;
#7350 = ORIENTED_EDGE ( 'NONE', *, *, #26356, .T. ) ;
#7351 = EDGE_CURVE ( 'NONE', #8689, #22441, #26042, .T. ) ;
#7352 = CIRCLE ( 'NONE', #34667, 3.999999999999976019 ) ;
#7353 = ORIENTED_EDGE ( 'NONE', *, *, #6576, .T. ) ;
#7354 = LINE ( 'NONE', #20556, #317 ) ;
#7355 = ORIENTED_EDGE ( 'NONE', *, *, #18035, .T. ) ;
#7356 = ORIENTED_EDGE ( 'NONE', *, *, #2612, .F. ) ;
#7357 = CARTESIAN_POINT ( 'NONE',  ( -9.978866888775426602, 16.12922284503174097, -87.50000000000000000 ) ) ;
#7358 = EDGE_CURVE ( 'NONE', #24110, #5728, #34051, .T. ) ;
#7360 = ADVANCED_FACE ( 'NONE', ( #6989 ), #2028, .T. ) ;
#7359 = CARTESIAN_POINT ( 'NONE',  ( 11.99999999999999645, 144.9999999999999147, 187.0000000000000000 ) ) ;
#7361 = CARTESIAN_POINT ( 'NONE',  ( 2.783107584500409626, 4.187058600949539411, 30.58452291340892160 ) ) ;
#7362 = ORIENTED_EDGE ( 'NONE', *, *, #31569, .F. ) ;
#7363 = VERTEX_POINT ( 'NONE', #17705 ) ;
#7364 = LINE ( 'NONE', #15067, #28731 ) ;
#7365 = DIRECTION ( 'NONE',  ( 0.000000000000000000, 0.000000000000000000, -1.000000000000000000 ) ) ;
#7366 = B_SPLINE_CURVE_WITH_KNOTS ( 'NONE', 3,
 ( #1785, #14985, #23499, #25821 ),
 .UNSPECIFIED., .F., .F.,
 ( 4, 4 ),
 ( 0.005298355823470651295, 0.005985224365431043858 ),
 .UNSPECIFIED. ) ;
#7367 = DIRECTION ( 'NONE',  ( -0.9941379571543595972, -0.1081190184239421009, -1.986114147597516136E-17 ) ) ;
#7368 = LINE ( 'NONE', #34983, #4484 ) ;
#7369 = DIRECTION ( 'NONE',  ( -0.000000000000000000, 6.123233995736766036E-17, 1.000000000000000000 ) ) ;
#7370 = UNCERTAINTY_MEASURE_WITH_UNIT (LENGTH_MEASURE( 1.000000000000000082E-05 ), #24179, 'distance_accuracy_value', 'NONE');
#7371 = VERTEX_POINT ( 'NONE', #9141 ) ;
#7372 = AXIS2_PLACEMENT_3D ( 'NONE', #28999, #26327, #31830 ) ;
#7373 = VERTEX_POINT ( 'NONE', #31381 ) ;
#7374 = CYLINDRICAL_SURFACE ( 'NONE', #20762, 2.524999999999999467 ) ;
#7375 = LINE ( 'NONE', #4006, #22129 ) ;
#7376 = EDGE_LOOP ( 'NONE', ( #1810, #22306, #18745, #25043, #23903, #8065, #28326, #17589, #14965, #10425, #18910 ) ) ;
#7377 = LINE ( 'NONE', #2571, #6618 ) ;
#7378 = DIRECTION ( 'NONE',  ( 0.000000000000000000, -1.310824597558155437E-49, -1.000000000000000000 ) ) ;
#7379 = DIRECTION ( 'NONE',  ( -0.000000000000000000, 1.836970198721029934E-16, -1.000000000000000000 ) ) ;
#7380 = ORIENTED_EDGE ( 'NONE', *, *, #2637, .F. ) ;
#7381 = LINE ( 'NONE', #21281, #14942 ) ;
#7382 = ORIENTED_EDGE ( 'NONE', *, *, #28651, .T. ) ;
#7383 = EDGE_CURVE ( 'NONE', #12838, #3029, #3964, .T. ) ;
#7384 = ADVANCED_FACE ( 'NONE', ( #15199 ), #1657, .T. ) ;
#7385 =( REPRESENTATION_RELATIONSHIP ('NONE','NONE', #23037, #28231 ) REPRESENTATION_RELATIONSHIP_WITH_TRANSFORMATION ( #32060 )SHAPE_REPRESENTATION_RELATIONSHIP( ) );
#7386 = FACE_OUTER_BOUND ( 'NONE', #4502, .T. ) ;
#7387 = ORIENTED_EDGE ( 'NONE', *, *, #29134, .T. ) ;
#7389 = CARTESIAN_POINT ( 'NONE',  ( -499.9999999999999432, 136.9999999999999432, -155.0000000000000000 ) ) ;
#7388 = DIRECTION ( 'NONE',  ( 1.000000000000000000, 3.040835319149746528E-31, 1.232595164407830946E-32 ) ) ;
#7390 = CARTESIAN_POINT ( 'NONE',  ( -5.210000000000000853, 0.000000000000000000, 0.000000000000000000 ) ) ;
#7391 = ADVANCED_FACE ( 'NONE', ( #14688 ), #1488, .F. ) ;
#7392 = EDGE_LOOP ( 'NONE', ( #25845, #13798, #23914, #3380 ) ) ;
#7393 = DIRECTION ( 'NONE',  ( 0.000000000000000000, 0.000000000000000000, -1.000000000000000000 ) ) ;
#7394 = CARTESIAN_POINT ( 'NONE',  ( -6.637260778198712075, 37.28255902965928215, 68.31122994652405112 ) ) ;
#7395 = VERTEX_POINT ( 'NONE', #12525 ) ;
#7396 = DIRECTION ( 'NONE',  ( -6.336005985659138209E-14, 3.792805845712701427E-14, 1.000000000000000000 ) ) ;
#7397 = ORIENTED_EDGE ( 'NONE', *, *, #23510, .T. ) ;
#7398 = CARTESIAN_POINT ( 'NONE',  ( 100.3426091166337812, -3.356891575080633849, 12.04186941445821724 ) ) ;
#7399 = ORIENTED_EDGE ( 'NONE', *, *, #15315, .F. ) ;
#7400 = CARTESIAN_POINT ( 'NONE',  ( -19.99999999999998934, -137.0000000000000000, 187.0000000000000000 ) ) ;
#7401 = EDGE_CURVE ( 'NONE', #17794, #35009, #30688, .T. ) ;
#7402 = DIRECTION ( 'NONE',  ( -0.000000000000000000, -1.000000000000000000, -0.000000000000000000 ) ) ;
#7403 = ADVANCED_FACE ( 'NONE', ( #17180 ), #17363, .T. ) ;
#7404 = CARTESIAN_POINT ( 'NONE',  ( 0.000000000000000000, 0.000000000000000000, -0.7500000000000000000 ) ) ;
#7405 = CIRCLE ( 'NONE', #21064, 34.41491905851385269 ) ;
#7406 = DIRECTION ( 'NONE',  ( -0.000000000000000000, 0.000000000000000000, -1.000000000000000000 ) ) ;
#7407 = CONTEXT_DEPENDENT_SHAPE_REPRESENTATION ( #803, #942 ) ;
#7408 = ORIENTED_EDGE ( 'NONE', *, *, #3088, .T. ) ;
#7409 = ORIENTED_EDGE ( 'NONE', *, *, #12105, .T. ) ;
#7410 = ORIENTED_EDGE ( 'NONE', *, *, #22989, .T. ) ;
#7411 = LINE ( 'NONE', #31462, #16946 ) ;
#7412 = ADVANCED_FACE ( 'NONE', ( #2526 ), #18400, .F. ) ;
#7413 = DIRECTION ( 'NONE',  ( -0.000000000000000000, 1.836970198721029934E-16, -1.000000000000000000 ) ) ;
#7415 = EDGE_CURVE ( 'NONE', #24798, #12655, #16079, .T. ) ;
#7414 = LINE ( 'NONE', #10810, #3675 ) ;
#7416 = DIRECTION ( 'NONE',  ( -0.1378075576670459157, 0.8405889147755769564, -0.5238505067347569710 ) ) ;
#7417 = DIRECTION ( 'NONE',  ( 0.000000000000000000, -0.000000000000000000, -1.000000000000000000 ) ) ;
#7418 = CARTESIAN_POINT ( 'NONE',  ( -365.0000000000000000, -131.0000000000000000, 113.9999999999999858 ) ) ;
#7419 = ORIENTED_EDGE ( 'NONE', *, *, #5701, .F. ) ;
#7420 = EDGE_CURVE ( 'NONE', #31947, #23009, #8278, .T. ) ;
#7421 = AXIS2_PLACEMENT_3D ( 'NONE', #10407, #5574, #27127 ) ;
#7422 = CARTESIAN_POINT ( 'NONE',  ( -35.55956070192387841, -32.65143121711728469, 5.690671783530174999 ) ) ;
#7423 = CARTESIAN_POINT ( 'NONE',  ( 1.040000000000002034, 28.00026196654299326, -20.00929742917092824 ) ) ;
#7424 = CARTESIAN_POINT ( 'NONE',  ( -349.0000000000000000, -125.0000000000000284, 113.9999999999999858 ) ) ;
#7425 = ORIENTED_EDGE ( 'NONE', *, *, #25479, .F. ) ;
#7426 = DIRECTION ( 'NONE',  ( -1.000000000000000000, 0.000000000000000000, -0.000000000000000000 ) ) ;
#7427 = ORIENTED_EDGE ( 'NONE', *, *, #13712, .F. ) ;
#7428 = DIRECTION ( 'NONE',  ( -1.000000000000000000, 0.000000000000000000, 0.000000000000000000 ) ) ;
#7429 = CARTESIAN_POINT ( 'NONE',  ( 0.000000000000000000, -17.83604598421681331, 24.70480026434162113 ) ) ;
#7431 = VERTEX_POINT ( 'NONE', #31554 ) ;
#7430 = VECTOR ( 'NONE', #17700, 1000.000000000000000 ) ;
#7432 = CIRCLE ( 'NONE', #22299, 30.47050528711511674 ) ;
#7433 = FACE_OUTER_BOUND ( 'NONE', #20297, .T. ) ;
#7434 = VECTOR ( 'NONE', #26794, 1000.000000000000227 ) ;
#7435 = FACE_OUTER_BOUND ( 'NONE', #5655, .T. ) ;
#7436 = DIRECTION ( 'NONE',  ( 1.000000000000000000, 3.040835319149746090E-31, 1.232595164407830946E-32 ) ) ;
#7437 = EDGE_LOOP ( 'NONE', ( #14980, #5588, #13560, #14411 ) ) ;
#7438 = EDGE_LOOP ( 'NONE', ( #13903, #20764, #6198, #1824 ) ) ;
#7439 = DIRECTION ( 'NONE',  ( -0.1063910735369017202, 0.9943243633099136947, -1.000770725407181676E-14 ) ) ;
#7440 = VECTOR ( 'NONE', #9138, 1000.000000000000000 ) ;
#7441 = VERTEX_POINT ( 'NONE', #18754 ) ;
#7442 = CIRCLE ( 'NONE', #18860, 13.49999999999999822 ) ;
#7443 = ADVANCED_FACE ( 'NONE', ( #29590 ), #7156, .T. ) ;
#7444 = CARTESIAN_POINT ( 'NONE',  ( 20.73027531293552528, -10.15143121711728469, 20.00000000000000000 ) ) ;
#7445 = EDGE_CURVE ( 'NONE', #1337, #23936, #18061, .T. ) ;
#7446 = DIRECTION ( 'NONE',  ( 1.000000000000000000, 0.000000000000000000, 0.000000000000000000 ) ) ;
#7447 = CARTESIAN_POINT ( 'NONE',  ( 104.8054821786513884, -5.738162003225207641, 4.829440634198706839 ) ) ;
#7448 = ITEM_DEFINED_TRANSFORMATION ( 'NONE', 'NONE', #16663,  #28566 ) ;
#7449 = EDGE_LOOP ( 'NONE', ( #17810, #27063, #6835, #31042 ) ) ;
#7450 = CARTESIAN_POINT ( 'NONE',  ( 1.532562817202168137, 32.50931595846690669, 49.43553178847298568 ) ) ;
#7452 = CARTESIAN_POINT ( 'NONE',  ( 2.033800774785157195, -2.658747979797710936, 33.81079988514328249 ) ) ;
#7451 = DIRECTION ( 'NONE',  ( 0.000000000000000000, 0.000000000000000000, 1.000000000000000000 ) ) ;
#7454 = ORIENTED_EDGE ( 'NONE', *, *, #635, .F. ) ;
#7453 = CIRCLE ( 'NONE', #19405, 30.47050528711511674 ) ;
#7455 = ORIENTED_EDGE ( 'NONE', *, *, #10276, .T. ) ;
#7456 = DIRECTION ( 'NONE',  ( 0.000000000000000000, 0.000000000000000000, -1.000000000000000000 ) ) ;
#7457 = CIRCLE ( 'NONE', #5170, 7.500000000000000000 ) ;
#7458 = ORIENTED_EDGE ( 'NONE', *, *, #33947, .T. ) ;
#7459 = AXIS2_PLACEMENT_3D ( 'NONE', #24460, #15967, #13458 ) ;
#7460 = VECTOR ( 'NONE', #9805, 1000.000000000000000 ) ;
#7461 = DIRECTION ( 'NONE',  ( 1.000000000000000000, 0.000000000000000000, -0.000000000000000000 ) ) ;
#7462 = CARTESIAN_POINT ( 'NONE',  ( 19.99999999999998224, 134.9999999999999432, -162.9999999999999432 ) ) ;
#7463 = ORIENTED_EDGE ( 'NONE', *, *, #11954, .F. ) ;
#7464 = LINE ( 'NONE', #21009, #33348 ) ;
#7465 = ORIENTED_EDGE ( 'NONE', *, *, #12666, .T. ) ;
#7466 = B_SPLINE_CURVE_WITH_KNOTS ( 'NONE', 3,
 ( #1159, #33725, #20214, #35092 ),
 .UNSPECIFIED., .F., .F.,
 ( 4, 4 ),
 ( 2.128468106753875164E-07, 0.0006879486673519094857 ),
 .UNSPECIFIED. ) ;
#7467 = CARTESIAN_POINT ( 'NONE',  ( -19.99999999999998934, 144.9999999999999716, 162.9999999999999716 ) ) ;
#7468 = CARTESIAN_POINT ( 'NONE',  ( 0.000000000000000000, 1.974842713994612024E-15, 76.74945698428001606 ) ) ;
#7469 = CIRCLE ( 'NONE', #6891, 7.999999999999986677 ) ;
#7470 = CARTESIAN_POINT ( 'NONE',  ( 28.23027531293552528, -17.65143121711728469, 20.00000000000000000 ) ) ;
#7472 = DIRECTION ( 'NONE',  ( 0.000000000000000000, 0.000000000000000000, 1.000000000000000000 ) ) ;
#7471 = CARTESIAN_POINT ( 'NONE',  ( 0.07094833857658310039, -31.66307346108432341, -1.400387680934324308 ) ) ;
#7473 = CARTESIAN_POINT ( 'NONE',  ( 0.000000000000000000, 0.000000000000000000, 10.00000000000000000 ) ) ;
#7474 = CARTESIAN_POINT ( 'NONE',  ( 12.00000000000001066, -60.99999999999997158, -175.0000000000000000 ) ) ;
#7475 = CARTESIAN_POINT ( 'NONE',  ( 0.07098929236673945375, -8.452877438714468283, 30.54658108095609848 ) ) ;
#7476 = DIRECTION ( 'NONE',  ( 1.000000000000000000, 0.000000000000000000, 1.300283923313630633E-47 ) ) ;
#7477 = PRODUCT_DEFINITION_SHAPE ( 'NONE', 'NONE',  #35184 ) ;
#7478 = VECTOR ( 'NONE', #7436, 1000.000000000000000 ) ;
#7479 = ORIENTED_EDGE ( 'NONE', *, *, #20683, .F. ) ;
#7480 = AXIS2_PLACEMENT_3D ( 'NONE', #28760, #26258, #2058 ) ;
#7481 = CARTESIAN_POINT ( 'NONE',  ( 787.0597240610728704, 1342.348721680644985, 1756.388338701304974 ) ) ;
#7482 = CIRCLE ( 'NONE', #9209, 3.999999999999976019 ) ;
#7483 = AXIS2_PLACEMENT_3D ( 'NONE', #6387, #33625, #9249 ) ;
#7484 = ORIENTED_EDGE ( 'NONE', *, *, #4288, .T. ) ;
#7485 = ORIENTED_EDGE ( 'NONE', *, *, #1589, .F. ) ;
#7486 = EDGE_CURVE ( 'NONE', #14225, #26110, #34758, .T. ) ;
#7487 = EDGE_CURVE ( 'NONE', #12045, #11373, #29420, .T. ) ;
#7488 = DIRECTION ( 'NONE',  ( 0.000000000000000000, 0.000000000000000000, -1.000000000000000000 ) ) ;
#7489 = PRODUCT_CONTEXT ( 'NONE', #5985, 'mechanical' ) ;
#7490 = ORIENTED_EDGE ( 'NONE', *, *, #31834, .T. ) ;
#7491 = EDGE_LOOP ( 'NONE', ( #19669, #17057, #15453, #12771 ) ) ;
#7492 = ORIENTED_EDGE ( 'NONE', *, *, #32135, .F. ) ;
#7493 = ADVANCED_FACE ( 'NONE', ( #32072 ), #34583, .T. ) ;
#7494 = LINE ( 'NONE', #7316, #29295 ) ;
#7495 = CARTESIAN_POINT ( 'NONE',  ( -500.0000000000000000, -104.9999999999999858, -162.9999999999999716 ) ) ;
#7496 = CONTEXT_DEPENDENT_SHAPE_REPRESENTATION ( #32192, #10751 ) ;
#7497 = DIRECTION ( 'NONE',  ( 1.000000000000000000, 0.000000000000000000, -0.000000000000000000 ) ) ;
#7498 = CARTESIAN_POINT ( 'NONE',  ( 0.1859802865221972246, 25.38927130757771877, 19.93727243998150556 ) ) ;
#7499 = EDGE_LOOP ( 'NONE', ( #6308, #14214, #1903, #2232, #22505, #28404 ) ) ;
#7500 = EDGE_LOOP ( 'NONE', ( #17353, #22619, #28907, #19252 ) ) ;
#7501 = CARTESIAN_POINT ( 'NONE',  ( 0.000000000000000000, 3.909681563761695067, 30.21863799912385673 ) ) ;
#7502 = CARTESIAN_POINT ( 'NONE',  ( 5.390701026406702567, -37.47456861236018000, -36.68877005347593467 ) ) ;
#7503 = FACE_OUTER_BOUND ( 'NONE', #34427, .T. ) ;
#7504 = CARTESIAN_POINT ( 'NONE',  ( 10.17231796313411429, 17.63622956525712127, -77.50000000000000000 ) ) ;
#7505 = CARTESIAN_POINT ( 'NONE',  ( 2.765921099433443331, 26.03801215795517621, 16.98986790278620873 ) ) ;
#7506 = ORIENTED_EDGE ( 'NONE', *, *, #10904, .F. ) ;
#7507 = AXIS2_PLACEMENT_3D ( 'NONE', #4856, #33412, #17247 ) ;
#7508 = CARTESIAN_POINT ( 'NONE',  ( 1.341640786499872284, 0.000000000000000000, 0.000000000000000000 ) ) ;
#7509 = DIRECTION ( 'NONE',  ( -0.000000000000000000, -0.000000000000000000, -1.000000000000000000 ) ) ;
#7510 = AXIS2_PLACEMENT_3D ( 'NONE', #2397, #18449, #34807 ) ;
#7511 =( GEOMETRIC_REPRESENTATION_CONTEXT ( 3 ) GLOBAL_UNCERTAINTY_ASSIGNED_CONTEXT ( ( #22475 ) ) GLOBAL_UNIT_ASSIGNED_CONTEXT ( ( #21468, #29648, #19685 ) ) REPRESENTATION_CONTEXT ( 'NONE', 'WORKASPACE' ) );
#7512 = CARTESIAN_POINT ( 'NONE',  ( 15.99999999999998579, -145.0000000000000000, 162.9999999999999716 ) ) ;
#7513 = CARTESIAN_POINT ( 'NONE',  ( -12.00000000000001066, 124.9999999999999716, 155.0000000000000000 ) ) ;
#7514 = PLANE ( 'NONE',  #25174 ) ;
#7516 = CARTESIAN_POINT ( 'NONE',  ( -109.0419893062853305, 3.151985035376887456, -6.811940677030117186 ) ) ;
#7515 = DIRECTION ( 'NONE',  ( 0.8276889981568903432, -0.5611870653623827199, 0.000000000000000000 ) ) ;
#7517 = DIRECTION ( 'NONE',  ( 1.000000000000000000, 0.000000000000000000, -1.848892746611746966E-32 ) ) ;
#7518 = ORIENTED_EDGE ( 'NONE', *, *, #2444, .T. ) ;
#7519 = CARTESIAN_POINT ( 'NONE',  ( 102.9575692563913236, 5.365524250098477665, -11.29014866489559843 ) ) ;
#7521 = DIRECTION ( 'NONE',  ( 0.5611870653623813876, -0.8276889981568911203, -0.000000000000000000 ) ) ;
#7520 = CARTESIAN_POINT ( 'NONE',  ( 15.99999999999998579, -56.99999999999997868, -154.9999999999999716 ) ) ;
#7522 = ORIENTED_EDGE ( 'NONE', *, *, #18044, .F. ) ;
#7523 = DIRECTION ( 'NONE',  ( -0.000000000000000000, -1.836970198721029688E-16, 1.000000000000000000 ) ) ;
#7524 = VERTEX_POINT ( 'NONE', #31724 ) ;
#7525 = EDGE_CURVE ( 'NONE', #17161, #27507, #4483, .T. ) ;
#7526 = VECTOR ( 'NONE', #18674, 1000.000000000000000 ) ;
#7527 = VECTOR ( 'NONE', #10209, 1000.000000000000000 ) ;
#7528 = AXIS2_PLACEMENT_3D ( 'NONE', #269, #10780, #2575 ) ;
#7529 = ORIENTED_EDGE ( 'NONE', *, *, #12163, .T. ) ;
#7530 = CARTESIAN_POINT ( 'NONE',  ( 2.789999999999999147, -29.00730259674844902, 9.328884633908842261 ) ) ;
#7531 = ORIENTED_EDGE ( 'NONE', *, *, #32979, .T. ) ;
#7532 = ORIENTED_EDGE ( 'NONE', *, *, #5166, .T. ) ;
#7533 = EDGE_CURVE ( 'NONE', #28789, #25461, #26207, .T. ) ;
#7534 = DIRECTION ( 'NONE',  ( 1.000000000000000000, 0.000000000000000000, 0.000000000000000000 ) ) ;
#7535 = EDGE_CURVE ( 'NONE', #28627, #11597, #25920, .T. ) ;
#7536 = DIRECTION ( 'NONE',  ( 0.000000000000000000, 1.836970198721029441E-16, -1.000000000000000000 ) ) ;
#7537 = LINE ( 'NONE', #18251, #29053 ) ;
#7538 = EDGE_CURVE ( 'NONE', #13424, #8890, #26387, .T. ) ;
#7539 = ORIENTED_EDGE ( 'NONE', *, *, #253, .F. ) ;
#7540 = EDGE_CURVE ( 'NONE', #13074, #4867, #26564, .T. ) ;
#7541 = ORIENTED_EDGE ( 'NONE', *, *, #18034, .F. ) ;
#7542 = CYLINDRICAL_SURFACE ( 'NONE', #4292, 2.036051781435508801 ) ;
#7543 = FACE_OUTER_BOUND ( 'NONE', #29636, .T. ) ;
#7544 = DIRECTION ( 'NONE',  ( 0.000000000000000000, 1.836970198721029441E-16, -1.000000000000000000 ) ) ;
#7545 = EDGE_CURVE ( 'NONE', #28866, #29720, #34406, .T. ) ;
#7546 = DIRECTION ( 'NONE',  ( -0.000000000000000000, 0.000000000000000000, 1.000000000000000000 ) ) ;
#7547 = CARTESIAN_POINT ( 'NONE',  ( -345.0000000000000000, 134.9999999999999716, 113.9999999999999858 ) ) ;
#7548 = VERTEX_POINT ( 'NONE', #15545 ) ;
#7549 = ADVANCED_BREP_SHAPE_REPRESENTATION ( '', ( #34166, #28566 ), #18940 ) ;
#7550 = LINE ( 'NONE', #18442, #10578 ) ;
#7551 = AXIS2_PLACEMENT_3D ( 'NONE', #20192, #8449, #22330 ) ;
#7552 = CARTESIAN_POINT ( 'NONE',  ( 2.789999999999999147, -5.984944020945660803, -31.37417528048448645 ) ) ;
#7553 = VERTEX_POINT ( 'NONE', #2007 ) ;
#7554 = LINE ( 'NONE', #15596, #11189 ) ;
#7555 = LINE ( 'NONE', #13098, #29682 ) ;
#7556 = DIRECTION ( 'NONE',  ( 0.1081190184239417262, 0.9941379571543595972, 0.000000000000000000 ) ) ;
#7557 = VERTEX_POINT ( 'NONE', #23726 ) ;
#7558 = AXIS2_PLACEMENT_3D ( 'NONE', #30217, #21857, #22040 ) ;
#7559 = CARTESIAN_POINT ( 'NONE',  ( 2.765921099433443775, -11.07880054387241664, 29.04985141099759360 ) ) ;
#7560 = VERTEX_POINT ( 'NONE', #10198 ) ;
#7561 = VECTOR ( 'NONE', #30203, 1000.000000000000000 ) ;
#7562 = VECTOR ( 'NONE', #20326, 1000.000000000000114 ) ;
#7563 = LINE ( 'NONE', #32129, #9304 ) ;
#7564 = ORIENTED_EDGE ( 'NONE', *, *, #10405, .T. ) ;
#7566 = DIRECTION ( 'NONE',  ( 1.232595164407830946E-32, 3.421138828918010427E-49, -1.000000000000000000 ) ) ;
#7565 = PLANE ( 'NONE',  #3453 ) ;
#7567 = ORIENTED_EDGE ( 'NONE', *, *, #19823, .T. ) ;
#7568 = CYLINDRICAL_SURFACE ( 'NONE', #22295, 3.999999999999976019 ) ;
#7569 = DIRECTION ( 'NONE',  ( 0.000000000000000000, 1.836970198721029441E-16, -1.000000000000000000 ) ) ;
#7570 = VERTEX_POINT ( 'NONE', #7690 ) ;
#7571 = VECTOR ( 'NONE', #27548, 1000.000000000000114 ) ;
#7572 = DIRECTION ( 'NONE',  ( -0.1063910735369225230, 0.9943243633099118073, -1.000770725407345128E-14 ) ) ;
#7573 = ORIENTED_EDGE ( 'NONE', *, *, #25922, .T. ) ;
#7574 = CARTESIAN_POINT ( 'NONE',  ( 1.205771365940040196, 7.794228634059932048, -13.49999999999999822 ) ) ;
#7575 = VERTEX_POINT ( 'NONE', #5016 ) ;
#7576 = DIRECTION ( 'NONE',  ( 0.000000000000000000, 0.000000000000000000, 1.000000000000000000 ) ) ;
#7577 = AXIS2_PLACEMENT_3D ( 'NONE', #34114, #9734, #23949 ) ;
#7578 = DIRECTION ( 'NONE',  ( 0.000000000000000000, 0.000000000000000000, 1.000000000000000000 ) ) ;
#7579 = CIRCLE ( 'NONE', #1899, 2.000000000000001776 ) ;
#7580 = CARTESIAN_POINT ( 'NONE',  ( -100.4342740665978084, -2.311989032590066717, -7.136426621730634245 ) ) ;
#7581 = CARTESIAN_POINT ( 'NONE',  ( 212.5000000000000000, 1.224646799147353256E-15, -10.00000000000000000 ) ) ;
#7582 = ADVANCED_FACE ( 'NONE', ( #21408 ), #15914, .T. ) ;
#7583 = EDGE_LOOP ( 'NONE', ( #22541, #13466, #20401, #12866 ) ) ;
#7584 = EDGE_CURVE ( 'NONE', #5838, #27122, #29763, .T. ) ;
#7585 = EDGE_LOOP ( 'NONE', ( #15443, #6228, #14053, #20033, #23160, #2804, #35019, #7419 ) ) ;
#7586 = PRODUCT_DEFINITION_SHAPE ( 'NONE', 'NONE',  #35207 ) ;
#7587 = ORIENTED_EDGE ( 'NONE', *, *, #19452, .F. ) ;
#7588 = CARTESIAN_POINT ( 'NONE',  ( -28.23027531293552528, -17.65143121711728469, 0.000000000000000000 ) ) ;
#7589 = CARTESIAN_POINT ( 'NONE',  ( 32.40067729534749219, 3.066020821660475626, 49.43553178847298568 ) ) ;
#7590 = LINE ( 'NONE', #4742, #9413 ) ;
#7591 = CARTESIAN_POINT ( 'NONE',  ( -418.0000000000000000, -105.0000000000000142, 139.9999999999999716 ) ) ;
#7593 = DIRECTION ( 'NONE',  ( 0.000000000000000000, 0.000000000000000000, -1.000000000000000000 ) ) ;
#7592 =( REPRESENTATION_RELATIONSHIP ('NONE','NONE', #23037, #15767 ) REPRESENTATION_RELATIONSHIP_WITH_TRANSFORMATION ( #34695 )SHAPE_REPRESENTATION_RELATIONSHIP( ) );
#7594 = CARTESIAN_POINT ( 'NONE',  ( -1.155000000000000027, 0.000000000000000000, 3.930000000000000160 ) ) ;
#7595 = EDGE_LOOP ( 'NONE', ( #25884, #25189, #19260 ) ) ;
#7596 = B_SPLINE_CURVE_WITH_KNOTS ( 'NONE', 3,
 ( #4821, #26548, #18567, #23873 ),
 .UNSPECIFIED., .F., .F.,
 ( 4, 4 ),
 ( 0.005298360586756152568, 0.005985229062776067227 ),
 .UNSPECIFIED. ) ;
#7597 = DIRECTION ( 'NONE',  ( 0.000000000000000000, 0.000000000000000000, 1.000000000000000000 ) ) ;
#7598 = CARTESIAN_POINT ( 'NONE',  ( 0.1859802613287491191, 26.80718912072172344, -17.98567582844204438 ) ) ;
#7599 = ADVANCED_FACE ( 'NONE', ( #19104 ), #32422, .T. ) ;
#7600 = DIRECTION ( 'NONE',  ( -0.000000000000000000, -0.000000000000000000, 1.000000000000000000 ) ) ;
#7601 = ORIENTED_EDGE ( 'NONE', *, *, #32770, .T. ) ;
#7602 = AXIS2_PLACEMENT_3D ( 'NONE', #22004, #24653, #13817 ) ;
#7603 = LINE ( 'NONE', #4937, #7526 ) ;
#7604 = ORIENTED_EDGE ( 'NONE', *, *, #3211, .T. ) ;
#7605 = CARTESIAN_POINT ( 'NONE',  ( -105.6755875751734948, 5.081434799294424209, -11.42078282599713468 ) ) ;
#7606 = EDGE_CURVE ( 'NONE', #4507, #32250, #10003, .T. ) ;
#7607 = CARTESIAN_POINT ( 'NONE',  ( -20.00000000000007461, 112.9999999999999574, -159.0000000000000000 ) ) ;
#7608 = EDGE_CURVE ( 'NONE', #19198, #30770, #5707, .T. ) ;
#7609 = DIRECTION ( 'NONE',  ( -3.040835319149746090E-31, -1.000000000000000000, 0.000000000000000000 ) ) ;
#7610 = ADVANCED_FACE ( 'NONE', ( #32597 ), #27443, .T. ) ;
#7611 = CIRCLE ( 'NONE', #33205, 34.41491905851385269 ) ;
#7612 = ORIENTED_EDGE ( 'NONE', *, *, #7281, .F. ) ;
#7613 = AXIS2_PLACEMENT_3D ( 'NONE', #32180, #8141, #26840 ) ;
#7614 = CARTESIAN_POINT ( 'NONE',  ( 0.000000000000000000, 7.489092610871091793, 29.53582882395389930 ) ) ;
#7615 = DIRECTION ( 'NONE',  ( -1.000000000000000000, -0.000000000000000000, -0.000000000000000000 ) ) ;
#7616 = CARTESIAN_POINT ( 'NONE',  ( 0.000000000000000000, 49.99999999999999289, -9.999999999999998224 ) ) ;
#7617 = VECTOR ( 'NONE', #29535, 1000.000000000000000 ) ;
#7618 = ADVANCED_FACE ( 'NONE', ( #16787 ), #21583, .F. ) ;
#7619 = VERTEX_POINT ( 'NONE', #3053 ) ;
#7620 = B_SPLINE_CURVE_WITH_KNOTS ( 'NONE', 3,
 ( #15345, #1288, #25657, #23001, #33857, #4283 ),
 .UNSPECIFIED., .F., .F.,
 ( 4, 2, 4 ),
 ( 2.380729204623403261E-07, 0.003943479449179655878, 0.007886720825438849058 ),
 .UNSPECIFIED. ) ;
#7621 = VERTEX_POINT ( 'NONE', #24768 ) ;
#7622 = DIRECTION ( 'NONE',  ( -0.1063910735369017202, 0.9943243633099136947, -1.000770725407181676E-14 ) ) ;
#7623 = ORIENTED_EDGE ( 'NONE', *, *, #30632, .F. ) ;
#7624 = LINE ( 'NONE', #2812, #27143 ) ;
#7625 = CARTESIAN_POINT ( 'NONE',  ( -499.9999999999999432, 136.9999999999999432, 162.9999999999999716 ) ) ;
#7626 = VECTOR ( 'NONE', #29268, 1000.000000000000000 ) ;
#7627 = B_SPLINE_CURVE_WITH_KNOTS ( 'NONE', 3,
 ( #8479, #301, #14369, #8828, #25193, #30553 ),
 .UNSPECIFIED., .F., .F.,
 ( 4, 2, 4 ),
 ( 4.404817168095868535E-07, 0.001874269729529001467, 0.003748098977341193273 ),
 .UNSPECIFIED. ) ;
#7628 = DIRECTION ( 'NONE',  ( -0.000000000000000000, -0.000000000000000000, -1.000000000000000000 ) ) ;
#7629 = CARTESIAN_POINT ( 'NONE',  ( 105.9811049962103056, -5.656875047978680904, 4.924762495648698390 ) ) ;
#7630 = EDGE_CURVE ( 'NONE', #916, #27137, #16276, .T. ) ;
#7631 = ORIENTED_EDGE ( 'NONE', *, *, #16410, .T. ) ;
#7632 = DIRECTION ( 'NONE',  ( 0.000000000000000000, 0.000000000000000000, 1.000000000000000000 ) ) ;
#7633 = AXIS2_PLACEMENT_3D ( 'NONE', #20912, #23585, #7195 ) ;
#7634 = CARTESIAN_POINT ( 'NONE',  ( -430.0000000000000000, -133.0000000000000000, 126.0000000000000000 ) ) ;
#7636 = DIRECTION ( 'NONE',  ( 0.000000000000000000, 0.000000000000000000, -1.000000000000000000 ) ) ;
#7635 = DIRECTION ( 'NONE',  ( -1.000000000000000000, 0.000000000000000000, 0.000000000000000000 ) ) ;
#7637 = VECTOR ( 'NONE', #29427, 1000.000000000000000 ) ;
#7638 = ORIENTED_EDGE ( 'NONE', *, *, #31227, .T. ) ;
#7639 = ORIENTED_EDGE ( 'NONE', *, *, #12710, .F. ) ;
#7640 = VECTOR ( 'NONE', #13941, 1000.000000000000000 ) ;
#7641 = DIRECTION ( 'NONE',  ( 0.000000000000000000, 0.000000000000000000, 1.000000000000000000 ) ) ;
#7642 = ORIENTED_EDGE ( 'NONE', *, *, #28523, .T. ) ;
#7643 = VECTOR ( 'NONE', #33781, 1000.000000000000114 ) ;
#7644 = CARTESIAN_POINT ( 'NONE',  ( -449.9999999999999432, 137.0000000000000000, -155.0000000000000000 ) ) ;
#7645 = CARTESIAN_POINT ( 'NONE',  ( 20.89386240318430410, 24.95297350523386726, 68.31122994652405112 ) ) ;
#7646 = ORIENTED_EDGE ( 'NONE', *, *, #7136, .F. ) ;
#7647 = CARTESIAN_POINT ( 'NONE',  ( -35.55956070192387841, -12.65143121711728291, 10.00000000000000000 ) ) ;
#7648 = CYLINDRICAL_SURFACE ( 'NONE', #699, 4.000000000000003553 ) ;
#7649 = ORIENTED_EDGE ( 'NONE', *, *, #20685, .T. ) ;
#7650 = CYLINDRICAL_SURFACE ( 'NONE', #2680, 10.00000000000000000 ) ;
#7651 = CARTESIAN_POINT ( 'NONE',  ( 0.02407890056655564992, -0.3931553186911057041, -31.08824725498900676 ) ) ;
#7652 = ADVANCED_FACE ( 'NONE', ( #16610 ), #30471, .T. ) ;
#7654 = CARTESIAN_POINT ( 'NONE',  ( 1.749999999999999778, 6.714005886385429278, -33.75364837705166110 ) ) ;
#7653 = DIRECTION ( 'NONE',  ( -1.000000000000000000, -0.000000000000000000, 0.000000000000000000 ) ) ;
#7655 = EDGE_CURVE ( 'NONE', #17624, #27112, #21747, .T. ) ;
#7656 = VECTOR ( 'NONE', #555, 1000.000000000000000 ) ;
#7657 = DIRECTION ( 'NONE',  ( 1.000000000000000000, 0.000000000000000000, 0.000000000000000000 ) ) ;
#7658 = CARTESIAN_POINT ( 'NONE',  ( 0.000000000000000000, -0.09145294252700143789, 30.47036804522410236 ) ) ;
#7659 = CARTESIAN_POINT ( 'NONE',  ( -5.210000000000000853, 0.000000000000000000, 0.000000000000000000 ) ) ;
#7660 = AXIS2_PLACEMENT_3D ( 'NONE', #29186, #26509, #5311 ) ;
#7662 = ORIENTED_EDGE ( 'NONE', *, *, #25232, .T. ) ;
#7661 = VECTOR ( 'NONE', #7653, 1000.000000000000000 ) ;
#7663 = VECTOR ( 'NONE', #34331, 1000.000000000000000 ) ;
#7664 = EDGE_LOOP ( 'NONE', ( #11874, #17392, #23792, #32982 ) ) ;
#7665 = AXIS2_PLACEMENT_3D ( 'NONE', #17019, #17548, #14516 ) ;
#7666 = VERTEX_POINT ( 'NONE', #30286 ) ;
#7667 = DIRECTION ( 'NONE',  ( -1.000000000000000000, -0.000000000000000000, -0.000000000000000000 ) ) ;
#7668 = CARTESIAN_POINT ( 'NONE',  ( 751.5001633591576820, 1334.697290463531772, 1332.896119909287563 ) ) ;
#7669 = ORIENTED_EDGE ( 'NONE', *, *, #12702, .T. ) ;
#7670 = ORIENTED_EDGE ( 'NONE', *, *, #12272, .F. ) ;
#7671 = DIRECTION ( 'NONE',  ( -1.000000000000000000, 0.000000000000000000, 0.000000000000000000 ) ) ;
#7672 = FILL_AREA_STYLE ('',( #32058 ) ) ;
#7673 = CONTEXT_DEPENDENT_SHAPE_REPRESENTATION ( #7385, #18140 ) ;
#7674 = AXIS2_PLACEMENT_3D ( 'NONE', #4916, #27166, #32159 ) ;
#7675 = CARTESIAN_POINT ( 'NONE',  ( -5.527271473480783293, -1.747512292859696226, 0.000000000000000000 ) ) ;
#7676 = CARTESIAN_POINT ( 'NONE',  ( 127.4999999999999147, 0.000000000000000000, 0.000000000000000000 ) ) ;
#7677 = ORIENTED_EDGE ( 'NONE', *, *, #1635, .T. ) ;
#7678 = ORIENTED_EDGE ( 'NONE', *, *, #23750, .T. ) ;
#7679 = LINE ( 'NONE', #2176, #34469 ) ;
#7680 = AXIS2_PLACEMENT_3D ( 'NONE', #12713, #15378, #13057 ) ;
#7681 = B_SPLINE_CURVE_WITH_KNOTS ( 'NONE', 3,
 ( #23052, #9520, #31230, #15046, #11673, #19681 ),
 .UNSPECIFIED., .F., .F.,
 ( 4, 2, 4 ),
 ( 4.404817011923048155E-07, 0.001874269613276477800, 0.003748098744851763222 ),
 .UNSPECIFIED. ) ;
#7683 = ADVANCED_FACE ( 'NONE', ( #8403 ), #14106, .T. ) ;
#7682 = DIRECTION ( 'NONE',  ( -0.000000000000000000, -0.000000000000000000, -1.000000000000000000 ) ) ;
#7684 = VECTOR ( 'NONE', #28054, 1000.000000000000000 ) ;
#7685 = CARTESIAN_POINT ( 'NONE',  ( -345.0000000000000000, -125.0000000000000284, 181.0000000000000000 ) ) ;
#7686 = CARTESIAN_POINT ( 'NONE',  ( 0.07098932668446723826, 14.74869129583196958, 28.05389252521654342 ) ) ;
#7687 = FACE_OUTER_BOUND ( 'NONE', #20874, .T. ) ;
#7688 = ORIENTED_EDGE ( 'NONE', *, *, #23863, .T. ) ;
#7689 = CARTESIAN_POINT ( 'NONE',  ( 13.32059394339353986, -35.43959265050634144, 68.31122994652405112 ) ) ;
#7690 = CARTESIAN_POINT ( 'NONE',  ( 0.02407890056655738464, 28.29688452313417812, -12.88099432405573630 ) ) ;
#7691 = VECTOR ( 'NONE', #16711, 1000.000000000000000 ) ;
#7692 = AXIS2_PLACEMENT_3D ( 'NONE', #26879, #21717, #11043 ) ;
#7693 = DIRECTION ( 'NONE',  ( -3.040835319149746528E-31, -1.000000000000000000, 0.000000000000000000 ) ) ;
#7694 = ADVANCED_FACE ( 'NONE', ( #16435 ), #19278, .T. ) ;
#7695 = DIRECTION ( 'NONE',  ( 0.000000000000000000, -1.000000000000000000, -2.465190328815662439E-32 ) ) ;
#7696 = CARTESIAN_POINT ( 'NONE',  ( 109.9315740078916690, 2.939425563888521609, -6.902236325305502795 ) ) ;
#7697 = EDGE_CURVE ( 'NONE', #8132, #23220, #1522, .T. ) ;
#7699 = DIRECTION ( 'NONE',  ( 0.1081190184239420177, 0.9941379571543595972, -0.000000000000000000 ) ) ;
#7698 = CARTESIAN_POINT ( 'NONE',  ( 2.265105863614538695, 20.67343389904883111, 26.20724806577312904 ) ) ;
#7700 = AXIS2_PLACEMENT_3D ( 'NONE', #29619, #31585, #31920 ) ;
#7701 = EDGE_CURVE ( 'NONE', #6283, #6435, #16259, .T. ) ;
#7702 = CARTESIAN_POINT ( 'NONE',  ( 0.2989565185775198697, 1.556832243416072701E-15, -11.22499999999999787 ) ) ;
#7703 = ORIENTED_EDGE ( 'NONE', *, *, #34768, .T. ) ;
#7704 = EDGE_CURVE ( 'NONE', #32148, #10173, #21931, .T. ) ;
#7705 = CARTESIAN_POINT ( 'NONE',  ( 110.7008314884919287, 0.7568087271434544849, -12.48276086518024464 ) ) ;
#7707 = CARTESIAN_POINT ( 'NONE',  ( -410.0000000000000568, 124.9999999999999432, -162.9999999999999716 ) ) ;
#7706 = FACE_OUTER_BOUND ( 'NONE', #21398, .T. ) ;
#7708 = AXIS2_PLACEMENT_3D ( 'NONE', #11779, #33468, #22629 ) ;
#7709 = ORIENTED_EDGE ( 'NONE', *, *, #15476, .T. ) ;
#7710 = DIRECTION ( 'NONE',  ( 1.000000000000000000, 0.000000000000000000, 0.000000000000000000 ) ) ;
#7711 = VECTOR ( 'NONE', #29628, 1000.000000000000000 ) ;
#7712 = ORIENTED_EDGE ( 'NONE', *, *, #2390, .T. ) ;
#7713 = VERTEX_POINT ( 'NONE', #2872 ) ;
#7714 = FACE_BOUND ( 'NONE', #32822, .T. ) ;
#7715 = VERTEX_POINT ( 'NONE', #13747 ) ;
#7716 = VERTEX_POINT ( 'NONE', #32776 ) ;
#7717 = DIRECTION ( 'NONE',  ( 0.000000000000000000, 2.465190328815661892E-32, 1.000000000000000000 ) ) ;
#7718 = COLOUR_RGB ( '',0.7921568627450980005, 0.8196078431372548767, 0.9333333333333333481 ) ;
#7719 = CARTESIAN_POINT ( 'NONE',  ( 110.7380848894536598, 7.027127293105237708E-16, -57.49999999999999289 ) ) ;
#7720 = DIRECTION ( 'NONE',  ( -0.8276889981568903432, 0.5611870653623828309, 0.000000000000000000 ) ) ;
#7721 = VERTEX_POINT ( 'NONE', #11082 ) ;
#7722 = ORIENTED_EDGE ( 'NONE', *, *, #1578, .T. ) ;
#7723 = CARTESIAN_POINT ( 'NONE',  ( -345.0000000000000000, 124.9999999999999432, 168.9999999999999716 ) ) ;
#7724 = DIRECTION ( 'NONE',  ( 1.000000000000000000, -0.000000000000000000, -0.000000000000000000 ) ) ;
#7725 = CARTESIAN_POINT ( 'NONE',  ( 5.021133111224473033, 6.201984591278717041, -67.50000000000000000 ) ) ;
#7726 = CARTESIAN_POINT ( 'NONE',  ( 0.000000000000000000, 0.000000000000000000, 0.000000000000000000 ) ) ;
#7727 = DIRECTION ( 'NONE',  ( -1.000000000000000000, 0.000000000000000000, 0.000000000000000000 ) ) ;
#7728 = ORIENTED_EDGE ( 'NONE', *, *, #4662, .T. ) ;
#7729 = VECTOR ( 'NONE', #1309, 1000.000000000000000 ) ;
#7730 = DIRECTION ( 'NONE',  ( 0.000000000000000000, 0.000000000000000000, 1.000000000000000000 ) ) ;
#7731 = DIRECTION ( 'NONE',  ( 0.000000000000000000, 0.000000000000000000, -1.000000000000000000 ) ) ;
#7732 = EDGE_LOOP ( 'NONE', ( #22287, #16154, #10591, #2077 ) ) ;
#7733 = EDGE_CURVE ( 'NONE', #13445, #21650, #25110, .T. ) ;
#7734 = VECTOR ( 'NONE', #21322, 1000.000000000000000 ) ;
#7735 = DIRECTION ( 'NONE',  ( -0.9635499925192231307, -0.2675283385292199223, 0.000000000000000000 ) ) ;
#7736 = CARTESIAN_POINT ( 'NONE',  ( 29.44023756548696369, 13.87360028845404969, 68.31122994652405112 ) ) ;
#7737 = EDGE_CURVE ( 'NONE', #14830, #1305, #840, .T. ) ;
#7738 = CARTESIAN_POINT ( 'NONE',  ( -12.00000000000001066, 134.9999999999998863, 187.0000000000000000 ) ) ;
#7739 = ORIENTED_EDGE ( 'NONE', *, *, #15312, .T. ) ;
#7740 = DIRECTION ( 'NONE',  ( 0.000000000000000000, -1.000000000000000000, -2.132064625830773463E-16 ) ) ;
#7741 = EDGE_LOOP ( 'NONE', ( #21467, #32024, #2663, #11767, #29338, #9409 ) ) ;
#7742 = LINE ( 'NONE', #15959, #8151 ) ;
#7743 = EDGE_LOOP ( 'NONE', ( #30871, #1289, #24851, #34537 ) ) ;
#7744 = ADVANCED_FACE ( 'NONE', ( #12617 ), #34315, .F. ) ;
#7746 = CARTESIAN_POINT ( 'NONE',  ( -10.84269519964070305, -36.27449394610879096, 68.31122994652405112 ) ) ;
#7745 = CARTESIAN_POINT ( 'NONE',  ( -70.00000000000000000, 75.55999999999990280, -177.7400000000000091 ) ) ;
#7747 = DIRECTION ( 'NONE',  ( -1.000000000000000000, 0.000000000000000000, 0.000000000000000000 ) ) ;
#7748 = ORIENTED_EDGE ( 'NONE', *, *, #27426, .F. ) ;
#7749 = ADVANCED_FACE ( 'NONE', ( #4567 ), #1744, .T. ) ;
#7750 = FACE_OUTER_BOUND ( 'NONE', #6089, .T. ) ;
#7751 = FACE_OUTER_BOUND ( 'NONE', #24508, .T. ) ;
#7752 = EDGE_CURVE ( 'NONE', #27733, #25432, #28758, .T. ) ;
#7753 = ORIENTED_EDGE ( 'NONE', *, *, #28290, .T. ) ;
#7754 = EDGE_CURVE ( 'NONE', #25273, #4606, #23458, .T. ) ;
#7755 = VECTOR ( 'NONE', #34003, 1000.000000000000000 ) ;
#7756 = DIRECTION ( 'NONE',  ( -0.1063910735369225230, 0.9943243633099118073, -1.000770725407345128E-14 ) ) ;
#7757 = ORIENTED_EDGE ( 'NONE', *, *, #11062, .T. ) ;
#7758 = CARTESIAN_POINT ( 'NONE',  ( -99.88497961182923746, 0.3508469386294337244, 7.500000000000000888 ) ) ;
#7759 = VERTEX_POINT ( 'NONE', #7422 ) ;
#7760 = CARTESIAN_POINT ( 'NONE',  ( 44.94043929807611448, -32.65143121711728469, 20.00000000000000000 ) ) ;
#7761 = CARTESIAN_POINT ( 'NONE',  ( 2.765921099433442443, 31.00221527374952046, -2.344426712874310148 ) ) ;
#7762 = CARTESIAN_POINT ( 'NONE',  ( -103.6349267833586651, -4.941537997685731654, -5.642681918066577929 ) ) ;
#7763 = CARTESIAN_POINT ( 'NONE',  ( -418.0000000000000000, -125.0000000000000000, 159.0000000000000000 ) ) ;
#7764 = ORIENTED_EDGE ( 'NONE', *, *, #16575, .T. ) ;
#7765 = ORIENTED_EDGE ( 'NONE', *, *, #15906, .T. ) ;
#7766 = ORIENTED_EDGE ( 'NONE', *, *, #34557, .T. ) ;
#7767 = CARTESIAN_POINT ( 'NONE',  ( 5.021133111224473033, 4.168562732279004202, -67.50000000000000000 ) ) ;
#7768 = B_SPLINE_CURVE_WITH_KNOTS ( 'NONE', 3,
 ( #8083, #19140, #11123, #14143, #27654, #21785, #32811, #5742, #30511, #13609, #781, #16469, #3091, #14325, #25152, #6105, #21616, #30144, #257, #32456, #32980, #21970, #24973, #8437, #27828, #19310, #16646, #8605, #18958, #19666, #5927, #29801, #27479, #17004, #5406, #604, #29978, #32633, #5573, #11294, #16294, #27126, #8260 ),
 .UNSPECIFIED., .F., .F.,
 ( 4, 2, 2, 2, 2, 2, 2, 2, 2, 2, 2, 1, 2, 2, 2, 2, 2, 2, 2, 2, 2, 4 ),
 ( 0.01819865299508306028, 0.01933465672311146522, 0.02047066045113987015, 0.02103866231515406568, 0.02160666417916826121, 0.02217466604318245327, 0.02274266790719664880, 0.02387867163522501210, 0.02501467536325337540, 0.02615067909128173870, 0.02671868095529592035, 0.02728668281931010547, 0.02785468468332428366, 0.02842268654733846878, 0.02955869027536687371, 0.03069469400339527518, 0.03183069773142367664, 0.03296670145945208852, 0.03353470332346628752, 0.03410270518748048652, 0.03523870891550889839, 0.03637471264353730332 ),
 .UNSPECIFIED. ) ;
#7769 = B_SPLINE_CURVE_WITH_KNOTS ( 'NONE', 3,
 ( #21611, #8430, #13604, #21964 ),
 .UNSPECIFIED., .F., .F.,
 ( 4, 4 ),
 ( 2.876507994500877895E-07, 0.0006880240977454964548 ),
 .UNSPECIFIED. ) ;
#7770 = LINE ( 'NONE', #7949, #19201 ) ;
#7771 = FACE_OUTER_BOUND ( 'NONE', #29126, .T. ) ;
#7772 = LINE ( 'NONE', #2260, #15641 ) ;
#7773 = DIRECTION ( 'NONE',  ( 0.000000000000000000, -1.836970198721029934E-16, 1.000000000000000000 ) ) ;
#7774 = DIRECTION ( 'NONE',  ( -0.000000000000000000, -0.000000000000000000, 1.000000000000000000 ) ) ;
#7775 = FACE_OUTER_BOUND ( 'NONE', #31395, .T. ) ;
#7776 = VERTEX_POINT ( 'NONE', #17136 ) ;
#7777 = VECTOR ( 'NONE', #30607, 1000.000000000000000 ) ;
#7778 = LINE ( 'NONE', #29677, #7734 ) ;
#7779 = DIRECTION ( 'NONE',  ( -0.000000000000000000, 5.053935297177146739E-49, 1.000000000000000000 ) ) ;
#7780 = CARTESIAN_POINT ( 'NONE',  ( -5.527271473480783293, -1.747512292859696226, 3.180000000000000160 ) ) ;
#7781 = ORIENTED_EDGE ( 'NONE', *, *, #20959, .F. ) ;
#7782 = AXIS2_PLACEMENT_3D ( 'NONE', #34344, #32017, #4777 ) ;
#7783 = FACE_OUTER_BOUND ( 'NONE', #32835, .T. ) ;
#7784 = ORIENTED_EDGE ( 'NONE', *, *, #26682, .T. ) ;
#7785 = CARTESIAN_POINT ( 'NONE',  ( -12.00000000000001243, 134.9999999999999432, -154.9999999999999716 ) ) ;
#7786 = EDGE_CURVE ( 'NONE', #17311, #24353, #5919, .T. ) ;
#7787 = DIRECTION ( 'NONE',  ( 0.000000000000000000, 0.000000000000000000, -1.000000000000000000 ) ) ;
#7788 = EDGE_LOOP ( 'NONE', ( #21908, #34638, #6025, #31710 ) ) ;
#7789 = EDGE_CURVE ( 'NONE', #6643, #2811, #34451, .T. ) ;
#7790 = ADVANCED_FACE ( 'NONE', ( #33484 ), #11967, .F. ) ;
#7791 = DIRECTION ( 'NONE',  ( 1.000000000000000000, -0.000000000000000000, -0.000000000000000000 ) ) ;
#7792 = VECTOR ( 'NONE', #28961, 1000.000000000000000 ) ;
#7793 = FACE_OUTER_BOUND ( 'NONE', #11460, .T. ) ;
#7794 = DIRECTION ( 'NONE',  ( 1.000000000000000000, 0.000000000000000000, -0.000000000000000000 ) ) ;
#7795 = ORIENTED_EDGE ( 'NONE', *, *, #12555, .F. ) ;
#7796 = ORIENTED_EDGE ( 'NONE', *, *, #6555, .F. ) ;
#7797 = AXIS2_PLACEMENT_3D ( 'NONE', #16325, #27324, #27681 ) ;
#7798 = DIRECTION ( 'NONE',  ( 0.9646352864427241158, 0.2635882473661587122, 1.856746474777097304E-14 ) ) ;
#7799 = CARTESIAN_POINT ( 'NONE',  ( -145.0000000000000568, -97.56119630548165844, -180.0000000000000000 ) ) ;
#7800 = EDGE_LOOP ( 'NONE', ( #5558, #29761, #17522, #34106, #21177, #704 ) ) ;
#7801 = DIRECTION ( 'NONE',  ( 0.000000000000000000, 1.836970198721029934E-16, -1.000000000000000000 ) ) ;
#7802 = EDGE_CURVE ( 'NONE', #7313, #3609, #6236, .T. ) ;
#7803 =( NAMED_UNIT ( * ) SI_UNIT ( $, .STERADIAN. ) SOLID_ANGLE_UNIT ( ) );
#7804 = CIRCLE ( 'NONE', #30538, 30.47050528711512030 ) ;
#7805 = CIRCLE ( 'NONE', #17508, 10.00000000000000000 ) ;
#7806 = DIRECTION ( 'NONE',  ( -0.000000000000000000, -0.000000000000000000, -1.000000000000000000 ) ) ;
#7807 = CARTESIAN_POINT ( 'NONE',  ( 0.000000000000000000, -27.53147453683416757, -13.05640081644872197 ) ) ;
#7808 = CONTEXT_DEPENDENT_SHAPE_REPRESENTATION ( #25798, #1799 ) ;
#7809 = APPLICATION_CONTEXT ( 'automotive_design' ) ;
#7810 = ORIENTED_EDGE ( 'NONE', *, *, #19794, .F. ) ;
#7811 = PLANE ( 'NONE',  #1043 ) ;
#7812 = EDGE_CURVE ( 'NONE', #6257, #33253, #6593, .T. ) ;
#7813 = AXIS2_PLACEMENT_3D ( 'NONE', #11340, #6323, #8651 ) ;
#7814 = ADVANCED_FACE ( 'NONE', ( #19969 ), #18317, .T. ) ;
#7816 = LINE ( 'NONE', #6147, #34613 ) ;
#7815 = DIRECTION ( 'NONE',  ( 0.000000000000000000, 1.000000000000000000, 1.836970198721029688E-16 ) ) ;
#7817 = EDGE_CURVE ( 'NONE', #30541, #29056, #14809, .T. ) ;
#7818 = ORIENTED_EDGE ( 'NONE', *, *, #15617, .F. ) ;
#7819 = VERTEX_POINT ( 'NONE', #7248 ) ;
#7820 = DIRECTION ( 'NONE',  ( -1.000000000000000000, 0.000000000000000000, 0.000000000000000000 ) ) ;
#7821 = EDGE_LOOP ( 'NONE', ( #162, #13824, #12393, #22072 ) ) ;
#7822 = B_SPLINE_CURVE_WITH_KNOTS ( 'NONE', 3,
 ( #8271, #448, #13448, #11132, #32820, #22157 ),
 .UNSPECIFIED., .F., .F.,
 ( 4, 2, 4 ),
 ( 1.974571759321287545E-07, 0.001873395748763630230, 0.003746594040351328408 ),
 .UNSPECIFIED. ) ;
#7823 = CARTESIAN_POINT ( 'NONE',  ( 2.789999999999999147, -3.728217946242703196, -30.24156218513559935 ) ) ;
#7824 = CARTESIAN_POINT ( 'NONE',  ( -430.0000000000000000, 118.9999999999999716, 113.9999999999999858 ) ) ;
#7825 = ORIENTED_EDGE ( 'NONE', *, *, #18799, .F. ) ;
#7826 = DIRECTION ( 'NONE',  ( 1.000000000000000000, 0.000000000000000000, 0.000000000000000000 ) ) ;
#7827 = TOROIDAL_SURFACE ( 'NONE', #14698, 30.47050528711511674, 8.000000000000000000 ) ;
#7828 = CARTESIAN_POINT ( 'NONE',  ( 0.000000000000000000, -11.69134295108991672, -6.750000000000007105 ) ) ;
#7829 = EDGE_LOOP ( 'NONE', ( #26573, #28655, #1430, #1724 ) ) ;
#7830 = PLANE ( 'NONE',  #17526 ) ;
#7831 = CARTESIAN_POINT ( 'NONE',  ( 187.4264068711928530, -12.50000000000000888, -14.99999999999998757 ) ) ;
#7832 = CARTESIAN_POINT ( 'NONE',  ( -418.0000000000000000, -125.0000000000000000, -109.9999999999999574 ) ) ;
#7834 = DIRECTION ( 'NONE',  ( 0.000000000000000000, 1.836970198721029441E-16, -1.000000000000000000 ) ) ;
#7833 = DIRECTION ( 'NONE',  ( 0.000000000000000000, 1.836970198721029934E-16, -1.000000000000000000 ) ) ;
#7835 = AXIS2_PLACEMENT_3D ( 'NONE', #34944, #16436, #5187 ) ;
#7836 = CIRCLE ( 'NONE', #14105, 30.47050528711511674 ) ;
#7837 = ADVANCED_FACE ( 'NONE', ( #18152 ), #28978, .F. ) ;
#7838 = ADVANCED_FACE ( 'NONE', ( #1914 ), #745, .T. ) ;
#7839 = PLANE ( 'NONE',  #27929 ) ;
#7840 = CARTESIAN_POINT ( 'NONE',  ( -349.0000000000000000, -125.0000000000000284, 168.9999999999999716 ) ) ;
#7841 = CARTESIAN_POINT ( 'NONE',  ( 2.789999999999999147, 31.00221527374952046, 2.344426712874309260 ) ) ;
#7842 = ADVANCED_FACE ( 'NONE', ( #18666 ), #29511, .F. ) ;
#7843 = VECTOR ( 'NONE', #15241, 1000.000000000000000 ) ;
#7844 = VERTEX_POINT ( 'NONE', #27177 ) ;
#7845 = DIRECTION ( 'NONE',  ( -1.000000000000000000, 0.000000000000000000, 0.000000000000000000 ) ) ;
#7846 = CARTESIAN_POINT ( 'NONE',  ( 824.8301442019338765, 989.3487216806460083, 1654.189744389411317 ) ) ;
#7847 = PRODUCT_DEFINITION_CONTEXT ( 'detailed design', #12152, 'design' ) ;
#7848 = ORIENTED_EDGE ( 'NONE', *, *, #14205, .T. ) ;
#7849 = ORIENTED_EDGE ( 'NONE', *, *, #30287, .T. ) ;
#7850 = DIRECTION ( 'NONE',  ( -1.000000000000000000, -0.000000000000000000, -0.000000000000000000 ) ) ;
#7851 = DIRECTION ( 'NONE',  ( 0.000000000000000000, 0.000000000000000000, 1.000000000000000000 ) ) ;
#7852 = ORIENTED_EDGE ( 'NONE', *, *, #33222, .F. ) ;
#7853 = CARTESIAN_POINT ( 'NONE',  ( 145.0000000000000568, -78.33668825982579165, -65.00000000000000000 ) ) ;
#7854 = EDGE_CURVE ( 'NONE', #1246, #15960, #21952, .T. ) ;
#7855 = ITEM_DEFINED_TRANSFORMATION ( 'NONE', 'NONE', #1359,  #28566 ) ;
#7856 = VECTOR ( 'NONE', #2645, 1000.000000000000000 ) ;
#7857 = EDGE_CURVE ( 'NONE', #22621, #11445, #2265, .T. ) ;
#7858 = CARTESIAN_POINT ( 'NONE',  ( 1.749999999999999778, -18.66807150955392913, -28.91175816027522671 ) ) ;
#7859 = ORIENTED_EDGE ( 'NONE', *, *, #25543, .F. ) ;
#7860 = ORIENTED_EDGE ( 'NONE', *, *, #29038, .F. ) ;
#7861 =( REPRESENTATION_RELATIONSHIP ('NONE','NONE', #23037, #28231 ) REPRESENTATION_RELATIONSHIP_WITH_TRANSFORMATION ( #6972 )SHAPE_REPRESENTATION_RELATIONSHIP( ) );
#7862 = CIRCLE ( 'NONE', #23152, 2.525000000000001243 ) ;
#7863 = DIRECTION ( 'NONE',  ( 1.000000000000000000, 0.000000000000000000, 0.000000000000000000 ) ) ;
#7864 = CARTESIAN_POINT ( 'NONE',  ( 0.000000000000000000, 25.67797970382157402, -16.40405592474731833 ) ) ;
#7865 = EDGE_CURVE ( 'NONE', #21604, #32940, #13421, .T. ) ;
#7866 = CARTESIAN_POINT ( 'NONE',  ( 7.700000000000001954, 0.000000000000000000, 0.000000000000000000 ) ) ;
#7867 = DIRECTION ( 'NONE',  ( 0.000000000000000000, 0.000000000000000000, -1.000000000000000000 ) ) ;
#7868 = CARTESIAN_POINT ( 'NONE',  ( -365.0000000000000000, -119.0000000000000000, 130.0000000000000000 ) ) ;
#7869 = B_SPLINE_CURVE_WITH_KNOTS ( 'NONE', 3,
 ( #5481, #513, #27376, #19217, #22048, #13682 ),
 .UNSPECIFIED., .F., .F.,
 ( 4, 2, 4 ),
 ( 2.008842330397746412E-07, 0.001873399179558948857, 0.003746597474884857948 ),
 .UNSPECIFIED. ) ;
#7870 = ORIENTED_EDGE ( 'NONE', *, *, #13875, .F. ) ;
#7871 = VECTOR ( 'NONE', #33795, 1000.000000000000114 ) ;
#7872 = CARTESIAN_POINT ( 'NONE',  ( -70.00000000000000000, 4.559999999999908127, 172.9900000000000091 ) ) ;
#7873 = DIRECTION ( 'NONE',  ( 0.000000000000000000, 1.000000000000000000, 0.000000000000000000 ) ) ;
#7874 = PLANE ( 'NONE',  #23193 ) ;
#7875 = EDGE_CURVE ( 'NONE', #5682, #27718, #34858, .T. ) ;
#7876 = CARTESIAN_POINT ( 'NONE',  ( 0.7561992144253976145, -25.08322906883816117, -22.82697412903104350 ) ) ;
#7877 = PLANE ( 'NONE',  #8613 ) ;
#7878 = VECTOR ( 'NONE', #33084, 1000.000000000000000 ) ;
#7879 = DIRECTION ( 'NONE',  ( -1.000000000000000000, -0.000000000000000000, -0.000000000000000000 ) ) ;
#7881 = CARTESIAN_POINT ( 'NONE',  ( -100.1623731062489355, 1.695881020439946596, -7.312931660397135047 ) ) ;
#7880 = CARTESIAN_POINT ( 'NONE',  ( 2.765921099433441999, -17.95514392185434360, 25.38201125280350468 ) ) ;
#7882 = VECTOR ( 'NONE', #25195, 1000.000000000000000 ) ;
#7883 = DIRECTION ( 'NONE',  ( 0.000000000000000000, 1.000000000000000000, 0.000000000000000000 ) ) ;
#7884 = ORIENTED_EDGE ( 'NONE', *, *, #175, .T. ) ;
#7885 = DIRECTION ( 'NONE',  ( 0.000000000000000000, 0.000000000000000000, 1.000000000000000000 ) ) ;
#7887 = CARTESIAN_POINT ( 'NONE',  ( 2.265105745614923727, -33.37077467988373058, -0.7759739055977695754 ) ) ;
#7886 = LINE ( 'NONE', #23896, #7527 ) ;
#7888 = VECTOR ( 'NONE', #26284, 1000.000000000000000 ) ;
#7889 = ORIENTED_EDGE ( 'NONE', *, *, #33581, .F. ) ;
#7890 = CARTESIAN_POINT ( 'NONE',  ( -110.1150203881707910, 3.829664765295703645E-16, -7.500000000000000000 ) ) ;
#7891 = PRODUCT_DEFINITION_SHAPE ( 'NONE', 'NONE',  #35201 ) ;
#7892 = EDGE_CURVE ( 'NONE', #19057, #8463, #21498, .T. ) ;
#7893 = ORIENTED_EDGE ( 'NONE', *, *, #1833, .F. ) ;
#7894 = AXIS2_PLACEMENT_3D ( 'NONE', #29937, #25957, #9933 ) ;
#7895 = EDGE_LOOP ( 'NONE', ( #18240, #17119, #7639, #33474 ) ) ;
#7896 = FACE_BOUND ( 'NONE', #20563, .T. ) ;
#7897 = ORIENTED_EDGE ( 'NONE', *, *, #26520, .F. ) ;
#7898 = ORIENTED_EDGE ( 'NONE', *, *, #10412, .F. ) ;
#7899 = DIRECTION ( 'NONE',  ( -1.000000000000000000, -0.000000000000000000, -0.000000000000000000 ) ) ;
#7900 = EDGE_CURVE ( 'NONE', #18455, #11327, #23813, .T. ) ;
#7901 = EDGE_CURVE ( 'NONE', #11290, #15534, #32338, .T. ) ;
#7902 = EDGE_CURVE ( 'NONE', #25989, #11449, #12326, .T. ) ;
#7903 = VECTOR ( 'NONE', #8740, 1000.000000000000000 ) ;
#7904 = LINE ( 'NONE', #26072, #29894 ) ;
#7905 = CARTESIAN_POINT ( 'NONE',  ( -418.0000000000000000, -124.9999999999999858, -73.99999999999998579 ) ) ;
#7906 = VERTEX_POINT ( 'NONE', #8314 ) ;
#7907 = ORIENTED_EDGE ( 'NONE', *, *, #18077, .T. ) ;
#7908 = CARTESIAN_POINT ( 'NONE',  ( -20.00000000000007461, 112.9999999999999574, 159.0000000000000000 ) ) ;
#7909 = FILL_AREA_STYLE_COLOUR ( '', #15827 ) ;
#7910 = DIRECTION ( 'NONE',  ( 0.000000000000000000, 0.000000000000000000, -1.000000000000000000 ) ) ;
#7911 = CYLINDRICAL_SURFACE ( 'NONE', #10843, 5.738084889453667792 ) ;
#7912 = ORIENTED_EDGE ( 'NONE', *, *, #9086, .T. ) ;
#7913 = AXIS2_PLACEMENT_3D ( 'NONE', #26723, #33913, #25540 ) ;
#7914 = CARTESIAN_POINT ( 'NONE',  ( -5.469264258321805627, 1.713938105891546382, -0.7500000000000000000 ) ) ;
#7915 = DIRECTION ( 'NONE',  ( 0.000000000000000000, -3.374343856708137958E-53, 1.000000000000000000 ) ) ;
#7916 = ORIENTED_EDGE ( 'NONE', *, *, #25648, .T. ) ;
#7917 = CARTESIAN_POINT ( 'NONE',  ( -500.0000000000000000, -137.0000000000000000, 155.0000000000000000 ) ) ;
#7918 = CARTESIAN_POINT ( 'NONE',  ( 2.789999999999999147, -29.91351748324107263, 5.799410679710522487 ) ) ;
#7919 = CARTESIAN_POINT ( 'NONE',  ( -32.71222340678873053, 19.07754906224033675, 68.31122994652405112 ) ) ;
#7920 = ORIENTED_EDGE ( 'NONE', *, *, #522, .T. ) ;
#7921 = VECTOR ( 'NONE', #27483, 1000.000000000000000 ) ;
#7922 = CARTESIAN_POINT ( 'NONE',  ( -442.0000000000000000, -137.0000000000000000, 154.9999999999999716 ) ) ;
#7923 = ORIENTED_EDGE ( 'NONE', *, *, #15699, .T. ) ;
#7924 = LINE ( 'NONE', #29297, #5271 ) ;
#7925 = ORIENTED_EDGE ( 'NONE', *, *, #33501, .T. ) ;
#7927 = CARTESIAN_POINT ( 'NONE',  ( 2.033800775632456759, -29.46088656861438793, -16.80164552011282808 ) ) ;
#7926 = PRESENTATION_STYLE_ASSIGNMENT (( #19325 ) ) ;
#7928 = AXIS2_PLACEMENT_3D ( 'NONE', #32942, #5360, #27085 ) ;
#7929 = ORIENTED_EDGE ( 'NONE', *, *, #33766, .F. ) ;
#7930 = DIRECTION ( 'NONE',  ( 0.000000000000000000, 0.000000000000000000, 1.000000000000000000 ) ) ;
#7931 = ORIENTED_EDGE ( 'NONE', *, *, #32770, .F. ) ;
#7932 = DIRECTION ( 'NONE',  ( -0.1063910735369225230, 0.9943243633099118073, -1.000770725407345128E-14 ) ) ;
#7933 = EDGE_CURVE ( 'NONE', #32587, #8985, #20264, .T. ) ;
#7934 = ORIENTED_EDGE ( 'NONE', *, *, #11535, .F. ) ;
#7935 = CARTESIAN_POINT ( 'NONE',  ( -102.4133971961325926, 4.424631548980197060, 6.059743929710633026 ) ) ;
#7936 = ORIENTED_EDGE ( 'NONE', *, *, #11972, .T. ) ;
#7937 = CARTESIAN_POINT ( 'NONE',  ( 1.395000000000002238, -34.41385771548413430, -0.2702793785573798790 ) ) ;
#7938 = EDGE_CURVE ( 'NONE', #17702, #28091, #27009, .T. ) ;
#7939 = AXIS2_PLACEMENT_3D ( 'NONE', #5082, #32149, #10967 ) ;
#7940 = DIRECTION ( 'NONE',  ( -1.000000000000000000, -0.000000000000000000, -0.000000000000000000 ) ) ;
#7941 = EDGE_CURVE ( 'NONE', #28175, #30030, #7778, .T. ) ;
#7942 = CARTESIAN_POINT ( 'NONE',  ( -100.5942677908518306, -2.603972021169325135, -7.035140931575556422 ) ) ;
#7943 = CARTESIAN_POINT ( 'NONE',  ( -28.23027531293552528, -17.65143121711728469, 20.00000000000000000 ) ) ;
#7944 = ORIENTED_EDGE ( 'NONE', *, *, #762, .F. ) ;
#7945 = ORIENTED_EDGE ( 'NONE', *, *, #5916, .T. ) ;
#7946 = VERTEX_POINT ( 'NONE', #5278 ) ;
#7947 = LINE ( 'NONE', #8120, #16812 ) ;
#7948 = ADVANCED_FACE ( 'NONE', ( #26477 ), #2618, .T. ) ;
#7949 = CARTESIAN_POINT ( 'NONE',  ( -499.9999999999999432, 104.9999999999999858, 162.9999999999999716 ) ) ;
#7950 = LINE ( 'NONE', #5267, #12061 ) ;
#7951 = DIRECTION ( 'NONE',  ( -1.000000000000000000, 0.000000000000000000, 0.000000000000000000 ) ) ;
#7952 = FACE_OUTER_BOUND ( 'NONE', #26976, .T. ) ;
#7953 = CARTESIAN_POINT ( 'NONE',  ( -5.781867695661277118, -1.866624223957557893, 5.429999999999999716 ) ) ;
#7954 = DIRECTION ( 'NONE',  ( -0.000000000000000000, -0.000000000000000000, -1.000000000000000000 ) ) ;
#7955 = ORIENTED_EDGE ( 'NONE', *, *, #5611, .T. ) ;
#7956 = DIRECTION ( 'NONE',  ( -1.000000000000000000, 0.000000000000000000, -0.000000000000000000 ) ) ;
#7957 = ADVANCED_FACE ( 'NONE', ( #13486, #10282 ), #21140, .T. ) ;
#7958 = DIRECTION ( 'NONE',  ( 0.000000000000000000, 0.000000000000000000, 1.000000000000000000 ) ) ;
#7959 = CARTESIAN_POINT ( 'NONE',  ( -20.00000000000004619, -137.0000000000000000, -190.9999999999999716 ) ) ;
#7960 = ORIENTED_EDGE ( 'NONE', *, *, #11222, .T. ) ;
#7961 = DIRECTION ( 'NONE',  ( -1.000000000000000000, 0.000000000000000000, 0.000000000000000000 ) ) ;
#7962 = ORIENTED_EDGE ( 'NONE', *, *, #34586, .F. ) ;
#7963 = CARTESIAN_POINT ( 'NONE',  ( -101.1480816615366223, 3.381649300054700991, -12.03636906590512723 ) ) ;
#7964 = LINE ( 'NONE', #21670, #26368 ) ;
#7965 = AXIS2_PLACEMENT_3D ( 'NONE', #25804, #12300, #30631 ) ;
#7966 = ORIENTED_EDGE ( 'NONE', *, *, #2239, .F. ) ;
#7967 = DIRECTION ( 'NONE',  ( -0.000000000000000000, -0.000000000000000000, 1.000000000000000000 ) ) ;
#7968 = DIRECTION ( 'NONE',  ( -0.000000000000000000, -0.000000000000000000, -1.000000000000000000 ) ) ;
#7969 = DIRECTION ( 'NONE',  ( 1.000000000000000000, 0.000000000000000000, 0.000000000000000000 ) ) ;
#7970 = VERTEX_POINT ( 'NONE', #29335 ) ;
#7971 = ORIENTED_EDGE ( 'NONE', *, *, #17089, .F. ) ;
#7972 = DIRECTION ( 'NONE',  ( 0.8319571443084845530, -0.5548398958565174954, 1.551805961504353214E-14 ) ) ;
#7973 = DIRECTION ( 'NONE',  ( 0.000000000000000000, 0.000000000000000000, -1.000000000000000000 ) ) ;
#7974 = ORIENTED_EDGE ( 'NONE', *, *, #14348, .T. ) ;
#7975 = CARTESIAN_POINT ( 'NONE',  ( 212.5000000000000000, 0.000000000000000000, 7.500000000000000000 ) ) ;
#7976 = EDGE_CURVE ( 'NONE', #18566, #13940, #10816, .T. ) ;
#7977 = FILL_AREA_STYLE_COLOUR ( '', #14705 ) ;
#7978 = CARTESIAN_POINT ( 'NONE',  ( -20.00000000000004619, -145.0000000000000000, -162.9999999999999432 ) ) ;
#7979 = CARTESIAN_POINT ( 'NONE',  ( -110.0447977791740897, -0.8621751556914719616, 7.452240479933210260 ) ) ;
#7980 = CONTEXT_DEPENDENT_SHAPE_REPRESENTATION ( #28973, #28222 ) ;
#7981 = ORIENTED_EDGE ( 'NONE', *, *, #2919, .F. ) ;
#7982 = AXIS2_PLACEMENT_3D ( 'NONE', #19006, #123, #5972 ) ;
#7983 = EDGE_CURVE ( 'NONE', #21957, #7154, #4928, .T. ) ;
#7984 = DIRECTION ( 'NONE',  ( 1.000000000000000000, 0.000000000000000000, 0.000000000000000000 ) ) ;
#7985 = EDGE_CURVE ( 'NONE', #11635, #19542, #33569, .T. ) ;
#7986 = VECTOR ( 'NONE', #19563, 1000.000000000000000 ) ;
#7988 = DIRECTION ( 'NONE',  ( 1.232595164407830946E-32, 3.421138828918010427E-49, -1.000000000000000000 ) ) ;
#7987 = FACE_OUTER_BOUND ( 'NONE', #15622, .T. ) ;
#7989 = ORIENTED_EDGE ( 'NONE', *, *, #7292, .T. ) ;
#7990 = EDGE_LOOP ( 'NONE', ( #18821, #21984, #19873, #21528, #24648, #23471, #22361, #1913 ) ) ;
#7991 = ADVANCED_FACE ( 'NONE', ( #33220, #22372 ), #22557, .T. ) ;
#7992 = EDGE_CURVE ( 'NONE', #7619, #17138, #3666, .T. ) ;
#7993 = DIRECTION ( 'NONE',  ( -0.2149704402110243773, -0.9766205557100865464, -0.000000000000000000 ) ) ;
#7994 = ORIENTED_EDGE ( 'NONE', *, *, #25214, .T. ) ;
#7995 = CARTESIAN_POINT ( 'NONE',  ( 0.000000000000000000, 33.69708579775584667, 49.43553178847298568 ) ) ;
#7996 = ADVANCED_FACE ( 'NONE', ( #25381 ), #30563, .F. ) ;
#7997 = CARTESIAN_POINT ( 'NONE',  ( 31.83311414508816029, -6.771795677801490498, 49.43553178847298568 ) ) ;
#7998 = ORIENTED_EDGE ( 'NONE', *, *, #5079, .F. ) ;
#7999 = ORIENTED_EDGE ( 'NONE', *, *, #17296, .F. ) ;
#8000 = DIRECTION ( 'NONE',  ( -0.000000000000000000, 1.000000000000000000, -0.000000000000000000 ) ) ;
#8001 = VECTOR ( 'NONE', #10017, 1000.000000000000227 ) ;
#8002 =( GEOMETRIC_REPRESENTATION_CONTEXT ( 3 ) GLOBAL_UNCERTAINTY_ASSIGNED_CONTEXT ( ( #14296 ) ) GLOBAL_UNIT_ASSIGNED_CONTEXT ( ( #32654, #8279, #18802 ) ) REPRESENTATION_CONTEXT ( 'NONE', 'WORKASPACE' ) );
#8004 = CARTESIAN_POINT ( 'NONE',  ( 0.1387913946425842759, -13.01149508916977204, -4.463429423125060858 ) ) ;
#8003 = AXIS2_PLACEMENT_3D ( 'NONE', #10952, #5589, #29819 ) ;
#8005 = ORIENTED_EDGE ( 'NONE', *, *, #24601, .T. ) ;
#8006 = CARTESIAN_POINT ( 'NONE',  ( -15.99999999999998579, -32.99999999999997158, -154.9999999999999716 ) ) ;
#8007 = CYLINDRICAL_SURFACE ( 'NONE', #29632, 3.999999999999976019 ) ;
#8008 = EDGE_CURVE ( 'NONE', #2489, #32312, #30380, .T. ) ;
#8009 = DIRECTION ( 'NONE',  ( 1.000000000000000000, 0.000000000000000000, 0.000000000000000000 ) ) ;
#8010 = LINE ( 'NONE', #18720, #4307 ) ;
#8011 = DIRECTION ( 'NONE',  ( 0.000000000000000000, -1.000000000000000000, -1.836970198721029934E-16 ) ) ;
#8012 = LINE ( 'NONE', #16579, #30958 ) ;
#8013 = AXIS2_PLACEMENT_3D ( 'NONE', #32812, #26774, #10596 ) ;
#8014 = PLANE ( 'NONE',  #20092 ) ;
#8015 = AXIS2_PLACEMENT_3D ( 'NONE', #16865, #33556, #22890 ) ;
#8016 = ORIENTED_EDGE ( 'NONE', *, *, #7976, .T. ) ;
#8017 = CARTESIAN_POINT ( 'NONE',  ( 145.0000000000000568, -12.50000000000001066, 1.224646799147353217E-14 ) ) ;
#8018 = VERTEX_POINT ( 'NONE', #22733 ) ;
#8019 = ORIENTED_EDGE ( 'NONE', *, *, #1570, .F. ) ;
#8020 = VECTOR ( 'NONE', #16216, 1000.000000000000000 ) ;
#8021 = CARTESIAN_POINT ( 'NONE',  ( 100.0684259921083452, 2.939425563888521609, 6.902236325305502795 ) ) ;
#8022 = APPLICATION_PROTOCOL_DEFINITION ( 'draft international standard', 'automotive_design', 1998, #5985 ) ;
#8023 = CIRCLE ( 'NONE', #2917, 9.999999999999998224 ) ;
#8024 = ORIENTED_EDGE ( 'NONE', *, *, #4096, .T. ) ;
#8025 = AXIS2_PLACEMENT_3D ( 'NONE', #16850, #27675, #11677 ) ;
#8026 = CIRCLE ( 'NONE', #22831, 22.50000000000000355 ) ;
#8027 = LINE ( 'NONE', #32936, #20211 ) ;
#8028 = CARTESIAN_POINT ( 'NONE',  ( -12.00000000000001066, 134.9999999999998863, 162.9999999999999716 ) ) ;
#8029 = ITEM_DEFINED_TRANSFORMATION ( 'NONE', 'NONE', #10445,  #28566 ) ;
#8030 = CARTESIAN_POINT ( 'NONE',  ( 2.789999999999999147, -17.95514392185398833, -25.38201125280375692 ) ) ;
#8031 = ORIENTED_EDGE ( 'NONE', *, *, #24497, .F. ) ;
#8032 = ORIENTED_EDGE ( 'NONE', *, *, #3993, .F. ) ;
#8033 = ADVANCED_FACE ( 'NONE', ( #27877 ), #11348, .T. ) ;
#8034 = EDGE_CURVE ( 'NONE', #29789, #20441, #1016, .T. ) ;
#8035 = LINE ( 'NONE', #5176, #943 ) ;
#8036 = DIRECTION ( 'NONE',  ( 0.000000000000000000, 0.000000000000000000, -1.000000000000000000 ) ) ;
#8037 = DIRECTION ( 'NONE',  ( -1.000000000000000000, -0.000000000000000000, -0.000000000000000000 ) ) ;
#8038 = DIRECTION ( 'NONE',  ( -1.000000000000000000, 0.000000000000000000, 0.000000000000000000 ) ) ;
#8039 = DIRECTION ( 'NONE',  ( -1.000000000000000000, -0.000000000000000000, -0.000000000000000000 ) ) ;
#8040 = ORIENTED_EDGE ( 'NONE', *, *, #6772, .F. ) ;
#8041 = VECTOR ( 'NONE', #9415, 1000.000000000000000 ) ;
#8042 = FACE_OUTER_BOUND ( 'NONE', #20726, .T. ) ;
#8043 = CARTESIAN_POINT ( 'NONE',  ( 11.99999999999999645, 136.9999999999999716, 155.0000000000000000 ) ) ;
#8044 = DIRECTION ( 'NONE',  ( 0.000000000000000000, -1.000000000000000000, -0.000000000000000000 ) ) ;
#8045 = CARTESIAN_POINT ( 'NONE',  ( -20.00000000000007461, 136.9999999999999432, 162.9999999999999716 ) ) ;
#8046 = EDGE_CURVE ( 'NONE', #28825, #24229, #661, .T. ) ;
#8047 = DIRECTION ( 'NONE',  ( 1.000000000000000000, 3.040835319149746528E-31, 1.232595164407830946E-32 ) ) ;
#8050 = DIRECTION ( 'NONE',  ( 0.000000000000000000, 0.000000000000000000, -1.000000000000000000 ) ) ;
#8049 = DIRECTION ( 'NONE',  ( 0.000000000000000000, -0.7071067811865489050, -0.7071067811865462405 ) ) ;
#8048 = AXIS2_PLACEMENT_3D ( 'NONE', #26532, #18892, #23859 ) ;
#8051 = VECTOR ( 'NONE', #20107, 1000.000000000000114 ) ;
#8052 = AXIS2_PLACEMENT_3D ( 'NONE', #4538, #29122, #12942 ) ;
#8053 = DIRECTION ( 'NONE',  ( -0.000000000000000000, 1.000000000000000000, -0.000000000000000000 ) ) ;
#8055 = ORIENTED_EDGE ( 'NONE', *, *, #15598, .F. ) ;
#8054 = AXIS2_PLACEMENT_3D ( 'NONE', #15112, #6726, #1575 ) ;
#8056 = LINE ( 'NONE', #2542, #25843 ) ;
#8058 = CARTESIAN_POINT ( 'NONE',  ( 110.6566244370989551, -0.9828571727418841109, -7.437816238889399578 ) ) ;
#8057 = DIRECTION ( 'NONE',  ( 0.000000000000000000, 0.000000000000000000, 1.000000000000000000 ) ) ;
#8059 = EDGE_CURVE ( 'NONE', #31695, #27282, #17053, .T. ) ;
#8060 = EDGE_CURVE ( 'NONE', #4867, #10934, #945, .T. ) ;
#8061 = ADVANCED_FACE ( 'NONE', ( #5980 ), #27346, .T. ) ;
#8062 = VERTEX_POINT ( 'NONE', #2962 ) ;
#8063 =( LENGTH_UNIT ( ) NAMED_UNIT ( * ) SI_UNIT ( .MILLI., .METRE. ) );
#8064 = EDGE_CURVE ( 'NONE', #2517, #2454, #3491, .T. ) ;
#8065 = ORIENTED_EDGE ( 'NONE', *, *, #11305, .T. ) ;
#8066 = CIRCLE ( 'NONE', #12634, 9.999999999999998224 ) ;
#8067 =( REPRESENTATION_RELATIONSHIP ('NONE','NONE', #23037, #28231 ) REPRESENTATION_RELATIONSHIP_WITH_TRANSFORMATION ( #14492 )SHAPE_REPRESENTATION_RELATIONSHIP( ) );
#8068 = VERTEX_POINT ( 'NONE', #30731 ) ;
#8069 = FACE_BOUND ( 'NONE', #20564, .T. ) ;
#8070 = ORIENTED_EDGE ( 'NONE', *, *, #14689, .F. ) ;
#8071 = ORIENTED_EDGE ( 'NONE', *, *, #21380, .T. ) ;
#8072 = DIRECTION ( 'NONE',  ( 0.000000000000000000, 0.000000000000000000, 1.000000000000000000 ) ) ;
#8073 =( GEOMETRIC_REPRESENTATION_CONTEXT ( 3 ) GLOBAL_UNCERTAINTY_ASSIGNED_CONTEXT ( ( #14954 ) ) GLOBAL_UNIT_ASSIGNED_CONTEXT ( ( #11939, #17989, #14616 ) ) REPRESENTATION_CONTEXT ( 'NONE', 'WORKASPACE' ) );
#8074 = ADVANCED_FACE ( 'NONE', ( #19714 ), #33034, .T. ) ;
#8075 = CARTESIAN_POINT ( 'NONE',  ( -45.00000000000000000, 42.49491490430484220, 36.69637551990492597 ) ) ;
#8076 = AXIS2_PLACEMENT_3D ( 'NONE', #34990, #32296, #29634 ) ;
#8077 = DIRECTION ( 'NONE',  ( 0.000000000000000000, 0.000000000000000000, 1.000000000000000000 ) ) ;
#8078 = ORIENTED_EDGE ( 'NONE', *, *, #5715, .T. ) ;
#8079 = ORIENTED_EDGE ( 'NONE', *, *, #4051, .T. ) ;
#8080 = VECTOR ( 'NONE', #26833, 1000.000000000000000 ) ;
#8081 = DIRECTION ( 'NONE',  ( 0.000000000000000000, 1.000000000000000000, 0.000000000000000000 ) ) ;
#8082 = DIRECTION ( 'NONE',  ( 0.000000000000000000, 0.000000000000000000, 1.000000000000000000 ) ) ;
#8083 = CARTESIAN_POINT ( 'NONE',  ( 110.7380848894536598, 7.027143731242819742E-16, -12.50000000000000000 ) ) ;
#8084 = DIRECTION ( 'NONE',  ( 0.000000000000000000, -0.5877852522924686962, -0.8090169943749506709 ) ) ;
#8085 = ORIENTED_EDGE ( 'NONE', *, *, #26759, .F. ) ;
#8086 = DIRECTION ( 'NONE',  ( 1.000000000000000000, 0.000000000000000000, 0.000000000000000000 ) ) ;
#8087 = CARTESIAN_POINT ( 'NONE',  ( -500.0000000000000000, -113.0000000000000000, 194.9999999999999716 ) ) ;
#8088 = ORIENTED_EDGE ( 'NONE', *, *, #17426, .T. ) ;
#8089 = DIRECTION ( 'NONE',  ( -1.000000000000000000, -0.000000000000000000, -0.000000000000000000 ) ) ;
#8090 = CARTESIAN_POINT ( 'NONE',  ( -8.427639665100776541E-14, -7.838364976555423524, -29.64395146466218733 ) ) ;
#8091 = DIRECTION ( 'NONE',  ( 0.000000000000000000, 1.224646799147353207E-16, -1.000000000000000000 ) ) ;
#8092 = CARTESIAN_POINT ( 'NONE',  ( 2.265105727189284046, 7.015288891537251992, -32.63428354963176048 ) ) ;
#8093 = ORIENTED_EDGE ( 'NONE', *, *, #7487, .T. ) ;
#8094 = PLANE ( 'NONE',  #21242 ) ;
#8095 = ORIENTED_EDGE ( 'NONE', *, *, #9484, .F. ) ;
#8097 = CARTESIAN_POINT ( 'NONE',  ( -442.0000000000000000, -109.0000000000000142, 155.0000000000000000 ) ) ;
#8096 = CARTESIAN_POINT ( 'NONE',  ( 0.02407890056655825201, -3.506335382740311868, -30.89238256715869468 ) ) ;
#8098 = LINE ( 'NONE', #18441, #26185 ) ;
#8099 = EDGE_CURVE ( 'NONE', #726, #27282, #23601, .T. ) ;
#8100 = AXIS2_PLACEMENT_3D ( 'NONE', #4501, #10215, #17430 ) ;
#8101 = EDGE_CURVE ( 'NONE', #23708, #12488, #31623, .T. ) ;
#8103 = EDGE_LOOP ( 'NONE', ( #23984, #18516, #16069, #24046, #5580, #1763 ) ) ;
#8102 = VECTOR ( 'NONE', #33620, 1000.000000000000000 ) ;
#8104 = CIRCLE ( 'NONE', #33692, 2.033421858999711951 ) ;
#8105 = AXIS2_PLACEMENT_3D ( 'NONE', #8316, #24326, #19017 ) ;
#8106 = CARTESIAN_POINT ( 'NONE',  ( 1.749999999999999778, 0.000000000000000000, 0.000000000000000000 ) ) ;
#8107 = CARTESIAN_POINT ( 'NONE',  ( 2.719051668539516076, -31.01658195443389943, -6.517894193013122006 ) ) ;
#8108 = ORIENTED_EDGE ( 'NONE', *, *, #34271, .F. ) ;
#8109 = ORIENTED_EDGE ( 'NONE', *, *, #2367, .F. ) ;
#8110 = LINE ( 'NONE', #19168, #11245 ) ;
#8111 = CARTESIAN_POINT ( 'NONE',  ( -108.1240957144767521, 4.062957613056745743, 6.307943406627045668 ) ) ;
#8112 = ORIENTED_EDGE ( 'NONE', *, *, #34759, .F. ) ;
#8113 = ORIENTED_EDGE ( 'NONE', *, *, #23673, .T. ) ;
#8114 = LINE ( 'NONE', #5086, #4773 ) ;
#8115 = CARTESIAN_POINT ( 'NONE',  ( 0.1149164202474876467, -10.37169118567827653, -9.035703905990969176 ) ) ;
#8116 = CARTESIAN_POINT ( 'NONE',  ( 22.89764159710611224, 13.56412600238610366, -77.50000000000000000 ) ) ;
#8117 = CARTESIAN_POINT ( 'NONE',  ( 11.99999999999999645, -145.0000000000000000, -154.9999999999999716 ) ) ;
#8118 = ORIENTED_EDGE ( 'NONE', *, *, #27834, .T. ) ;
#8119 = ORIENTED_EDGE ( 'NONE', *, *, #19257, .F. ) ;
#8120 = CARTESIAN_POINT ( 'NONE',  ( 11.99999999999999645, 140.9999999999999716, 155.0000000000000000 ) ) ;
#8121 = DIRECTION ( 'NONE',  ( 1.000000000000000000, 0.000000000000000000, 0.000000000000000000 ) ) ;
#8122 = DIRECTION ( 'NONE',  ( -1.000000000000000000, 0.000000000000000000, -5.546364386991661285E-52 ) ) ;
#8123 = DIRECTION ( 'NONE',  ( -1.000000000000000000, 0.000000000000000000, -0.000000000000000000 ) ) ;
#8124 =( GEOMETRIC_REPRESENTATION_CONTEXT ( 3 ) GLOBAL_UNCERTAINTY_ASSIGNED_CONTEXT ( ( #10711 ) ) GLOBAL_UNIT_ASSIGNED_CONTEXT ( ( #6790, #17854, #6960 ) ) REPRESENTATION_CONTEXT ( 'NONE', 'WORKASPACE' ) );
#8125 = DIRECTION ( 'NONE',  ( -0.000000000000000000, 0.000000000000000000, -1.000000000000000000 ) ) ;
#8126 = DIRECTION ( 'NONE',  ( 1.000000000000000000, -0.000000000000000000, -0.000000000000000000 ) ) ;
#8127 = AXIS2_PLACEMENT_3D ( 'NONE', #4013, #28597, #12245 ) ;
#8128 = MECHANICAL_DESIGN_GEOMETRIC_PRESENTATION_REPRESENTATION (  '', ( #23398 ), #17812 ) ;
#8129 = FACE_OUTER_BOUND ( 'NONE', #19152, .T. ) ;
#8130 = CIRCLE ( 'NONE', #29733, 7.999999999999979572 ) ;
#8131 = LINE ( 'NONE', #19011, #20414 ) ;
#8132 = VERTEX_POINT ( 'NONE', #3321 ) ;
#8133 = CARTESIAN_POINT ( 'NONE',  ( -12.00000000000001066, -109.0000000000000142, 155.0000000000000000 ) ) ;
#8134 = CARTESIAN_POINT ( 'NONE',  ( -418.0000000000000000, -112.9999999999999858, -155.0000000000000000 ) ) ;
#8135 = CARTESIAN_POINT ( 'NONE',  ( 2.790000000000082192, -0.2199561701061230334, 30.66195251245370201 ) ) ;
#8136 = ORIENTED_EDGE ( 'NONE', *, *, #13110, .T. ) ;
#8137 = DIRECTION ( 'NONE',  ( 0.000000000000000000, 5.145227585319922065E-49, 1.000000000000000000 ) ) ;
#8138 = ORIENTED_EDGE ( 'NONE', *, *, #33019, .F. ) ;
#8139 = CARTESIAN_POINT ( 'NONE',  ( -109.4325559004959416, 2.574279381791157562, -12.23535145228420085 ) ) ;
#8140 = EDGE_CURVE ( 'NONE', #6590, #12207, #8489, .T. ) ;
#8141 = DIRECTION ( 'NONE',  ( 0.000000000000000000, -1.000000000000000000, -1.224646799147353207E-16 ) ) ;
#8142 = EDGE_CURVE ( 'NONE', #18475, #33757, #34398, .T. ) ;
#8143 = ORIENTED_EDGE ( 'NONE', *, *, #3119, .F. ) ;
#8144 = B_SPLINE_CURVE_WITH_KNOTS ( 'NONE', 3,
 ( #5833, #27736, #16728, #27910 ),
 .UNSPECIFIED., .F., .F.,
 ( 4, 4 ),
 ( 0.005298437004852360292, 0.005985304466813747698 ),
 .UNSPECIFIED. ) ;
#8145 = CARTESIAN_POINT ( 'NONE',  ( -410.0000000000000568, 105.0000000000000142, 162.9999999999999716 ) ) ;
#8146 = DIRECTION ( 'NONE',  ( 0.000000000000000000, 0.000000000000000000, 1.000000000000000000 ) ) ;
#8147 = LINE ( 'NONE', #22743, #33664 ) ;
#8148 = ORIENTED_EDGE ( 'NONE', *, *, #30430, .F. ) ;
#8149 = AXIS2_PLACEMENT_3D ( 'NONE', #24871, #22213, #33056 ) ;
#8150 = ORIENTED_EDGE ( 'NONE', *, *, #26237, .T. ) ;
#8151 = VECTOR ( 'NONE', #29639, 1000.000000000000000 ) ;
#8152 = DIRECTION ( 'NONE',  ( -7.893605728314050488E-14, 1.618803117314786135E-15, 0.9999999999999998890 ) ) ;
#8153 = AXIS2_PLACEMENT_3D ( 'NONE', #17467, #33452, #27756 ) ;
#8154 = DIRECTION ( 'NONE',  ( -0.000000000000000000, 1.000000000000000000, 3.017235169886638201E-16 ) ) ;
#8155 = ORIENTED_EDGE ( 'NONE', *, *, #32256, .F. ) ;
#8156 = LINE ( 'NONE', #11012, #33402 ) ;
#8157 = CARTESIAN_POINT ( 'NONE',  ( -15.99999999999998579, 75.55999999999990280, -172.9900000000000091 ) ) ;
#8158 = CARTESIAN_POINT ( 'NONE',  ( -105.6898066376448497, -5.079998963781828358, 5.518357322521167951 ) ) ;
#8159 = ORIENTED_EDGE ( 'NONE', *, *, #12607, .T. ) ;
#8160 = ORIENTED_EDGE ( 'NONE', *, *, #2272, .F. ) ;
#8161 = CARTESIAN_POINT ( 'NONE',  ( 11.99999999999995559, -145.0000000000000000, -162.9999999999999432 ) ) ;
#8162 = AXIS2_PLACEMENT_3D ( 'NONE', #16370, #27200, #18690 ) ;
#8164 = LINE ( 'NONE', #35067, #21534 ) ;
#8163 = DIRECTION ( 'NONE',  ( 0.7621620551276367950, 0.6473862847818272481, 0.000000000000000000 ) ) ;
#8165 = ORIENTED_EDGE ( 'NONE', *, *, #5681, .F. ) ;
#8166 = VERTEX_POINT ( 'NONE', #3837 ) ;
#8167 = CARTESIAN_POINT ( 'NONE',  ( 2.033800798445904334, -29.97203090897430755, 15.87187733270971357 ) ) ;
#8168 = ORIENTED_EDGE ( 'NONE', *, *, #29090, .F. ) ;
#8169 = DIRECTION ( 'NONE',  ( -1.000000000000000000, 0.000000000000000000, -0.000000000000000000 ) ) ;
#8170 = CARTESIAN_POINT ( 'NONE',  ( -499.9999999999999432, 136.9999999999999432, 162.9999999999999716 ) ) ;
#8171 = EDGE_LOOP ( 'NONE', ( #15773, #784, #20770, #5640, #6688, #856, #27053, #21822 ) ) ;
#8172 = AXIS2_PLACEMENT_3D ( 'NONE', #31963, #10258, #4544 ) ;
#8173 = ORIENTED_EDGE ( 'NONE', *, *, #11271, .T. ) ;
#8174 = CYLINDRICAL_SURFACE ( 'NONE', #16404, 3.999999999999989786 ) ;
#8175 = VECTOR ( 'NONE', #24949, 1000.000000000000114 ) ;
#8176 = CIRCLE ( 'NONE', #795, 2.525000000000000355 ) ;
#8177 = PRODUCT_DEFINITION_SHAPE ( 'NONE', 'NONE',  #35204 ) ;
#8178 = FACE_OUTER_BOUND ( 'NONE', #31226, .T. ) ;
#8179 = VERTEX_POINT ( 'NONE', #17751 ) ;
#8180 = CYLINDRICAL_SURFACE ( 'NONE', #19774, 3.999999999999976019 ) ;
#8181 = CARTESIAN_POINT ( 'NONE',  ( -20.00000000000004619, 112.9999999999999574, -154.9999999999999716 ) ) ;
#8182 = ADVANCED_FACE ( 'NONE', ( #9712 ), #4527, .T. ) ;
#8183 = CARTESIAN_POINT ( 'NONE',  ( 145.0000000000000568, -174.9263417920030577, -39.67942821175577706 ) ) ;
#8184 = LINE ( 'NONE', #32224, #13991 ) ;
#8185 = CYLINDRICAL_SURFACE ( 'NONE', #34174, 34.41491905851385269 ) ;
#8186 = CARTESIAN_POINT ( 'NONE',  ( -20.63749999999999929, 0.000000000000000000, 0.000000000000000000 ) ) ;
#8188 = ADVANCED_FACE ( 'NONE', ( #31428 ), #12407, .T. ) ;
#8187 = CARTESIAN_POINT ( 'NONE',  ( 0.000000000000000000, 0.000000000000000000, -0.7500000000000000000 ) ) ;
#8189 = VECTOR ( 'NONE', #2421, 1000.000000000000000 ) ;
#8190 = ORIENTED_EDGE ( 'NONE', *, *, #25260, .T. ) ;
#8191 = EDGE_CURVE ( 'NONE', #23670, #26414, #11050, .T. ) ;
#8192 = CARTESIAN_POINT ( 'NONE',  ( -20.00000000000004619, -105.0000000000000000, -187.0000000000000000 ) ) ;
#8193 = CARTESIAN_POINT ( 'NONE',  ( 0.000000000000000000, 0.000000000000000000, 0.000000000000000000 ) ) ;
#8194 = VERTEX_POINT ( 'NONE', #31092 ) ;
#8195 = VECTOR ( 'NONE', #17307, 1000.000000000000000 ) ;
#8196 = ORIENTED_EDGE ( 'NONE', *, *, #887, .T. ) ;
#8197 = EDGE_CURVE ( 'NONE', #2635, #1617, #34821, .T. ) ;
#8198 = LINE ( 'NONE', #13669, #15439 ) ;
#8199 = VECTOR ( 'NONE', #12716, 1000.000000000000000 ) ;
#8200 = CARTESIAN_POINT ( 'NONE',  ( 99.47175666340625355, 1.549642152983123244, 7.340597171393927312 ) ) ;
#8201 = PRODUCT_CONTEXT ( 'NONE', #29861, 'mechanical' ) ;
#8202 = VERTEX_POINT ( 'NONE', #4189 ) ;
#8203 = DIRECTION ( 'NONE',  ( 0.000000000000000000, 2.309213040847544338E-50, 1.000000000000000000 ) ) ;
#8204 =( LENGTH_UNIT ( ) NAMED_UNIT ( * ) SI_UNIT ( .MILLI., .METRE. ) );
#8205 = VECTOR ( 'NONE', #61, 1000.000000000000000 ) ;
#8206 = ITEM_DEFINED_TRANSFORMATION ( 'NONE', 'NONE', #11600,  #28566 ) ;
#8207 = LINE ( 'NONE', #29578, #14120 ) ;
#8208 = EDGE_LOOP ( 'NONE', ( #19468, #34217, #3794, #2009 ) ) ;
#8209 = ORIENTED_EDGE ( 'NONE', *, *, #20677, .T. ) ;
#8210 = CARTESIAN_POINT ( 'NONE',  ( -25.07182831876307105, -28.36910952062234870, 68.31122994652405112 ) ) ;
#8211 = CARTESIAN_POINT ( 'NONE',  ( 18.92820323027550344, -115.0000000000000000, -158.9999999999999716 ) ) ;
#8212 = CARTESIAN_POINT ( 'NONE',  ( 0.000000000000000000, 0.000000000000000000, 62.49999999999999289 ) ) ;
#8213 = CARTESIAN_POINT ( 'NONE',  ( 2.789999999999998703, -27.64940622781567470, 13.25307083675137321 ) ) ;
#8214 = CARTESIAN_POINT ( 'NONE',  ( 2.789999999999999147, -25.83993731729781729, -18.77381338200996552 ) ) ;
#8215 = VERTEX_POINT ( 'NONE', #20581 ) ;
#8216 = DIRECTION ( 'NONE',  ( -1.000000000000000000, 0.000000000000000000, 0.000000000000000000 ) ) ;
#8217 = DIRECTION ( 'NONE',  ( -2.154935995002245207E-17, -0.000000000000000000, -1.000000000000000000 ) ) ;
#8218 = VECTOR ( 'NONE', #25137, 1000.000000000000000 ) ;
#8219 = CARTESIAN_POINT ( 'NONE',  ( -8.000000000000000000, 11.79999999999999893, 0.000000000000000000 ) ) ;
#8220 = VECTOR ( 'NONE', #15111, 1000.000000000000000 ) ;
#8221 = DIRECTION ( 'NONE',  ( 0.000000000000000000, 0.000000000000000000, 1.000000000000000000 ) ) ;
#8222 = CARTESIAN_POINT ( 'NONE',  ( 11.99999999999999645, -55.00000000000000711, 162.9999999999999716 ) ) ;
#8223 = ADVANCED_FACE ( 'NONE', ( #10750 ), #21599, .F. ) ;
#8224 = CARTESIAN_POINT ( 'NONE',  ( -12.00000000000001066, 144.9999999999999716, 159.0000000000000000 ) ) ;
#8226 = CARTESIAN_POINT ( 'NONE',  ( -5.210000000000000853, 0.000000000000000000, 0.000000000000000000 ) ) ;
#8225 = LINE ( 'NONE', #26744, #7637 ) ;
#8227 = VECTOR ( 'NONE', #15339, 1000.000000000000000 ) ;
#8228 = CIRCLE ( 'NONE', #32667, 10.00000000000000000 ) ;
#8229 = CARTESIAN_POINT ( 'NONE',  ( 0.000000000000000000, 27.60935207499554522, 12.89090262359660422 ) ) ;
#8230 = EDGE_LOOP ( 'NONE', ( #17213, #14529, #14877, #18329 ) ) ;
#8231 = DIRECTION ( 'NONE',  ( 0.9947866662129278836, -0.05393576583119110562, -0.08654722346309881575 ) ) ;
#8233 = DIRECTION ( 'NONE',  ( -0.000000000000000000, -0.000000000000000000, 1.000000000000000000 ) ) ;
#8232 = CARTESIAN_POINT ( 'NONE',  ( -20.63749999999999929, 0.000000000000000000, 0.000000000000000000 ) ) ;
#8234 = AXIS2_PLACEMENT_3D ( 'NONE', #22398, #8340, #11729 ) ;
#8235 = ADVANCED_FACE ( 'NONE', ( #7033 ), #23595, .F. ) ;
#8236 = ORIENTED_EDGE ( 'NONE', *, *, #3081, .F. ) ;
#8237 = EDGE_CURVE ( 'NONE', #25058, #192, #14735, .T. ) ;
#8238 = EDGE_CURVE ( 'NONE', #1340, #7081, #22547, .T. ) ;
#8239 = CARTESIAN_POINT ( 'NONE',  ( 0.000000000000000000, -11.13185981125894486, 28.36429779836949194 ) ) ;
#8240 = ORIENTED_EDGE ( 'NONE', *, *, #27319, .F. ) ;
#8241 = VECTOR ( 'NONE', #12172, 1000.000000000000000 ) ;
#8242 = ORIENTED_EDGE ( 'NONE', *, *, #7992, .F. ) ;
#8243 = CARTESIAN_POINT ( 'NONE',  ( -20.00000000000007461, 136.9999999999999432, -155.0000000000000000 ) ) ;
#8244 = ORIENTED_EDGE ( 'NONE', *, *, #32525, .T. ) ;
#8245 = ORIENTED_EDGE ( 'NONE', *, *, #10275, .T. ) ;
#8246 = CARTESIAN_POINT ( 'NONE',  ( -499.9999999999999432, 112.9999999999999574, -194.9999999999999716 ) ) ;
#8247 = VECTOR ( 'NONE', #20963, 1000.000000000000000 ) ;
#8248 = EDGE_CURVE ( 'NONE', #21282, #292, #30137, .T. ) ;
#8249 = ADVANCED_FACE ( 'NONE', ( #24077 ), #26934, .T. ) ;
#8250 = DIRECTION ( 'NONE',  ( 0.000000000000000000, 0.000000000000000000, 1.000000000000000000 ) ) ;
#8251 = CARTESIAN_POINT ( 'NONE',  ( 1.039999999999999591, -30.28730148581173864, 16.34215476954022606 ) ) ;
#8252 = ORIENTED_EDGE ( 'NONE', *, *, #19984, .T. ) ;
#8253 = ORIENTED_EDGE ( 'NONE', *, *, #2365, .F. ) ;
#8254 = AXIS2_PLACEMENT_3D ( 'NONE', #5637, #8326, #1197 ) ;
#8255 = FACE_OUTER_BOUND ( 'NONE', #9278, .T. ) ;
#8256 = CIRCLE ( 'NONE', #21907, 30.47050528711512030 ) ;
#8257 = CARTESIAN_POINT ( 'NONE',  ( 2.789999999999999147, 9.869977788040968036, 30.37666815053940539 ) ) ;
#8258 = CIRCLE ( 'NONE', #28165, 30.47050528711511674 ) ;
#8259 = EDGE_CURVE ( 'NONE', #7715, #33356, #27076, .T. ) ;
#8260 = CARTESIAN_POINT ( 'NONE',  ( 99.26191511054632599, -6.978196330887525654E-16, -12.50000000000000000 ) ) ;
#8261 = CARTESIAN_POINT ( 'NONE',  ( 2.789999999999999147, -30.46391896562411716, 6.211548095912460710 ) ) ;
#8262 = ORIENTED_EDGE ( 'NONE', *, *, #17870, .T. ) ;
#8263 = EDGE_CURVE ( 'NONE', #4626, #24189, #20755, .T. ) ;
#8264 = LINE ( 'NONE', #30148, #6573 ) ;
#8265 = ADVANCED_FACE ( 'NONE', ( #14903 ), #25558, .F. ) ;
#8266 = CARTESIAN_POINT ( 'NONE',  ( -410.0000000000000568, -125.0000000000000000, 187.0000000000000000 ) ) ;
#8267 = VERTEX_POINT ( 'NONE', #17414 ) ;
#8268 = CARTESIAN_POINT ( 'NONE',  ( -45.00000000000000000, 42.49491490430484220, 36.69637551990492597 ) ) ;
#8269 = ADVANCED_FACE ( 'NONE', ( #28242 ), #20243, .T. ) ;
#8270 = CARTESIAN_POINT ( 'NONE',  ( 2.765921099433442887, -30.46391896562411716, 6.211548095912460710 ) ) ;
#8271 = CARTESIAN_POINT ( 'NONE',  ( 2.765921099433441999, -29.68817180695669578, -9.232883799364548949 ) ) ;
#8272 = DIRECTION ( 'NONE',  ( 0.9075754196709575616, 0.4198891015602635446, 0.000000000000000000 ) ) ;
#8273 = ORIENTED_EDGE ( 'NONE', *, *, #2585, .T. ) ;
#8274 = AXIS2_PLACEMENT_3D ( 'NONE', #20650, #31493, #32680 ) ;
#8275 = DIRECTION ( 'NONE',  ( 0.000000000000000000, 1.000000000000000000, 2.465190328815662439E-32 ) ) ;
#8276 = ORIENTED_EDGE ( 'NONE', *, *, #21307, .F. ) ;
#8277 = CARTESIAN_POINT ( 'NONE',  ( -37.55078559520313064, -4.831299144296464121, 15.81122994652406710 ) ) ;
#8278 = CIRCLE ( 'NONE', #23086, 2.033421858999711951 ) ;
#8279 =( NAMED_UNIT ( * ) PLANE_ANGLE_UNIT ( ) SI_UNIT ( $, .RADIAN. ) );
#8280 = ORIENTED_EDGE ( 'NONE', *, *, #28479, .F. ) ;
#8281 = ADVANCED_FACE ( 'NONE', ( #1365 ), #12238, .F. ) ;
#8282 = EDGE_CURVE ( 'NONE', #9716, #2764, #18269, .T. ) ;
#8283 =( REPRESENTATION_RELATIONSHIP ('NONE','NONE', #23037, #15767 ) REPRESENTATION_RELATIONSHIP_WITH_TRANSFORMATION ( #23114 )SHAPE_REPRESENTATION_RELATIONSHIP( ) );
#8284 = DIRECTION ( 'NONE',  ( -0.4684084406997904848, -0.8835120444460226041, -0.000000000000000000 ) ) ;
#8285 = CARTESIAN_POINT ( 'NONE',  ( -28.00450684652667022, 16.58167570419054471, 68.31122994652405112 ) ) ;
#8286 = AXIS2_PLACEMENT_3D ( 'NONE', #8755, #19637, #31004 ) ;
#8287 = ORIENTED_EDGE ( 'NONE', *, *, #7875, .F. ) ;
#8288 = ORIENTED_EDGE ( 'NONE', *, *, #10815, .T. ) ;
#8289 = ORIENTED_EDGE ( 'NONE', *, *, #27121, .T. ) ;
#8290 = CARTESIAN_POINT ( 'NONE',  ( -20.02113311122488781, 6.201984591278720593, -87.50000000000000000 ) ) ;
#8291 = CARTESIAN_POINT ( 'NONE',  ( -109.4378652105823306, 2.632420417224709652, 7.052679658646592742 ) ) ;
#8292 = VERTEX_POINT ( 'NONE', #21450 ) ;
#8293 = ORIENTED_EDGE ( 'NONE', *, *, #7292, .F. ) ;
#8294 = CARTESIAN_POINT ( 'NONE',  ( 19.99999999999998224, -55.00000000000000711, -154.9999999999999716 ) ) ;
#8295 = LINE ( 'NONE', #21479, #9622 ) ;
#8296 = AXIS2_PLACEMENT_3D ( 'NONE', #3610, #25149, #29974 ) ;
#8297 = DIRECTION ( 'NONE',  ( 0.000000000000000000, 0.000000000000000000, -1.000000000000000000 ) ) ;
#8298 = DIRECTION ( 'NONE',  ( -1.000000000000000000, 0.000000000000000000, 0.000000000000000000 ) ) ;
#8299 = ORIENTED_EDGE ( 'NONE', *, *, #1011, .F. ) ;
#8300 = EDGE_LOOP ( 'NONE', ( #8620, #32439, #30606, #15427 ) ) ;
#8301 = CARTESIAN_POINT ( 'NONE',  ( -20.00000000000001776, -113.0000000000000000, 190.9999999999999716 ) ) ;
#8302 = DIRECTION ( 'NONE',  ( 3.697785493223492838E-32, 1.934419779023891545E-16, -1.000000000000000000 ) ) ;
#8303 = B_SPLINE_CURVE_WITH_KNOTS ( 'NONE', 3,
 ( #33944, #26273, #17764, #31106 ),
 .UNSPECIFIED., .F., .F.,
 ( 4, 4 ),
 ( 0.005298558704933904739, 0.005985424570307885592 ),
 .UNSPECIFIED. ) ;
#8304 = FACE_OUTER_BOUND ( 'NONE', #24607, .T. ) ;
#8305 = AXIS2_PLACEMENT_3D ( 'NONE', #11614, #13655, #2790 ) ;
#8306 = CARTESIAN_POINT ( 'NONE',  ( -7.700000000000000178, 0.000000000000000000, 0.000000000000000000 ) ) ;
#8307 = ADVANCED_FACE ( 'NONE', ( #26783 ), #13616, .T. ) ;
#8308 = EDGE_CURVE ( 'NONE', #3718, #32967, #7377, .T. ) ;
#8309 = DIRECTION ( 'NONE',  ( 1.000000000000000000, 0.000000000000000000, 0.000000000000000000 ) ) ;
#8310 = CARTESIAN_POINT ( 'NONE',  ( 119.9999999999998295, 0.000000000000000000, 0.000000000000000000 ) ) ;
#8311 = DIRECTION ( 'NONE',  ( 0.000000000000000000, 1.836970198721029441E-16, -1.000000000000000000 ) ) ;
#8312 = ORIENTED_EDGE ( 'NONE', *, *, #2961, .F. ) ;
#8313 = VECTOR ( 'NONE', #4711, 1000.000000000000000 ) ;
#8314 = CARTESIAN_POINT ( 'NONE',  ( -20.02113311122478123, 14.09580098603202458, -67.50000000000000000 ) ) ;
#8315 = FACE_OUTER_BOUND ( 'NONE', #29881, .T. ) ;
#8316 = CARTESIAN_POINT ( 'NONE',  ( 11.99999999999999645, -115.0000000000000000, 162.9999999999999716 ) ) ;
#8317 = VERTEX_POINT ( 'NONE', #10415 ) ;
#8318 = ADVANCED_FACE ( 'NONE', ( #29811 ), #15778, .T. ) ;
#8319 = DIRECTION ( 'NONE',  ( 1.000000000000000000, -0.000000000000000000, -0.000000000000000000 ) ) ;
#8320 = ORIENTED_EDGE ( 'NONE', *, *, #17017, .T. ) ;
#8321 = CARTESIAN_POINT ( 'NONE',  ( 0.6763010051031078662, -1.505030548027689319, 3.180000000000000160 ) ) ;
#8322 = DIRECTION ( 'NONE',  ( 0.000000000000000000, -1.000000000000000000, -0.000000000000000000 ) ) ;
#8323 = AXIS2_PLACEMENT_3D ( 'NONE', #25636, #12136, #25816 ) ;
#8324 = ORIENTED_EDGE ( 'NONE', *, *, #12466, .T. ) ;
#8325 = DIRECTION ( 'NONE',  ( 1.000000000000000000, -0.000000000000000000, -0.000000000000000000 ) ) ;
#8326 = DIRECTION ( 'NONE',  ( 0.000000000000000000, -1.000000000000000000, -1.836970198721029934E-16 ) ) ;
#8327 = LINE ( 'NONE', #16712, #5214 ) ;
#8328 = VECTOR ( 'NONE', #23417, 1000.000000000000000 ) ;
#8329 = ORIENTED_EDGE ( 'NONE', *, *, #8387, .T. ) ;
#8330 = EDGE_LOOP ( 'NONE', ( #23074, #30747, #21901, #23065, #10414, #10256 ) ) ;
#8331 = DIRECTION ( 'NONE',  ( 0.1063910735369155841, -0.9943243633099125844, -3.335902418025060287E-15 ) ) ;
#8332 = B_SPLINE_CURVE_WITH_KNOTS ( 'NONE', 3,
 ( #24889, #24362, #1404, #17452, #14941, #3710 ),
 .UNSPECIFIED., .F., .F.,
 ( 4, 2, 4 ),
 ( 4.404817130298605098E-07, 0.001874269701320913691, 0.003748098920928797251 ),
 .UNSPECIFIED. ) ;
#8333 = CARTESIAN_POINT ( 'NONE',  ( -499.9999999999999432, 104.9999999999999858, 187.0000000000000000 ) ) ;
#8334 = EDGE_CURVE ( 'NONE', #4421, #3207, #5412, .T. ) ;
#8335 = VERTEX_POINT ( 'NONE', #21270 ) ;
#8336 = AXIS2_PLACEMENT_3D ( 'NONE', #28207, #25351, #22703 ) ;
#8337 = CARTESIAN_POINT ( 'NONE',  ( 55.00000000000000711, 0.000000000000000000, 0.000000000000000000 ) ) ;
#8338 = DIRECTION ( 'NONE',  ( 0.000000000000000000, 0.000000000000000000, 1.000000000000000000 ) ) ;
#8339 = B_SPLINE_CURVE_WITH_KNOTS ( 'NONE', 3,
 ( #1093, #11964, #22808, #20147, #26517, #26695 ),
 .UNSPECIFIED., .F., .F.,
 ( 4, 2, 4 ),
 ( 4.404817006251796231E-07, 0.001874269609036412904, 0.003748098736372200684 ),
 .UNSPECIFIED. ) ;
#8340 = DIRECTION ( 'NONE',  ( -1.000000000000000000, 0.000000000000000000, 1.232595164407831220E-32 ) ) ;
#8341 = CARTESIAN_POINT ( 'NONE',  ( -101.2785545903827824, -3.512874579320472535, 6.627714125729965211 ) ) ;
#8342 = ITEM_DEFINED_TRANSFORMATION ( 'NONE', 'NONE', #14405,  #28566 ) ;
#8343 = EDGE_LOOP ( 'NONE', ( #19380, #18008, #8136, #20464 ) ) ;
#8344 = ORIENTED_EDGE ( 'NONE', *, *, #22707, .F. ) ;
#8345 = ORIENTED_EDGE ( 'NONE', *, *, #15652, .T. ) ;
#8346 = DIRECTION ( 'NONE',  ( -3.469446951953832974E-18, -1.000000000000000000, -7.888609052210116302E-31 ) ) ;
#8347 = AXIS2_PLACEMENT_3D ( 'NONE', #8219, #19279, #30114 ) ;
#8348 = EDGE_CURVE ( 'NONE', #15373, #32238, #27133, .T. ) ;
#8349 = CARTESIAN_POINT ( 'NONE',  ( 2.033589665476111197, -29.97226545381508345, -15.87222719455825093 ) ) ;
#8350 = EDGE_CURVE ( 'NONE', #29522, #33375, #4699, .T. ) ;
#8351 = VECTOR ( 'NONE', #10146, 1000.000000000000114 ) ;
#8352 = EDGE_CURVE ( 'NONE', #22453, #21269, #15747, .T. ) ;
#8353 = CARTESIAN_POINT ( 'NONE',  ( -347.0000000000000000, 134.9999999999999716, 126.0000000000000000 ) ) ;
#8354 = ORIENTED_EDGE ( 'NONE', *, *, #10623, .T. ) ;
#8355 = VERTEX_POINT ( 'NONE', #21622 ) ;
#8356 = CARTESIAN_POINT ( 'NONE',  ( 0.02407890056655608360, 4.286445725888036407, 30.79383171238946204 ) ) ;
#8357 = EDGE_LOOP ( 'NONE', ( #886, #19574, #21910, #11985 ) ) ;
#8358 = CARTESIAN_POINT ( 'NONE',  ( -9.978866888775632660, -3.725253662474303784, -67.50000000000000000 ) ) ;
#8359 = CARTESIAN_POINT ( 'NONE',  ( 5.021133111224265200, -13.65249191622732461, -87.50000000000000000 ) ) ;
#8360 = ORIENTED_EDGE ( 'NONE', *, *, #16093, .F. ) ;
#8361 = ORIENTED_EDGE ( 'NONE', *, *, #31835, .T. ) ;
#8362 = DIRECTION ( 'NONE',  ( 0.000000000000000000, 0.000000000000000000, -1.000000000000000000 ) ) ;
#8363 = DIRECTION ( 'NONE',  ( 0.000000000000000000, 0.000000000000000000, 1.000000000000000000 ) ) ;
#8364 = ORIENTED_EDGE ( 'NONE', *, *, #12404, .F. ) ;
#8365 = DIRECTION ( 'NONE',  ( 0.000000000000000000, 1.000000000000000000, 1.836970198721029688E-16 ) ) ;
#8366 = DIRECTION ( 'NONE',  ( 1.000000000000000000, 0.000000000000000000, 0.000000000000000000 ) ) ;
#8367 = DIRECTION ( 'NONE',  ( 0.000000000000000000, 0.000000000000000000, 1.000000000000000000 ) ) ;
#8368 = CYLINDRICAL_SURFACE ( 'NONE', #7692, 2.085824230283342740 ) ;
#8369 = CARTESIAN_POINT ( 'NONE',  ( 2.033589655956525188, -2.658578268446866399, -33.81118535743541287 ) ) ;
#8370 = CARTESIAN_POINT ( 'NONE',  ( -12.00000000000001066, 140.9999999999999716, -175.0000000000000284 ) ) ;
#8371 = DIRECTION ( 'NONE',  ( 3.697785493223492838E-32, 1.934419779023891545E-16, -1.000000000000000000 ) ) ;
#8372 = AXIS2_PLACEMENT_3D ( 'NONE', #30429, #22069, #3539 ) ;
#8373 = AXIS2_PLACEMENT_3D ( 'NONE', #31380, #1826, #12187 ) ;
#8374 = VECTOR ( 'NONE', #12146, 1000.000000000000000 ) ;
#8375 = ORIENTED_EDGE ( 'NONE', *, *, #6200, .T. ) ;
#8376 = LINE ( 'NONE', #16584, #32485 ) ;
#8377 = CARTESIAN_POINT ( 'NONE',  ( 849.8844278915690893, 1041.593900008597529, 1753.598338701302964 ) ) ;
#8378 = ORIENTED_EDGE ( 'NONE', *, *, #24585, .T. ) ;
#8379 = ORIENTED_EDGE ( 'NONE', *, *, #19499, .F. ) ;
#8380 = CIRCLE ( 'NONE', #25984, 4.000000000000003553 ) ;
#8381 = CARTESIAN_POINT ( 'NONE',  ( 102.9210534578009657, 5.351410369513340370, 5.255735268165820706 ) ) ;
#8382 = EDGE_CURVE ( 'NONE', #18126, #20668, #34989, .T. ) ;
#8383 = ORIENTED_EDGE ( 'NONE', *, *, #31763, .T. ) ;
#8384 = CARTESIAN_POINT ( 'NONE',  ( 0.000000000000000000, 3.524919873834583163E-15, 68.31122994652405112 ) ) ;
#8385 = CARTESIAN_POINT ( 'NONE',  ( -499.9999999999999432, -145.0000000000000000, -187.0000000000000000 ) ) ;
#8386 = EDGE_CURVE ( 'NONE', #21429, #26117, #29633, .T. ) ;
#8387 = EDGE_CURVE ( 'NONE', #16257, #5027, #24731, .T. ) ;
#8389 = DIRECTION ( 'NONE',  ( -1.000000000000000000, 0.000000000000000000, -0.000000000000000000 ) ) ;
#8388 = FACE_OUTER_BOUND ( 'NONE', #8759, .T. ) ;
#8390 = VECTOR ( 'NONE', #13636, 1000.000000000000000 ) ;
#8391 = EDGE_LOOP ( 'NONE', ( #18046, #29754, #34842, #24361, #11316, #11586 ) ) ;
#8392 = ORIENTED_EDGE ( 'NONE', *, *, #25680, .F. ) ;
#8393 = CARTESIAN_POINT ( 'NONE',  ( -9.978866888775632660, -3.725253662474303784, -67.50000000000000000 ) ) ;
#8394 = CARTESIAN_POINT ( 'NONE',  ( -12.00000000000001066, 144.9999999999999716, -186.9999999999999716 ) ) ;
#8395 = ADVANCED_FACE ( 'NONE', ( #13097 ), #29465, .T. ) ;
#8396 = DIRECTION ( 'NONE',  ( -1.000000000000000000, -0.000000000000000000, -0.000000000000000000 ) ) ;
#8397 = CARTESIAN_POINT ( 'NONE',  ( -10.00000000000000000, 0.000000000000000000, 0.000000000000000000 ) ) ;
#8398 = FACE_OUTER_BOUND ( 'NONE', #14678, .T. ) ;
#8399 = ORIENTED_EDGE ( 'NONE', *, *, #30630, .T. ) ;
#8401 = DIRECTION ( 'NONE',  ( 0.000000000000000000, 0.000000000000000000, -1.000000000000000000 ) ) ;
#8400 = VECTOR ( 'NONE', #27790, 999.9999999999998863 ) ;
#8403 = FACE_OUTER_BOUND ( 'NONE', #33163, .T. ) ;
#8402 = CIRCLE ( 'NONE', #9559, 4.000000000000003553 ) ;
#8404 = LINE ( 'NONE', #26737, #3290 ) ;
#8405 = DIRECTION ( 'NONE',  ( 0.000000000000000000, 0.000000000000000000, 1.000000000000000000 ) ) ;
#8406 =( NAMED_UNIT ( * ) SI_UNIT ( $, .STERADIAN. ) SOLID_ANGLE_UNIT ( ) );
#8407 = EDGE_CURVE ( 'NONE', #245, #6008, #7554, .T. ) ;
#8408 = DIRECTION ( 'NONE',  ( -1.000000000000000000, 0.000000000000000000, 1.848892746611746966E-32 ) ) ;
#8409 = MECHANICAL_DESIGN_GEOMETRIC_PRESENTATION_REPRESENTATION (  '', ( #20364 ), #2710 ) ;
#8411 = CARTESIAN_POINT ( 'NONE',  ( 37.55078559520313775, -4.831299144296470338, 68.31122994652405112 ) ) ;
#8410 = CARTESIAN_POINT ( 'NONE',  ( 1.039999999999999147, -24.90160365674884346, 23.75493189058332177 ) ) ;
#8412 = DIRECTION ( 'NONE',  ( 0.000000000000000000, 0.000000000000000000, 1.000000000000000000 ) ) ;
#8413 = ORIENTED_EDGE ( 'NONE', *, *, #27426, .T. ) ;
#8414 = DIRECTION ( 'NONE',  ( 0.000000000000000000, 0.000000000000000000, 1.000000000000000000 ) ) ;
#8416 = CARTESIAN_POINT ( 'NONE',  ( 110.1177974931836303, -2.622468385745837072, -7.036045090041716854 ) ) ;
#8415 = CARTESIAN_POINT ( 'NONE',  ( -0.9727285265192158192, -1.747512292859697114, 3.930000000000000160 ) ) ;
#8417 = VECTOR ( 'NONE', #18213, 1000.000000000000000 ) ;
#8418 = ORIENTED_EDGE ( 'NONE', *, *, #29791, .T. ) ;
#8419 = ORIENTED_EDGE ( 'NONE', *, *, #31180, .T. ) ;
#8420 = CIRCLE ( 'NONE', #26059, 34.41491905851385269 ) ;
#8421 = AXIS2_PLACEMENT_3D ( 'NONE', #32368, #164, #2652 ) ;
#8422 = ORIENTED_EDGE ( 'NONE', *, *, #22091, .T. ) ;
#8423 = FACE_BOUND ( 'NONE', #5408, .T. ) ;
#8424 = ORIENTED_EDGE ( 'NONE', *, *, #12117, .F. ) ;
#8425 = EDGE_LOOP ( 'NONE', ( #26192, #31699, #27048, #3458, #22844, #27025, #12510, #10788, #3333, #20172, #32420, #23199, #2626 ) ) ;
#8426 = CARTESIAN_POINT ( 'NONE',  ( 11.99999999999999645, 134.9999999999998863, 155.0000000000000000 ) ) ;
#8427 = AXIS2_PLACEMENT_3D ( 'NONE', #11249, #20104, #32590 ) ;
#8428 = ITEM_DEFINED_TRANSFORMATION ( 'NONE', 'NONE', #10419,  #28566 ) ;
#8429 = CARTESIAN_POINT ( 'NONE',  ( -105.0000000000000000, 0.000000000000000000, 60.00000000000000000 ) ) ;
#8430 = CARTESIAN_POINT ( 'NONE',  ( 2.783128855593303808, -27.79352918700739394, -13.43306967213438696 ) ) ;
#8431 = VERTEX_POINT ( 'NONE', #26433 ) ;
#8432 = VERTEX_POINT ( 'NONE', #21094 ) ;
#8433 = CARTESIAN_POINT ( 'NONE',  ( 127.4999999999999147, 1.530808498934191521E-15, -12.50000000000000000 ) ) ;
#8434 = CARTESIAN_POINT ( 'NONE',  ( 2.606461835800627291, -0.8174345826529154646, -32.26081300283389197 ) ) ;
#8435 = EDGE_CURVE ( 'NONE', #27344, #32731, #17463, .T. ) ;
#8436 = EDGE_CURVE ( 'NONE', #21178, #18207, #18448, .T. ) ;
#8437 = CARTESIAN_POINT ( 'NONE',  ( 104.6251203501937113, -5.728975534391925528, -11.10987307012756276 ) ) ;
#8438 = AXIS2_PLACEMENT_3D ( 'NONE', #34355, #17831, #21005 ) ;
#8439 = CARTESIAN_POINT ( 'NONE',  ( -20.02113311122488781, 8.235406450278430768, -87.50000000000000000 ) ) ;
#8440 = VERTEX_POINT ( 'NONE', #23930 ) ;
#8441 = LINE ( 'NONE', #5745, #29882 ) ;
#8442 = CIRCLE ( 'NONE', #31732, 30.47050528711512030 ) ;
#8443 = ADVANCED_FACE ( 'NONE', ( #34806 ), #32121, .F. ) ;
#8444 = ADVANCED_FACE ( 'NONE', ( #19148 ), #5753, .T. ) ;
#8445 = LINE ( 'NONE', #8609, #7317 ) ;
#8446 = ORIENTED_EDGE ( 'NONE', *, *, #28258, .F. ) ;
#8447 = DIRECTION ( 'NONE',  ( 0.7960930657056428661, -0.6051742151937663516, 0.000000000000000000 ) ) ;
#8448 = CYLINDRICAL_SURFACE ( 'NONE', #13781, 3.999999999999976019 ) ;
#8449 = DIRECTION ( 'NONE',  ( 1.000000000000000000, 3.040835319149746528E-31, 1.232595164407830946E-32 ) ) ;
#8450 = CARTESIAN_POINT ( 'NONE',  ( 0.1859802949991362364, -30.94574698966622250, -9.190792961030568975 ) ) ;
#8451 = ORIENTED_EDGE ( 'NONE', *, *, #32887, .F. ) ;
#8452 = B_SPLINE_CURVE_WITH_KNOTS ( 'NONE', 3,
 ( #56, #2369, #13593, #29436 ),
 .UNSPECIFIED., .F., .F.,
 ( 4, 4 ),
 ( 0.005298352064454681272, 0.005985220659832064284 ),
 .UNSPECIFIED. ) ;
#8453 = CARTESIAN_POINT ( 'NONE',  ( 0.000000000000000000, 33.69708579775584667, 49.43553178847298568 ) ) ;
#8454 = ORIENTED_EDGE ( 'NONE', *, *, #19698, .T. ) ;
#8456 = CARTESIAN_POINT ( 'NONE',  ( 5.021133111224473033, 4.168562732279007754, -87.50000000000000000 ) ) ;
#8455 = CARTESIAN_POINT ( 'NONE',  ( 4.170026905643898252E-16, 25.77033216996917631, 16.61395588374081456 ) ) ;
#8457 = CARTESIAN_POINT ( 'NONE',  ( 0.1835380964117766245, -22.67993007562076357, 22.95754798008695019 ) ) ;
#8458 = ADVANCED_FACE ( 'NONE', ( #11129 ), #614, .T. ) ;
#8459 = CIRCLE ( 'NONE', #32889, 15.00000000000000000 ) ;
#8460 = ORIENTED_EDGE ( 'NONE', *, *, #17006, .F. ) ;
#8461 = CARTESIAN_POINT ( 'NONE',  ( -2.791255079241054649, -37.75727539589163939, -36.68877005347593467 ) ) ;
#8462 = DIRECTION ( 'NONE',  ( -0.000000000000000000, -0.000000000000000000, -1.000000000000000000 ) ) ;
#8463 = VERTEX_POINT ( 'NONE', #16838 ) ;
#8464 = EDGE_CURVE ( 'NONE', #25101, #12748, #33357, .T. ) ;
#8465 = VECTOR ( 'NONE', #2047, 1000.000000000000000 ) ;
#8466 = EDGE_CURVE ( 'NONE', #21431, #6259, #11302, .T. ) ;
#8467 = ORIENTED_EDGE ( 'NONE', *, *, #25454, .F. ) ;
#8468 = CARTESIAN_POINT ( 'NONE',  ( -430.0000000000000000, -117.0000000000000000, 113.9999999999999858 ) ) ;
#8469 = VERTEX_POINT ( 'NONE', #266 ) ;
#8470 = ORIENTED_EDGE ( 'NONE', *, *, #9383, .T. ) ;
#8471 = CARTESIAN_POINT ( 'NONE',  ( -365.0000000000000000, 116.9999999999999858, 113.9999999999999858 ) ) ;
#8472 = CARTESIAN_POINT ( 'NONE',  ( -7.700000000000000178, 0.000000000000000000, 0.000000000000000000 ) ) ;
#8473 = CIRCLE ( 'NONE', #7309, 2.524999999999999467 ) ;
#8474 = DIRECTION ( 'NONE',  ( 1.000000000000000000, -0.000000000000000000, -0.000000000000000000 ) ) ;
#8475 = CARTESIAN_POINT ( 'NONE',  ( 1.749999999999999778, 6.714005886384948774, 33.75364837705175347 ) ) ;
#8476 = EDGE_LOOP ( 'NONE', ( #19930, #4070, #8031, #10541 ) ) ;
#8477 = ORIENTED_EDGE ( 'NONE', *, *, #9298, .F. ) ;
#8478 = DIRECTION ( 'NONE',  ( 5.546364386991661285E-52, 0.000000000000000000, 1.000000000000000000 ) ) ;
#8479 = CARTESIAN_POINT ( 'NONE',  ( 1.749999999999999778, 14.40815186467820475, -31.25366880301303496 ) ) ;
#8480 = PLANE ( 'NONE',  #27715 ) ;
#8481 = DIRECTION ( 'NONE',  ( 1.000000000000000000, 0.000000000000000000, 0.000000000000000000 ) ) ;
#8482 = CIRCLE ( 'NONE', #14192, 13.49999999999999822 ) ;
#8483 = CARTESIAN_POINT ( 'NONE',  ( 12.00000000000001066, -64.99999999999997158, -175.0000000000000000 ) ) ;
#8484 = EDGE_CURVE ( 'NONE', #8779, #6860, #21979, .T. ) ;
#8485 = EDGE_CURVE ( 'NONE', #29323, #2729, #14525, .T. ) ;
#8486 = CARTESIAN_POINT ( 'NONE',  ( -414.0000000000000568, -124.9999999999999858, -77.99999999999997158 ) ) ;
#8487 = LINE ( 'NONE', #2959, #16433 ) ;
#8488 = ORIENTED_EDGE ( 'NONE', *, *, #32543, .T. ) ;
#8489 = LINE ( 'NONE', #30198, #29296 ) ;
#8490 = CARTESIAN_POINT ( 'NONE',  ( 0.5248940569443696358, -17.22577838686597218, 28.59166429730529657 ) ) ;
#8491 = LINE ( 'NONE', #19539, #11528 ) ;
#8492 = ORIENTED_EDGE ( 'NONE', *, *, #28120, .T. ) ;
#8493 = VECTOR ( 'NONE', #24052, 1000.000000000000000 ) ;
#8494 =( REPRESENTATION_RELATIONSHIP ('NONE','NONE', #23037, #28231 ) REPRESENTATION_RELATIONSHIP_WITH_TRANSFORMATION ( #17118 )SHAPE_REPRESENTATION_RELATIONSHIP( ) );
#8495 = CARTESIAN_POINT ( 'NONE',  ( -37.85301660235036536, 0.7430237821112573027, -15.81122994652406355 ) ) ;
#8496 = ORIENTED_EDGE ( 'NONE', *, *, #25634, .T. ) ;
#8497 = DIRECTION ( 'NONE',  ( 0.000000000000000000, 0.000000000000000000, 1.000000000000000000 ) ) ;
#8498 = CARTESIAN_POINT ( 'NONE',  ( -100.5674440995040442, 2.574279381791158450, 12.23535145228419907 ) ) ;
#8499 = AXIS2_PLACEMENT_3D ( 'NONE', #15321, #28657, #29001 ) ;
#8500 = ORIENTED_EDGE ( 'NONE', *, *, #3903, .F. ) ;
#8501 = CARTESIAN_POINT ( 'NONE',  ( 0.000000000000000000, 17.11426446101236820, -26.96776559937708129 ) ) ;
#8502 = CYLINDRICAL_SURFACE ( 'NONE', #32698, 16.19999999999999929 ) ;
#8503 = FACE_OUTER_BOUND ( 'NONE', #16906, .T. ) ;
#8504 = ADVANCED_FACE ( 'NONE', ( #13794 ), #22328, .F. ) ;
#8505 = ORIENTED_EDGE ( 'NONE', *, *, #27189, .F. ) ;
#8506 = AXIS2_PLACEMENT_3D ( 'NONE', #31965, #4725, #2076 ) ;
#8507 = ADVANCED_FACE ( 'NONE', ( #8797 ), #6284, .F. ) ;
#8508 = EDGE_CURVE ( 'NONE', #20981, #2999, #13976, .T. ) ;
#8509 = DIRECTION ( 'NONE',  ( 0.1063910735369155841, -0.9943243633099125844, -3.335902418025060287E-15 ) ) ;
#8510 = CARTESIAN_POINT ( 'NONE',  ( 1.749999999999999778, 0.000000000000000000, 0.000000000000000000 ) ) ;
#8511 = ORIENTED_EDGE ( 'NONE', *, *, #4936, .T. ) ;
#8512 = CARTESIAN_POINT ( 'NONE',  ( 0.5288002472147362854, -24.86182815675670810, 22.28830832814871599 ) ) ;
#8513 = EDGE_CURVE ( 'NONE', #5041, #14854, #6113, .T. ) ;
#8514 = EDGE_CURVE ( 'NONE', #12038, #10814, #22512, .T. ) ;
#8515 = DIRECTION ( 'NONE',  ( 0.000000000000000000, 1.836970198721029934E-16, -1.000000000000000000 ) ) ;
#8516 = CARTESIAN_POINT ( 'NONE',  ( -104.1337689642702600, -5.044029065977395199, 5.550668370081901948 ) ) ;
#8517 = ORIENTED_EDGE ( 'NONE', *, *, #34012, .T. ) ;
#8518 = ORIENTED_EDGE ( 'NONE', *, *, #26675, .T. ) ;
#8519 = ORIENTED_EDGE ( 'NONE', *, *, #8906, .T. ) ;
#8520 = DIRECTION ( 'NONE',  ( -1.000000000000000000, -0.000000000000000000, -0.000000000000000000 ) ) ;
#8521 = CARTESIAN_POINT ( 'NONE',  ( -36.80830595996284416, 8.862931941313773265, 68.31122994652405112 ) ) ;
#8522 = CARTESIAN_POINT ( 'NONE',  ( 2.719051668256705856, -22.12275578582363877, 22.69570394412120251 ) ) ;
#8523 = ORIENTED_EDGE ( 'NONE', *, *, #19695, .T. ) ;
#8524 = ORIENTED_EDGE ( 'NONE', *, *, #15558, .F. ) ;
#8525 = LINE ( 'NONE', #5493, #17483 ) ;
#8526 = VERTEX_POINT ( 'NONE', #16476 ) ;
#8527 = DIRECTION ( 'NONE',  ( 0.000000000000000000, 0.000000000000000000, 1.000000000000000000 ) ) ;
#8528 = DIRECTION ( 'NONE',  ( -1.000000000000000000, -0.000000000000000000, -0.000000000000000000 ) ) ;
#8529 = ORIENTED_EDGE ( 'NONE', *, *, #20887, .F. ) ;
#8530 = AXIS2_PLACEMENT_3D ( 'NONE', #27245, #19086, #32757 ) ;
#8531 = VERTEX_POINT ( 'NONE', #27837 ) ;
#8532 = CARTESIAN_POINT ( 'NONE',  ( -499.9999999999999432, 136.9999999999999432, -159.0000000000000000 ) ) ;
#8533 = CARTESIAN_POINT ( 'NONE',  ( -23.78520691327551262, 22.21414650552148373, 68.31122994652405112 ) ) ;
#8534 = ORIENTED_EDGE ( 'NONE', *, *, #25230, .F. ) ;
#8535 = PLANE ( 'NONE',  #20351 ) ;
#8536 = DIRECTION ( 'NONE',  ( 0.000000000000000000, -1.000000000000000000, 6.123233995736766036E-17 ) ) ;
#8537 = CARTESIAN_POINT ( 'NONE',  ( -418.0000000000000000, -104.9999999999999716, -187.0000000000000000 ) ) ;
#8538 = SURFACE_SIDE_STYLE ('',( #11392 ) ) ;
#8539 =( REPRESENTATION_RELATIONSHIP ('NONE','NONE', #23037, #28231 ) REPRESENTATION_RELATIONSHIP_WITH_TRANSFORMATION ( #34743 )SHAPE_REPRESENTATION_RELATIONSHIP( ) );
#8540 = CARTESIAN_POINT ( 'NONE',  ( 2.765921099433443331, -3.506335382740311868, -30.89238256715869468 ) ) ;
#8541 = LINE ( 'NONE', #21719, #25251 ) ;
#8542 = CARTESIAN_POINT ( 'NONE',  ( 15.99999999999998579, 124.9999999999999716, 187.0000000000000000 ) ) ;
#8543 = EDGE_CURVE ( 'NONE', #12316, #14561, #8614, .T. ) ;
#8544 = EDGE_CURVE ( 'NONE', #8215, #33409, #14339, .T. ) ;
#8545 = ORIENTED_EDGE ( 'NONE', *, *, #20382, .T. ) ;
#8546 = CARTESIAN_POINT ( 'NONE',  ( 0.02407890056655608360, 14.63235270440974922, -27.43224275967423509 ) ) ;
#8547 = DIRECTION ( 'NONE',  ( 2.631201909438060269E-14, -5.396010391056495992E-16, 0.9999999999999998890 ) ) ;
#8548 = ORIENTED_EDGE ( 'NONE', *, *, #5609, .T. ) ;
#8549 = ORIENTED_EDGE ( 'NONE', *, *, #14574, .F. ) ;
#8550 = VECTOR ( 'NONE', #1040, 1000.000000000000000 ) ;
#8551 = CARTESIAN_POINT ( 'NONE',  ( -32.17792593279633451, -19.96555837188920890, -36.68877005347593467 ) ) ;
#8552 = VERTEX_POINT ( 'NONE', #86 ) ;
#8553 = DIRECTION ( 'NONE',  ( 0.000000000000000000, 0.000000000000000000, 1.000000000000000000 ) ) ;
#8554 = DIRECTION ( 'NONE',  ( 0.000000000000000000, 0.000000000000000000, 1.000000000000000000 ) ) ;
#8555 = ITEM_DEFINED_TRANSFORMATION ( 'NONE', 'NONE', #27488,  #28566 ) ;
#8557 = DIRECTION ( 'NONE',  ( 0.000000000000000000, 0.000000000000000000, -1.000000000000000000 ) ) ;
#8556 = CARTESIAN_POINT ( 'NONE',  ( 2.606461833931011274, -18.30111164264898704, 26.58002197185221149 ) ) ;
#8559 = VERTEX_POINT ( 'NONE', #21792 ) ;
#8558 = CIRCLE ( 'NONE', #1202, 4.000000000000003553 ) ;
#8560 = EDGE_LOOP ( 'NONE', ( #23090, #25447, #23085, #3124, #10169, #31747 ) ) ;
#8561 = PLANE ( 'NONE',  #16297 ) ;
#8562 = CARTESIAN_POINT ( 'NONE',  ( -27.13361903382165963, -26.41607761506755736, -36.68877005347593467 ) ) ;
#8563 = DIRECTION ( 'NONE',  ( -0.000000000000000000, 1.836970198721029934E-16, -1.000000000000000000 ) ) ;
#8564 = CARTESIAN_POINT ( 'NONE',  ( 0.000000000000000000, 0.000000000000000000, 0.000000000000000000 ) ) ;
#8565 = PRODUCT_DEFINITION_CONTEXT ( 'detailed design', #6666, 'design' ) ;
#8566 = ORIENTED_EDGE ( 'NONE', *, *, #11534, .F. ) ;
#8567 = DIRECTION ( 'NONE',  ( 1.000000000000000000, 3.040835319149746528E-31, 1.232595164407830946E-32 ) ) ;
#8568 = DIRECTION ( 'NONE',  ( 1.000000000000000000, 0.000000000000000000, -0.000000000000000000 ) ) ;
#8569 = CARTESIAN_POINT ( 'NONE',  ( 2.789999999999999147, -17.83604598421647935, -24.70480026434183429 ) ) ;
#8570 = ORIENTED_EDGE ( 'NONE', *, *, #23719, .T. ) ;
#8571 = AXIS2_PLACEMENT_3D ( 'NONE', #13789, #27294, #10770 ) ;
#8572 = CARTESIAN_POINT ( 'NONE',  ( 0.1835382041699210043, -11.11596589742306129, -30.29626325691716815 ) ) ;
#8573 = CARTESIAN_POINT ( 'NONE',  ( 0.7561992263075686393, 6.875399836226445238, 33.21096214980147465 ) ) ;
#8574 = CIRCLE ( 'NONE', #19975, 30.47050528711512030 ) ;
#8575 = LINE ( 'NONE', #8224, #17814 ) ;
#8577 = LINE ( 'NONE', #19978, #31584 ) ;
#8576 = DIRECTION ( 'NONE',  ( 0.000000000000000000, -1.000000000000000000, -1.836970198721029934E-16 ) ) ;
#8578 = DIRECTION ( 'NONE',  ( 0.000000000000000000, 1.000000000000000000, -6.842277657836020854E-49 ) ) ;
#8579 = ORIENTED_EDGE ( 'NONE', *, *, #29645, .F. ) ;
#8580 = DIRECTION ( 'NONE',  ( 0.000000000000000000, 1.000000000000000000, 1.934419779023891545E-16 ) ) ;
#8581 = SURFACE_SIDE_STYLE ('',( #27985 ) ) ;
#8582 = EDGE_CURVE ( 'NONE', #22067, #26131, #29987, .T. ) ;
#8583 = EDGE_CURVE ( 'NONE', #3175, #19641, #21348, .T. ) ;
#8584 = ORIENTED_EDGE ( 'NONE', *, *, #6204, .T. ) ;
#8585 = VECTOR ( 'NONE', #15501, 1000.000000000000000 ) ;
#8586 = VECTOR ( 'NONE', #27760, 1000.000000000000000 ) ;
#8587 = B_SPLINE_CURVE_WITH_KNOTS ( 'NONE', 3,
 ( #4830, #15725, #12878, #7864 ),
 .UNSPECIFIED., .F., .F.,
 ( 4, 4 ),
 ( 2.557638148655773837E-07, 0.0006879919438241504466 ),
 .UNSPECIFIED. ) ;
#8588 = EDGE_CURVE ( 'NONE', #27945, #11027, #11661, .T. ) ;
#8589 = ORIENTED_EDGE ( 'NONE', *, *, #15548, .F. ) ;
#8590 = VERTEX_POINT ( 'NONE', #14154 ) ;
#8591 = FACE_OUTER_BOUND ( 'NONE', #10226, .T. ) ;
#8592 = VERTEX_POINT ( 'NONE', #9327 ) ;
#8593 = VERTEX_POINT ( 'NONE', #22861 ) ;
#8594 = VECTOR ( 'NONE', #28010, 1000.000000000000000 ) ;
#8595 = DIRECTION ( 'NONE',  ( -1.000000000000000000, 0.000000000000000000, -0.000000000000000000 ) ) ;
#8596 = VECTOR ( 'NONE', #4222, 1000.000000000000000 ) ;
#8597 = ITEM_DEFINED_TRANSFORMATION ( 'NONE', 'NONE', #13831,  #28566 ) ;
#8598 = VERTEX_POINT ( 'NONE', #31216 ) ;
#8599 = FACE_OUTER_BOUND ( 'NONE', #16959, .T. ) ;
#8600 = CARTESIAN_POINT ( 'NONE',  ( -347.0000000000000000, 134.9999999999999716, 114.0000000000000000 ) ) ;
#8601 = VERTEX_POINT ( 'NONE', #6819 ) ;
#8602 = ORIENTED_EDGE ( 'NONE', *, *, #5718, .F. ) ;
#8603 = LINE ( 'NONE', #19483, #26490 ) ;
#8604 = DIRECTION ( 'NONE',  ( 0.000000000000000000, -1.000000000000000000, -2.465190328815662439E-32 ) ) ;
#8605 = CARTESIAN_POINT ( 'NONE',  ( 103.1365178746234363, -5.440007577125886229, -11.25529792293082032 ) ) ;
#8606 = CARTESIAN_POINT ( 'NONE',  ( -442.0000000000000000, 124.9999999999999432, -155.0000000000000000 ) ) ;
#8607 = ORIENTED_EDGE ( 'NONE', *, *, #20098, .T. ) ;
#8608 = DIRECTION ( 'NONE',  ( 0.000000000000000000, -2.312964634635743450E-15, -1.000000000000000000 ) ) ;
#8609 = CARTESIAN_POINT ( 'NONE',  ( 3.235562306570555532E-30, 8.235406450278427215, -67.50000000000000000 ) ) ;
#8610 = ORIENTED_EDGE ( 'NONE', *, *, #13820, .T. ) ;
#8611 = AXIS2_PLACEMENT_3D ( 'NONE', #30397, #33768, #27542 ) ;
#8612 = VECTOR ( 'NONE', #32834, 1000.000000000000000 ) ;
#8613 = AXIS2_PLACEMENT_3D ( 'NONE', #13409, #24242, #12147 ) ;
#8614 = LINE ( 'NONE', #3443, #29857 ) ;
#8615 = DIRECTION ( 'NONE',  ( 0.000000000000000000, -2.465190328815661892E-32, -1.000000000000000000 ) ) ;
#8616 = FACE_OUTER_BOUND ( 'NONE', #12595, .T. ) ;
#8617 = CARTESIAN_POINT ( 'NONE',  ( 2.606461796175087997, 7.231184547465761447, -31.45056812073505270 ) ) ;
#8618 = ORIENTED_EDGE ( 'NONE', *, *, #5078, .F. ) ;
#8619 = DIRECTION ( 'NONE',  ( 0.000000000000000000, -5.145227585319922065E-49, -1.000000000000000000 ) ) ;
#8620 = ORIENTED_EDGE ( 'NONE', *, *, #18281, .T. ) ;
#8622 = FACE_OUTER_BOUND ( 'NONE', #9036, .T. ) ;
#8621 = CARTESIAN_POINT ( 'NONE',  ( 2.265105899770494702, 27.45362965837546909, -18.98707279867223008 ) ) ;
#8623 = EDGE_CURVE ( 'NONE', #32949, #11691, #17883, .T. ) ;
#8624 = VECTOR ( 'NONE', #303, 1000.000000000000114 ) ;
#8625 = VERTEX_POINT ( 'NONE', #25877 ) ;
#8626 = CARTESIAN_POINT ( 'NONE',  ( -430.0000000000000000, -131.0000000000000000, 126.0000000000000000 ) ) ;
#8627 = PRODUCT ( 'angular contact ball bearing_68_iso_ISO 15 ABB - 5820 - Full,SI,NC,Full_68', 'angular contact ball bearing_68_iso_ISO 15 ABB - 5820 - Full,SI,NC,Full_68', '', ( #25094 ) ) ;
#8628 = DIRECTION ( 'NONE',  ( 0.000000000000000000, 1.836970198721029441E-16, -1.000000000000000000 ) ) ;
#8629 = EDGE_CURVE ( 'NONE', #4640, #28395, #28549, .T. ) ;
#8630 = ADVANCED_FACE ( 'NONE', ( #28888 ), #25338, .T. ) ;
#8631 = ORIENTED_EDGE ( 'NONE', *, *, #9555, .F. ) ;
#8632 = VECTOR ( 'NONE', #26314, 999.9999999999998863 ) ;
#8633 = VECTOR ( 'NONE', #34057, 1000.000000000000000 ) ;
#8634 = EDGE_CURVE ( 'NONE', #2214, #16123, #20023, .T. ) ;
#8635 = EDGE_CURVE ( 'NONE', #19142, #13351, #3968, .T. ) ;
#8636 = ORIENTED_EDGE ( 'NONE', *, *, #22989, .F. ) ;
#8637 = DIRECTION ( 'NONE',  ( 0.000000000000000000, 1.836970198721029441E-16, -1.000000000000000000 ) ) ;
#8638 = CARTESIAN_POINT ( 'NONE',  ( 12.00000000000001066, -32.99999999999997158, -154.9999999999999716 ) ) ;
#8639 = ORIENTED_EDGE ( 'NONE', *, *, #12857, .T. ) ;
#8640 = EDGE_LOOP ( 'NONE', ( #7757, #28443, #30687, #19475 ) ) ;
#8641 = AXIS2_PLACEMENT_3D ( 'NONE', #2491, #18885, #8366 ) ;
#8642 = LINE ( 'NONE', #27685, #11048 ) ;
#8643 = EDGE_CURVE ( 'NONE', #32317, #10400, #13204, .T. ) ;
#8644 = CARTESIAN_POINT ( 'NONE',  ( -414.0000000000000568, -137.0000000000000000, -155.0000000000000000 ) ) ;
#8645 = CARTESIAN_POINT ( 'NONE',  ( 1.040000000000002034, 32.09669216789253454, -12.41728656686340315 ) ) ;
#8646 = CARTESIAN_POINT ( 'NONE',  ( -430.0000000000000000, 130.9999999999999716, 111.9999999999999858 ) ) ;
#8647 = ORIENTED_EDGE ( 'NONE', *, *, #29737, .T. ) ;
#8648 = EDGE_LOOP ( 'NONE', ( #623, #33785, #8529, #13242 ) ) ;
#8649 = DIRECTION ( 'NONE',  ( 0.000000000000000000, 1.000000000000000000, 0.000000000000000000 ) ) ;
#8650 = CARTESIAN_POINT ( 'NONE',  ( 22.89764159710615132, -1.579009122040562207, -77.50000000000000000 ) ) ;
#8651 = DIRECTION ( 'NONE',  ( 0.000000000000000000, 0.000000000000000000, -1.000000000000000000 ) ) ;
#8652 = DIRECTION ( 'NONE',  ( 0.000000000000000000, -1.000000000000000000, 3.374343856708137958E-53 ) ) ;
#8653 = CARTESIAN_POINT ( 'NONE',  ( 0.02407890056655608360, 14.63235270440974922, -27.43224275967423509 ) ) ;
#8654 = LINE ( 'NONE', #27174, #2120 ) ;
#8655 = CARTESIAN_POINT ( 'NONE',  ( 0.02407890056655695096, -21.56796757982826307, 22.39322359481599278 ) ) ;
#8656 = ORIENTED_EDGE ( 'NONE', *, *, #13626, .T. ) ;
#8657 = CLOSED_SHELL ( 'NONE', ( #21004, #24410, #19616, #27914, #22164, #33945, #5857, #9540, #21077, #25711, #3534, #28709, #5521, #14832, #3612, #13063, #34674, #3473, #25599, #8758, #28836, #208, #26922, #18145, #7341, #17096, #3003 ) ) ;
#8658 = DIRECTION ( 'NONE',  ( 0.000000000000000000, 0.000000000000000000, 1.000000000000000000 ) ) ;
#8659 = CARTESIAN_POINT ( 'NONE',  ( -2.216215597024039141, -32.46987467335850397, -36.68877005347593467 ) ) ;
#8660 = AXIS2_PLACEMENT_3D ( 'NONE', #29260, #15749, #22572 ) ;
#8662 = DIRECTION ( 'NONE',  ( 0.000000000000000000, -1.000000000000000000, -5.053935297177146739E-49 ) ) ;
#8661 = B_SPLINE_CURVE_WITH_KNOTS ( 'NONE', 3,
 ( #2522, #7686, #29050, #13401, #16255, #2003 ),
 .UNSPECIFIED., .F., .F.,
 ( 4, 2, 4 ),
 ( 2.008842330431681463E-07, 0.001873399179558949725, 0.003746597474884856213 ),
 .UNSPECIFIED. ) ;
#8663 = VERTEX_POINT ( 'NONE', #1320 ) ;
#8664 = AXIS2_PLACEMENT_3D ( 'NONE', #15250, #13274, #17934 ) ;
#8665 = AXIS2_PLACEMENT_3D ( 'NONE', #21239, #27510, #2194 ) ;
#8666 = AXIS2_PLACEMENT_3D ( 'NONE', #22559, #837, #11705 ) ;
#8667 = LINE ( 'NONE', #2795, #28614 ) ;
#8668 = ORIENTED_EDGE ( 'NONE', *, *, #32045, .F. ) ;
#8669 = CARTESIAN_POINT ( 'NONE',  ( -349.0000000000000000, 124.9999999999999432, 168.9999999999999716 ) ) ;
#8670 = CARTESIAN_POINT ( 'NONE',  ( 2.765921099433443331, -29.68817180695682723, 9.232883799364120847 ) ) ;
#8671 = ORIENTED_EDGE ( 'NONE', *, *, #24789, .T. ) ;
#8672 = SHAPE_REPRESENTATION ( 'hex structural bolt gradec short_iso_ISO 7412 - M16 x 45 --- 26-WN', ( #28566 ), #29141 ) ;
#8673 = CARTESIAN_POINT ( 'NONE',  ( -45.05956070192387841, -20.15143121711730245, 0.000000000000000000 ) ) ;
#8674 = DIRECTION ( 'NONE',  ( -0.000000000000000000, 0.000000000000000000, -1.000000000000000000 ) ) ;
#8675 = DIRECTION ( 'NONE',  ( 0.000000000000000000, 1.836970198721029688E-16, -1.000000000000000000 ) ) ;
#8676 = ADVANCED_FACE ( 'NONE', ( #17370 ), #4488, .T. ) ;
#8677 = VERTEX_POINT ( 'NONE', #20534 ) ;
#8678 = ADVANCED_FACE ( 'NONE', ( #31388 ), #6992, .F. ) ;
#8679 = EDGE_CURVE ( 'NONE', #17981, #6860, #4317, .T. ) ;
#8680 = CARTESIAN_POINT ( 'NONE',  ( 847.8098030874582491, 1060.983214533547653, 1753.598338701303419 ) ) ;
#8681 = DIRECTION ( 'NONE',  ( 0.000000000000000000, 1.000000000000000000, 0.000000000000000000 ) ) ;
#8682 = ORIENTED_EDGE ( 'NONE', *, *, #15815, .F. ) ;
#8683 = FACE_OUTER_BOUND ( 'NONE', #30492, .T. ) ;
#8684 = FACE_OUTER_BOUND ( 'NONE', #19828, .T. ) ;
#8685 = LINE ( 'NONE', #14407, #18479 ) ;
#8686 = LINE ( 'NONE', #19218, #7986 ) ;
#8687 = AXIS2_PLACEMENT_3D ( 'NONE', #20845, #4620, #28854 ) ;
#8688 = ORIENTED_EDGE ( 'NONE', *, *, #19115, .F. ) ;
#8689 = VERTEX_POINT ( 'NONE', #25695 ) ;
#8690 = CIRCLE ( 'NONE', #22341, 34.41491905851385269 ) ;
#8691 = ORIENTED_EDGE ( 'NONE', *, *, #4284, .T. ) ;
#8692 = DIRECTION ( 'NONE',  ( 0.000000000000000000, 0.000000000000000000, -1.000000000000000000 ) ) ;
#8693 = EDGE_CURVE ( 'NONE', #18536, #22062, #9846, .T. ) ;
#8694 = CARTESIAN_POINT ( 'NONE',  ( -25.63124651156763179, 20.05601094782693394, 68.31122994652405112 ) ) ;
#8695 = DIRECTION ( 'NONE',  ( 1.848892746611746419E-32, 6.842277657836020854E-49, -1.000000000000000000 ) ) ;
#8696 = ORIENTED_EDGE ( 'NONE', *, *, #29160, .T. ) ;
#8697 = ORIENTED_EDGE ( 'NONE', *, *, #34759, .T. ) ;
#8698 = CARTESIAN_POINT ( 'NONE',  ( 2.265105948359096288, -29.61686074518757295, 15.39650178189414476 ) ) ;
#8699 = VERTEX_POINT ( 'NONE', #31047 ) ;
#8700 = EDGE_CURVE ( 'NONE', #28240, #22752, #28733, .T. ) ;
#8701 = CARTESIAN_POINT ( 'NONE',  ( -499.9999999999999432, 144.9999999999999716, 187.0000000000000000 ) ) ;
#8702 = LINE ( 'NONE', #3361, #25067 ) ;
#8703 = VERTEX_POINT ( 'NONE', #22693 ) ;
#8704 = EDGE_CURVE ( 'NONE', #27908, #4571, #12193, .T. ) ;
#8706 = EDGE_CURVE ( 'NONE', #3104, #23064, #28196, .T. ) ;
#8705 = ORIENTED_EDGE ( 'NONE', *, *, #8747, .T. ) ;
#8707 = CARTESIAN_POINT ( 'NONE',  ( -361.0000000000000000, -125.0000000000000284, 181.0000000000000000 ) ) ;
#8708 = AXIS2_PLACEMENT_3D ( 'NONE', #2185, #18587, #10374 ) ;
#8709 = DIRECTION ( 'NONE',  ( 0.000000000000000000, 0.000000000000000000, -1.000000000000000000 ) ) ;
#8710 = VERTEX_POINT ( 'NONE', #33890 ) ;
#8711 = CARTESIAN_POINT ( 'NONE',  ( -5.469264258321805627, 1.713938105891546382, -0.7500000000000000000 ) ) ;
#8712 = DIRECTION ( 'NONE',  ( 0.000000000000000000, 0.000000000000000000, 1.000000000000000000 ) ) ;
#8713 = EDGE_CURVE ( 'NONE', #22746, #3220, #21230, .T. ) ;
#8714 = DIRECTION ( 'NONE',  ( -1.000000000000000000, 0.000000000000000000, 0.000000000000000000 ) ) ;
#8716 = DIRECTION ( 'NONE',  ( 1.000000000000000000, 3.469446951953834515E-18, 0.000000000000000000 ) ) ;
#8715 = AXIS2_PLACEMENT_3D ( 'NONE', #17767, #15269, #28080 ) ;
#8717 = VECTOR ( 'NONE', #14206, 1000.000000000000000 ) ;
#8718 = AXIS2_PLACEMENT_3D ( 'NONE', #6568, #33275, #3890 ) ;
#8719 = DIRECTION ( 'NONE',  ( 1.000000000000000000, 0.000000000000000000, 0.000000000000000000 ) ) ;
#8720 = LINE ( 'NONE', #544, #24157 ) ;
#8721 = ORIENTED_EDGE ( 'NONE', *, *, #33222, .T. ) ;
#8722 = EDGE_CURVE ( 'NONE', #30104, #7716, #15917, .T. ) ;
#8723 = DIRECTION ( 'NONE',  ( 2.631201909438060269E-14, -5.396010391056495992E-16, 0.9999999999999998890 ) ) ;
#8724 = ORIENTED_EDGE ( 'NONE', *, *, #34882, .T. ) ;
#8725 = ORIENTED_EDGE ( 'NONE', *, *, #30283, .T. ) ;
#8726 = DIRECTION ( 'NONE',  ( 0.000000000000000000, -1.000000000000000000, 6.123233995736766036E-17 ) ) ;
#8727 = LINE ( 'NONE', #384, #32402 ) ;
#8728 = APPLICATION_PROTOCOL_DEFINITION ( 'draft international standard', 'automotive_design', 1998, #10309 ) ;
#8729 = ORIENTED_EDGE ( 'NONE', *, *, #24585, .F. ) ;
#8730 = LINE ( 'NONE', #16595, #304 ) ;
#8731 = CARTESIAN_POINT ( 'NONE',  ( -103.3404196479744570, -4.849832969747407851, -11.52164913186504513 ) ) ;
#8732 = ITEM_DEFINED_TRANSFORMATION ( 'NONE', 'NONE', #32613,  #28566 ) ;
#8734 = DIRECTION ( 'NONE',  ( 0.000000000000000000, 0.000000000000000000, 1.000000000000000000 ) ) ;
#8733 = CYLINDRICAL_SURFACE ( 'NONE', #25244, 7.999999999999979572 ) ;
#8735 = VECTOR ( 'NONE', #33714, 1000.000000000000000 ) ;
#8736 = ORIENTED_EDGE ( 'NONE', *, *, #18783, .T. ) ;
#8737 = EDGE_LOOP ( 'NONE', ( #34351, #34926 ) ) ;
#8738 = VECTOR ( 'NONE', #1842, 1000.000000000000000 ) ;
#8739 = CARTESIAN_POINT ( 'NONE',  ( -31.68358972719164512, 7.440061483287534472, 68.31122994652405112 ) ) ;
#8740 = DIRECTION ( 'NONE',  ( 0.000000000000000000, 1.836970198721029441E-16, -1.000000000000000000 ) ) ;
#8741 = DIRECTION ( 'NONE',  ( 0.000000000000000000, 0.000000000000000000, -1.000000000000000000 ) ) ;
#8742 = DIRECTION ( 'NONE',  ( 0.000000000000000000, 0.000000000000000000, -1.000000000000000000 ) ) ;
#8743 = ORIENTED_EDGE ( 'NONE', *, *, #23664, .F. ) ;
#8744 = ADVANCED_FACE ( 'NONE', ( #18925 ), #3142, .T. ) ;
#8745 = CARTESIAN_POINT ( 'NONE',  ( 12.46788440507149964, 30.06253867087536946, 68.31122994652405112 ) ) ;
#8746 = CARTESIAN_POINT ( 'NONE',  ( -355.0000000000000000, 130.9999999999999716, 128.0000000000000000 ) ) ;
#8747 = EDGE_CURVE ( 'NONE', #8677, #33838, #10200, .T. ) ;
#8748 = DIRECTION ( 'NONE',  ( 1.000000000000000000, 0.000000000000000000, 0.000000000000000000 ) ) ;
#8749 =( REPRESENTATION_RELATIONSHIP ('NONE','NONE', #23037, #15767 ) REPRESENTATION_RELATIONSHIP_WITH_TRANSFORMATION ( #33064 )SHAPE_REPRESENTATION_RELATIONSHIP( ) );
#8750 = ORIENTED_EDGE ( 'NONE', *, *, #2568, .F. ) ;
#8751 = CARTESIAN_POINT ( 'NONE',  ( 2.033800778643362506, 33.71011734938328885, -3.723857881850640261 ) ) ;
#8752 = DIRECTION ( 'NONE',  ( 0.000000000000000000, 0.000000000000000000, 1.000000000000000000 ) ) ;
#8753 = DIRECTION ( 'NONE',  ( 0.000000000000000000, -1.000000000000000000, 0.000000000000000000 ) ) ;
#8755 = CARTESIAN_POINT ( 'NONE',  ( -363.0000000000000000, -125.0000000000000284, 114.0000000000000000 ) ) ;
#8754 = DIRECTION ( 'NONE',  ( 0.000000000000000000, 1.836970198721029441E-16, -1.000000000000000000 ) ) ;
#8756 = VECTOR ( 'NONE', #1685, 1000.000000000000000 ) ;
#8758 = ADVANCED_FACE ( 'NONE', ( #10024 ), #34412, .T. ) ;
#8757 = CARTESIAN_POINT ( 'NONE',  ( 0.000000000000000000, 12.80000000000000071, 3.000000000000000000 ) ) ;
#8759 = EDGE_LOOP ( 'NONE', ( #3295, #19128, #4474, #9139 ) ) ;
#8760 = CARTESIAN_POINT ( 'NONE',  ( -499.9999999999999432, 104.9999999999999858, -187.0000000000000000 ) ) ;
#8761 = AXIS2_PLACEMENT_3D ( 'NONE', #12920, #23762, #34619 ) ;
#8762 = ORIENTED_EDGE ( 'NONE', *, *, #13140, .T. ) ;
#8764 = VERTEX_POINT ( 'NONE', #18228 ) ;
#8763 = AXIS2_PLACEMENT_3D ( 'NONE', #2882, #30484, #27981 ) ;
#8765 = VECTOR ( 'NONE', #10164, 1000.000000000000114 ) ;
#8766 = AXIS2_PLACEMENT_3D ( 'NONE', #24960, #31489, #19996 ) ;
#8767 = ORIENTED_EDGE ( 'NONE', *, *, #33879, .T. ) ;
#8768 = ORIENTED_EDGE ( 'NONE', *, *, #7754, .T. ) ;
#8769 = DIRECTION ( 'NONE',  ( 0.000000000000000000, 0.000000000000000000, -1.000000000000000000 ) ) ;
#8770 = ORIENTED_EDGE ( 'NONE', *, *, #13867, .F. ) ;
#8771 = ORIENTED_EDGE ( 'NONE', *, *, #6778, .F. ) ;
#8772 = EDGE_CURVE ( 'NONE', #21158, #1876, #21587, .T. ) ;
#8773 = CARTESIAN_POINT ( 'NONE',  ( 145.0000000000000568, -88.29863524074325198, -74.12844257252345415 ) ) ;
#8774 = CIRCLE ( 'NONE', #3082, 4.306175033202026547 ) ;
#8775 = VERTEX_POINT ( 'NONE', #16084 ) ;
#8776 = FACE_OUTER_BOUND ( 'NONE', #5477, .T. ) ;
#8777 = CARTESIAN_POINT ( 'NONE',  ( -445.9999999999999432, -137.0000000000000000, -155.0000000000000000 ) ) ;
#8778 = ORIENTED_EDGE ( 'NONE', *, *, #7752, .T. ) ;
#8779 = VERTEX_POINT ( 'NONE', #18586 ) ;
#8780 = DIRECTION ( 'NONE',  ( -3.040835319149746090E-31, -1.000000000000000000, 0.000000000000000000 ) ) ;
#8781 = FACE_BOUND ( 'NONE', #13923, .T. ) ;
#8782 = VECTOR ( 'NONE', #18699, 1000.000000000000114 ) ;
#8783 = ADVANCED_FACE ( 'NONE', ( #26210 ), #2530, .F. ) ;
#8784 = DIRECTION ( 'NONE',  ( 0.000000000000000000, 0.000000000000000000, 1.000000000000000000 ) ) ;
#8785 = DIRECTION ( 'NONE',  ( -1.000000000000000000, 0.000000000000000000, -1.300283923313630633E-47 ) ) ;
#8786 = CARTESIAN_POINT ( 'NONE',  ( 0.000000000000000000, 144.9999999999999716, 194.9999999999999716 ) ) ;
#8787 = VERTEX_POINT ( 'NONE', #34585 ) ;
#8788 = AXIS2_PLACEMENT_3D ( 'NONE', #23069, #2335, #23874 ) ;
#8789 = ADVANCED_FACE ( 'NONE', ( #15736 ), #1573, .T. ) ;
#8790 = DIRECTION ( 'NONE',  ( 0.000000000000000000, 1.310824597558155437E-49, 1.000000000000000000 ) ) ;
#8791 = EDGE_CURVE ( 'NONE', #549, #18500, #2352, .T. ) ;
#8792 = CIRCLE ( 'NONE', #25839, 1.999999999999999112 ) ;
#8793 = AXIS2_PLACEMENT_3D ( 'NONE', #9114, #25656, #6432 ) ;
#8794 = DIRECTION ( 'NONE',  ( -1.000000000000000000, 0.000000000000000000, -1.300283923313630633E-47 ) ) ;
#8795 = ORIENTED_EDGE ( 'NONE', *, *, #20035, .F. ) ;
#8796 = AXIS2_PLACEMENT_3D ( 'NONE', #17075, #690, #16545 ) ;
#8797 = FACE_OUTER_BOUND ( 'NONE', #22085, .T. ) ;
#8798 = CARTESIAN_POINT ( 'NONE',  ( -349.0000000000000000, 124.9999999999999432, 164.9999999999999716 ) ) ;
#8799 = LINE ( 'NONE', #5230, #17823 ) ;
#8800 = CARTESIAN_POINT ( 'NONE',  ( -418.0000000000000000, 105.0000000000000000, 132.0000000000000000 ) ) ;
#8801 = DIRECTION ( 'NONE',  ( -1.000000000000000000, -0.000000000000000000, -0.000000000000000000 ) ) ;
#8802 = DIRECTION ( 'NONE',  ( 0.000000000000000000, -0.9048270524660176894, -0.4257792915650768228 ) ) ;
#8803 = ORIENTED_EDGE ( 'NONE', *, *, #30700, .F. ) ;
#8805 = CARTESIAN_POINT ( 'NONE',  ( -23.46927268871045058, -22.54767421130281946, -36.68877005347593467 ) ) ;
#8804 = DIRECTION ( 'NONE',  ( -0.000000000000000000, 1.836970198721029934E-16, -1.000000000000000000 ) ) ;
#8806 = AXIS2_PLACEMENT_3D ( 'NONE', #32239, #2167, #15528 ) ;
#8807 = ORIENTED_EDGE ( 'NONE', *, *, #8485, .T. ) ;
#8808 = DIRECTION ( 'NONE',  ( -0.000000000000000000, -0.000000000000000000, -1.000000000000000000 ) ) ;
#8809 = CARTESIAN_POINT ( 'NONE',  ( -23.46927268871044348, -22.54767421130285143, 68.31122994652405112 ) ) ;
#8810 = VECTOR ( 'NONE', #4878, 1000.000000000000227 ) ;
#8811 = EDGE_LOOP ( 'NONE', ( #6112, #22318, #32658, #29442 ) ) ;
#8812 = FACE_BOUND ( 'NONE', #3673, .T. ) ;
#8813 = VECTOR ( 'NONE', #15130, 1000.000000000000000 ) ;
#8814 = ORIENTED_EDGE ( 'NONE', *, *, #12666, .F. ) ;
#8815 = CARTESIAN_POINT ( 'NONE',  ( 103.0960974094320903, -5.425683864377651489, -5.182047996533464485 ) ) ;
#8816 = DIRECTION ( 'NONE',  ( -1.000000000000000000, 0.000000000000000000, 0.000000000000000000 ) ) ;
#8817 = VERTEX_POINT ( 'NONE', #4657 ) ;
#8818 = EDGE_LOOP ( 'NONE', ( #1777, #3697, #28289, #29176 ) ) ;
#8819 = CARTESIAN_POINT ( 'NONE',  ( 6.078604839177340402, 33.69708579775584667, -36.68877005347592757 ) ) ;
#8820 = AXIS2_PLACEMENT_3D ( 'NONE', #34239, #34591, #34416 ) ;
#8821 = DIRECTION ( 'NONE',  ( 0.000000000000000000, -1.000000000000000000, -2.309213040847544338E-50 ) ) ;
#8822 = DIRECTION ( 'NONE',  ( 0.000000000000000000, 0.000000000000000000, -1.000000000000000000 ) ) ;
#8823 = DIRECTION ( 'NONE',  ( -0.000000000000000000, 1.000000000000000000, -0.000000000000000000 ) ) ;
#8824 = ORIENTED_EDGE ( 'NONE', *, *, #27472, .T. ) ;
#8825 = ORIENTED_EDGE ( 'NONE', *, *, #11727, .F. ) ;
#8826 = EDGE_CURVE ( 'NONE', #6559, #29137, #5511, .T. ) ;
#8827 = DIRECTION ( 'NONE',  ( 0.000000000000000000, 1.000000000000000000, -3.374343856708137958E-53 ) ) ;
#8828 = CARTESIAN_POINT ( 'NONE',  ( 2.604019739527419830, 12.64393372169708130, -29.70253967906851500 ) ) ;
#8829 = DIRECTION ( 'NONE',  ( 0.000000000000000000, 0.000000000000000000, 1.000000000000000000 ) ) ;
#8830 = ADVANCED_FACE ( 'NONE', ( #29423 ), #13233, .F. ) ;
#8831 = CARTESIAN_POINT ( 'NONE',  ( -36.80830595996284416, 8.862931941313773265, 68.31122994652405112 ) ) ;
#8832 = CARTESIAN_POINT ( 'NONE',  ( 0.000000000000000000, 0.000000000000000000, 3.931000000000000494 ) ) ;
#8833 = VECTOR ( 'NONE', #22893, 1000.000000000000000 ) ;
#8834 = DIRECTION ( 'NONE',  ( -0.7621620551276363509, -0.6473862847818278032, -0.000000000000000000 ) ) ;
#8835 = EDGE_CURVE ( 'NONE', #14930, #21561, #23402, .T. ) ;
#8836 = B_SPLINE_CURVE_WITH_KNOTS ( 'NONE', 3,
 ( #14541, #19696, #471, #24838 ),
 .UNSPECIFIED., .F., .F.,
 ( 4, 4 ),
 ( 0.005298373595863127387, 0.005985241895929838650 ),
 .UNSPECIFIED. ) ;
#8837 = DIRECTION ( 'NONE',  ( -3.469446951953832974E-18, -1.000000000000000000, 7.888609052210118054E-31 ) ) ;
#8838 = VERTEX_POINT ( 'NONE', #1832 ) ;
#8839 = AXIS2_PLACEMENT_3D ( 'NONE', #25160, #30692, #5937 ) ;
#8840 = EDGE_CURVE ( 'NONE', #18883, #1235, #6664, .T. ) ;
#8841 = CIRCLE ( 'NONE', #32715, 4.000000000000003553 ) ;
#8842 = CARTESIAN_POINT ( 'NONE',  ( -430.0000000000000000, 118.9999999999999716, 126.0000000000000000 ) ) ;
#8843 = CYLINDRICAL_SURFACE ( 'NONE', #5195, 4.750000000000004441 ) ;
#8844 = DIRECTION ( 'NONE',  ( -0.000000000000000000, 1.000000000000000000, -0.000000000000000000 ) ) ;
#8845 = ORIENTED_EDGE ( 'NONE', *, *, #4752, .F. ) ;
#8846 = DIRECTION ( 'NONE',  ( -1.000000000000000000, -0.000000000000000000, -0.000000000000000000 ) ) ;
#8847 = VERTEX_POINT ( 'NONE', #7512 ) ;
#8848 = LINE ( 'NONE', #6520, #16800 ) ;
#8850 = AXIS2_PLACEMENT_3D ( 'NONE', #9639, #29019, #4615 ) ;
#8849 = CARTESIAN_POINT ( 'NONE',  ( -449.9999999999999432, -112.9999999999999858, -174.9999999999999716 ) ) ;
#8851 = ADVANCED_FACE ( 'NONE', ( #18401 ), #4844, .T. ) ;
#8852 = EDGE_CURVE ( 'NONE', #6869, #6749, #27093, .T. ) ;
#8853 = ORIENTED_EDGE ( 'NONE', *, *, #3678, .F. ) ;
#8854 = CARTESIAN_POINT ( 'NONE',  ( -35.00000000000000000, 3.353962854566122864, -15.81122994652406355 ) ) ;
#8855 = DIRECTION ( 'NONE',  ( 1.000000000000000000, 0.000000000000000000, 0.000000000000000000 ) ) ;
#8856 = CARTESIAN_POINT ( 'NONE',  ( 7.700000000000000178, 1.261386203121773722E-15, 10.30000000000000071 ) ) ;
#8857 = VERTEX_POINT ( 'NONE', #33133 ) ;
#8858 = VECTOR ( 'NONE', #28004, 1000.000000000000000 ) ;
#8859 = DIRECTION ( 'NONE',  ( 2.631201909438060269E-14, -5.396010391056495992E-16, 0.9999999999999998890 ) ) ;
#8860 = DIRECTION ( 'NONE',  ( 0.000000000000000000, 1.310824597558155437E-49, 1.000000000000000000 ) ) ;
#8861 = ORIENTED_EDGE ( 'NONE', *, *, #19938, .F. ) ;
#8862 = AXIS2_PLACEMENT_3D ( 'NONE', #18961, #27482, #8608 ) ;
#8863 = CARTESIAN_POINT ( 'NONE',  ( -1.307386931792819285, 32.51914993179681090, 68.31122994652405112 ) ) ;
#8864 = CARTESIAN_POINT ( 'NONE',  ( 0.000000000000000000, 30.93646776788796160, 7.943134866716423659 ) ) ;
#8865 = DIRECTION ( 'NONE',  ( 0.3193015301359797276, 0.9476531711828024562, -0.000000000000000000 ) ) ;
#8866 = DIRECTION ( 'NONE',  ( 0.000000000000000000, 0.000000000000000000, 1.000000000000000000 ) ) ;
#8867 = ITEM_DEFINED_TRANSFORMATION ( 'NONE', 'NONE', #3016,  #28566 ) ;
#8868 = ORIENTED_EDGE ( 'NONE', *, *, #29287, .T. ) ;
#8869 = ORIENTED_EDGE ( 'NONE', *, *, #2386, .F. ) ;
#8870 = ORIENTED_EDGE ( 'NONE', *, *, #24062, .F. ) ;
#8871 = VECTOR ( 'NONE', #30613, 1000.000000000000000 ) ;
#8872 = DIRECTION ( 'NONE',  ( 0.7621620551276372391, -0.6473862847818265820, -0.000000000000000000 ) ) ;
#8873 = FACE_OUTER_BOUND ( 'NONE', #20609, .T. ) ;
#8874 = DIRECTION ( 'NONE',  ( 0.000000000000000000, 0.000000000000000000, 1.000000000000000000 ) ) ;
#8875 = VERTEX_POINT ( 'NONE', #22288 ) ;
#8876 = ORIENTED_EDGE ( 'NONE', *, *, #4086, .T. ) ;
#8877 = DIRECTION ( 'NONE',  ( 0.000000000000000000, 1.000000000000000000, 1.224646799147353207E-16 ) ) ;
#8878 = ORIENTED_EDGE ( 'NONE', *, *, #23991, .T. ) ;
#8879 = PRODUCT_DEFINITION_SHAPE ( 'NONE', 'NONE',  #35133 ) ;
#8880 = DIRECTION ( 'NONE',  ( 1.000000000000000000, 0.000000000000000000, -1.848892746611746966E-32 ) ) ;
#8881 = EDGE_CURVE ( 'NONE', #12045, #26496, #14290, .T. ) ;
#8882 = DIRECTION ( 'NONE',  ( 3.697785493223492838E-32, 1.934419779023891545E-16, -1.000000000000000000 ) ) ;
#8883 = VERTEX_POINT ( 'NONE', #13753 ) ;
#8884 = ORIENTED_EDGE ( 'NONE', *, *, #20769, .T. ) ;
#8885 = CIRCLE ( 'NONE', #15741, 7.999999999999979572 ) ;
#8886 =( LENGTH_UNIT ( ) NAMED_UNIT ( * ) SI_UNIT ( .MILLI., .METRE. ) );
#8887 = EDGE_CURVE ( 'NONE', #13361, #35039, #22115, .T. ) ;
#8888 = EDGE_CURVE ( 'NONE', #2593, #22922, #7805, .T. ) ;
#8889 = CARTESIAN_POINT ( 'NONE',  ( 7.700000000000000178, 1.922695474661344271E-15, 15.69999999999999929 ) ) ;
#8890 = VERTEX_POINT ( 'NONE', #5893 ) ;
#8891 = AXIS2_PLACEMENT_3D ( 'NONE', #22112, #5889, #24580 ) ;
#8892 = CARTESIAN_POINT ( 'NONE',  ( 2.765921099433440666, -11.07880054387200985, -29.04985141099774637 ) ) ;
#8893 = DIRECTION ( 'NONE',  ( 0.000000000000000000, 1.000000000000000000, 0.000000000000000000 ) ) ;
#8894 = DIRECTION ( 'NONE',  ( 3.040835319149746090E-31, 1.000000000000000000, 0.000000000000000000 ) ) ;
#8895 = FACE_OUTER_BOUND ( 'NONE', #3760, .T. ) ;
#8896 = CARTESIAN_POINT ( 'NONE',  ( 2.719010718194136533, 29.95554370010558287, -10.35423322779145217 ) ) ;
#8897 = CARTESIAN_POINT ( 'NONE',  ( -12.00000000000001066, 108.9999999999999858, -175.0000000000000284 ) ) ;
#8899 = EDGE_CURVE ( 'NONE', #6409, #32490, #574, .T. ) ;
#8898 = EDGE_LOOP ( 'NONE', ( #2420, #7889, #13126, #2853 ) ) ;
#8900 = ORIENTED_EDGE ( 'NONE', *, *, #32290, .T. ) ;
#8901 = DIRECTION ( 'NONE',  ( 0.1063910735368947813, -0.9943243633099144718, -3.335902418024520312E-15 ) ) ;
#8902 = VERTEX_POINT ( 'NONE', #8931 ) ;
#8903 = EDGE_LOOP ( 'NONE', ( #33153, #31403, #27468, #31746 ) ) ;
#8904 = AXIS2_PLACEMENT_3D ( 'NONE', #26162, #31676, #23680 ) ;
#8905 = CYLINDRICAL_SURFACE ( 'NONE', #30614, 34.41491905851385269 ) ;
#8906 = EDGE_CURVE ( 'NONE', #12986, #5991, #20330, .T. ) ;
#8907 = CIRCLE ( 'NONE', #22568, 34.41491905851385269 ) ;
#8908 = EDGE_CURVE ( 'NONE', #34042, #23786, #3816, .T. ) ;
#8909 = CYLINDRICAL_SURFACE ( 'NONE', #13665, 7.999999999999952038 ) ;
#8910 = PRODUCT_CONTEXT ( 'NONE', #2351, 'mechanical' ) ;
#8911 = ORIENTED_EDGE ( 'NONE', *, *, #18421, .T. ) ;
#8912 = LINE ( 'NONE', #28136, #7090 ) ;
#8913 = DIRECTION ( 'NONE',  ( 1.000000000000000000, 0.000000000000000000, 0.000000000000000000 ) ) ;
#8914 = ITEM_DEFINED_TRANSFORMATION ( 'NONE', 'NONE', #3039,  #28566 ) ;
#8916 = CARTESIAN_POINT ( 'NONE',  ( 119.9999999999998295, 0.000000000000000000, 0.000000000000000000 ) ) ;
#8915 = DIRECTION ( 'NONE',  ( -1.000000000000000000, -0.000000000000000000, -0.000000000000000000 ) ) ;
#8917 = ORIENTED_EDGE ( 'NONE', *, *, #8999, .T. ) ;
#8918 = EDGE_LOOP ( 'NONE', ( #32736, #5494, #2818, #23655 ) ) ;
#8919 = CARTESIAN_POINT ( 'NONE',  ( -410.0000000000000568, -112.9999999999999858, 154.9999999999999716 ) ) ;
#8920 = CIRCLE ( 'NONE', #28813, 1.999999999999999556 ) ;
#8921 = DIRECTION ( 'NONE',  ( 0.000000000000000000, 1.000000000000000000, 0.000000000000000000 ) ) ;
#8922 = DIRECTION ( 'NONE',  ( 1.000000000000000000, 0.000000000000000000, -0.000000000000000000 ) ) ;
#8923 = FACE_OUTER_BOUND ( 'NONE', #24535, .T. ) ;
#8924 = ORIENTED_EDGE ( 'NONE', *, *, #576, .F. ) ;
#8925 = CARTESIAN_POINT ( 'NONE',  ( -499.9999999999999432, 136.9999999999999432, -162.9999999999999716 ) ) ;
#8926 = CARTESIAN_POINT ( 'NONE',  ( 2.261199756575918762, 31.32081674369869972, 11.57089561809684497 ) ) ;
#8927 = DIRECTION ( 'NONE',  ( 0.5155538571770231782, 0.8568571761675883858, -0.000000000000000000 ) ) ;
#8928 = EDGE_CURVE ( 'NONE', #19525, #25531, #16614, .T. ) ;
#8929 = EDGE_CURVE ( 'NONE', #5130, #20230, #15347, .T. ) ;
#8930 = ORIENTED_EDGE ( 'NONE', *, *, #23202, .F. ) ;
#8931 = CARTESIAN_POINT ( 'NONE',  ( 36.10877985260814427, 11.38239727801116352, 68.31122994652405112 ) ) ;
#8932 = AXIS2_PLACEMENT_3D ( 'NONE', #23133, #18625, #12931 ) ;
#8933 = DIRECTION ( 'NONE',  ( 1.000000000000000000, 0.000000000000000000, 0.000000000000000000 ) ) ;
#8934 = EDGE_CURVE ( 'NONE', #25561, #25012, #14109, .T. ) ;
#8935 = FACE_OUTER_BOUND ( 'NONE', #28140, .T. ) ;
#8937 = DIRECTION ( 'NONE',  ( -0.000000000000000000, -0.000000000000000000, 1.000000000000000000 ) ) ;
#8936 = CARTESIAN_POINT ( 'NONE',  ( 11.99999999999999645, -115.0000000000000000, -162.9999999999999432 ) ) ;
#8938 = VECTOR ( 'NONE', #5975, 1000.000000000000000 ) ;
#8939 = AXIS2_PLACEMENT_3D ( 'NONE', #30824, #6423, #17321 ) ;
#8940 = UNCERTAINTY_MEASURE_WITH_UNIT (LENGTH_MEASURE( 1.000000000000000082E-05 ), #8886, 'distance_accuracy_value', 'NONE');
#8941 = CARTESIAN_POINT ( 'NONE',  ( -1.155000000000000027, 0.000000000000000000, 4.679999999999999716 ) ) ;
#8942 = ORIENTED_EDGE ( 'NONE', *, *, #11091, .T. ) ;
#8943 = CARTESIAN_POINT ( 'NONE',  ( -418.0000000000000000, -137.0000000000000000, -155.0000000000000000 ) ) ;
#8944 = LINE ( 'NONE', #19816, #15535 ) ;
#8945 = AXIS2_PLACEMENT_3D ( 'NONE', #13829, #13478, #24313 ) ;
#8946 = ORIENTED_EDGE ( 'NONE', *, *, #13711, .T. ) ;
#8947 = EDGE_LOOP ( 'NONE', ( #33352, #10310, #5219, #18601, #4901, #33551, #8078, #14686 ) ) ;
#8948 = EDGE_CURVE ( 'NONE', #16070, #8857, #33964, .T. ) ;
#8949 = EDGE_CURVE ( 'NONE', #23519, #4330, #6816, .T. ) ;
#8950 = AXIS2_PLACEMENT_3D ( 'NONE', #1694, #20568, #31247 ) ;
#8951 = VERTEX_POINT ( 'NONE', #24413 ) ;
#8952 = TOROIDAL_SURFACE ( 'NONE', #27064, 30.47050528711511674, 8.000000000000000000 ) ;
#8953 = CARTESIAN_POINT ( 'NONE',  ( -35.00000000000000711, 28.28427124746189847, -36.68877005347593467 ) ) ;
#8954 = ORIENTED_EDGE ( 'NONE', *, *, #25706, .T. ) ;
#8955 = ORIENTED_EDGE ( 'NONE', *, *, #10312, .F. ) ;
#8956 = DIRECTION ( 'NONE',  ( 0.000000000000000000, -2.309213040847544338E-50, -1.000000000000000000 ) ) ;
#8957 = EDGE_CURVE ( 'NONE', #23973, #7721, #4373, .T. ) ;
#8958 = AXIS2_PLACEMENT_3D ( 'NONE', #5535, #5706, #8401 ) ;
#8959 = VECTOR ( 'NONE', #19764, 1000.000000000000000 ) ;
#8960 = ADVANCED_FACE ( 'NONE', ( #3406 ), #19451, .F. ) ;
#8961 = ORIENTED_EDGE ( 'NONE', *, *, #20528, .T. ) ;
#8962 = CARTESIAN_POINT ( 'NONE',  ( -445.9999999999999432, 113.0000000000000000, 154.9999999999999716 ) ) ;
#8963 = FACE_OUTER_BOUND ( 'NONE', #21642, .T. ) ;
#8964 = ORIENTED_EDGE ( 'NONE', *, *, #12070, .T. ) ;
#8965 = ORIENTED_EDGE ( 'NONE', *, *, #12068, .T. ) ;
#8966 =( REPRESENTATION_RELATIONSHIP ('NONE','NONE', #23037, #15767 ) REPRESENTATION_RELATIONSHIP_WITH_TRANSFORMATION ( #17818 )SHAPE_REPRESENTATION_RELATIONSHIP( ) );
#8967 = CARTESIAN_POINT ( 'NONE',  ( 19.99999999999998224, 134.9999999999998863, 187.0000000000000000 ) ) ;
#8968 = EDGE_CURVE ( 'NONE', #28789, #1722, #26563, .T. ) ;
#8969 = FACE_OUTER_BOUND ( 'NONE', #21598, .T. ) ;
#8970 = CARTESIAN_POINT ( 'NONE',  ( 0.02407890056655651728, 18.59128259035506758, -24.91982945642901726 ) ) ;
#8971 = DIRECTION ( 'NONE',  ( 0.000000000000000000, 0.000000000000000000, 1.000000000000000000 ) ) ;
#8972 = CARTESIAN_POINT ( 'NONE',  ( -20.63749999999999574, 0.000000000000000000, 0.000000000000000000 ) ) ;
#8973 = ORIENTED_EDGE ( 'NONE', *, *, #1463, .F. ) ;
#8974 = AXIS2_PLACEMENT_3D ( 'NONE', #20571, #7196, #18098 ) ;
#8975 = CARTESIAN_POINT ( 'NONE',  ( -35.00000000000000000, -14.38258422898373112, -21.76353962326704661 ) ) ;
#8976 = CARTESIAN_POINT ( 'NONE',  ( 0.1835381908571713794, -3.232363112765380464, -32.10887868571001746 ) ) ;
#8977 = VERTEX_POINT ( 'NONE', #30117 ) ;
#8978 = CARTESIAN_POINT ( 'NONE',  ( 20.62763069236413926, -31.74750072459299588, 68.31122994652405112 ) ) ;
#8979 = CARTESIAN_POINT ( 'NONE',  ( 0.001366356357610495681, -26.04873650956165676, -16.24881338200997760 ) ) ;
#8980 = FACE_OUTER_BOUND ( 'NONE', #14185, .T. ) ;
#8981 = CARTESIAN_POINT ( 'NONE',  ( -35.00000000000000000, -38.34433698000722046, 36.69637551990492597 ) ) ;
#8982 = PLANE ( 'NONE',  #21333 ) ;
#8983 = AXIS2_PLACEMENT_3D ( 'NONE', #19834, #6628, #20179 ) ;
#8984 = CARTESIAN_POINT ( 'NONE',  ( 0.000000000000000000, 0.000000000000000000, 0.000000000000000000 ) ) ;
#8985 = VERTEX_POINT ( 'NONE', #5710 ) ;
#8986 = ADVANCED_FACE ( 'NONE', ( #3057 ), #13930, .T. ) ;
#8987 = DIRECTION ( 'NONE',  ( 0.000000000000000000, 0.000000000000000000, -1.000000000000000000 ) ) ;
#8989 = DIRECTION ( 'NONE',  ( 0.000000000000000000, 0.000000000000000000, 1.000000000000000000 ) ) ;
#8988 = CARTESIAN_POINT ( 'NONE',  ( 2.606462025418759598, 26.80070150627962633, -17.97639020990277459 ) ) ;
#8990 = VECTOR ( 'NONE', #14810, 1000.000000000000000 ) ;
#8991 = CIRCLE ( 'NONE', #16986, 3.999999999999976019 ) ;
#8992 = ORIENTED_EDGE ( 'NONE', *, *, #10903, .F. ) ;
#8993 = DIRECTION ( 'NONE',  ( -1.000000000000000000, -0.000000000000000000, -0.000000000000000000 ) ) ;
#8994 = CARTESIAN_POINT ( 'NONE',  ( 0.000000000000000000, 2.296212748401288367E-15, 47.49999999999999289 ) ) ;
#8995 = EDGE_CURVE ( 'NONE', #17552, #28037, #26007, .T. ) ;
#8996 = VERTEX_POINT ( 'NONE', #6776 ) ;
#8997 = ORIENTED_EDGE ( 'NONE', *, *, #19932, .T. ) ;
#8998 = AXIS2_PLACEMENT_3D ( 'NONE', #22848, #14681, #15191 ) ;
#8999 = EDGE_CURVE ( 'NONE', #21282, #17861, #15791, .T. ) ;
#9000 = EDGE_CURVE ( 'NONE', #14417, #16671, #14815, .T. ) ;
#9001 = ORIENTED_EDGE ( 'NONE', *, *, #20522, .F. ) ;
#9002 = DIRECTION ( 'NONE',  ( 0.000000000000000000, 1.131431318426415506E-52, 1.000000000000000000 ) ) ;
#9003 = EDGE_LOOP ( 'NONE', ( #25021, #22402, #12918, #7532 ) ) ;
#9004 = ORIENTED_EDGE ( 'NONE', *, *, #6942, .T. ) ;
#9005 = DIRECTION ( 'NONE',  ( 1.000000000000000000, 0.000000000000000000, -5.546364386991661285E-52 ) ) ;
#9006 = CIRCLE ( 'NONE', #31807, 32.54542015209056416 ) ;
#9007 = DIRECTION ( 'NONE',  ( 0.000000000000000000, 0.000000000000000000, -1.000000000000000000 ) ) ;
#9008 = AXIS2_PLACEMENT_3D ( 'NONE', #10722, #21572, #32411 ) ;
#9009 = DIRECTION ( 'NONE',  ( 1.000000000000000000, 0.000000000000000000, -0.000000000000000000 ) ) ;
#9010 = DIRECTION ( 'NONE',  ( -1.000000000000000000, 0.000000000000000000, 1.848892746611746966E-32 ) ) ;
#9011 = ORIENTED_EDGE ( 'NONE', *, *, #17660, .T. ) ;
#9012 = ORIENTED_EDGE ( 'NONE', *, *, #33578, .F. ) ;
#9013 = CARTESIAN_POINT ( 'NONE',  ( -27.76765758629847269, -16.97532223688794417, 68.31122994652405112 ) ) ;
#9014 = DIRECTION ( 'NONE',  ( 0.000000000000000000, -1.000000000000000000, -2.132064625830773463E-16 ) ) ;
#9015 = DIRECTION ( 'NONE',  ( 1.000000000000000000, 0.000000000000000000, -0.000000000000000000 ) ) ;
#9016 = CARTESIAN_POINT ( 'NONE',  ( 11.99999999999999645, 144.9999999999999716, -186.9999999999999716 ) ) ;
#9017 = DIRECTION ( 'NONE',  ( -1.000000000000000000, -0.000000000000000000, -0.000000000000000000 ) ) ;
#9018 = AXIS2_PLACEMENT_3D ( 'NONE', #6712, #4384, #25580 ) ;
#9019 = CARTESIAN_POINT ( 'NONE',  ( 0.000000000000000000, -20.35927063852789232, -22.08513060777193004 ) ) ;
#9020 = LINE ( 'NONE', #3835, #13023 ) ;
#9021 = EDGE_LOOP ( 'NONE', ( #5778, #11626, #6399, #4547 ) ) ;
#9022 = CARTESIAN_POINT ( 'NONE',  ( -500.0000000000000000, -137.0000000000000000, 155.0000000000000000 ) ) ;
#9023 = CARTESIAN_POINT ( 'NONE',  ( 0.07098932867738322328, 28.92461259213117586, -12.95806963937394762 ) ) ;
#9024 = CYLINDRICAL_SURFACE ( 'NONE', #2413, 4.750000000000004441 ) ;
#9025 = ORIENTED_EDGE ( 'NONE', *, *, #21585, .T. ) ;
#9026 = FACE_OUTER_BOUND ( 'NONE', #1019, .T. ) ;
#9027 = ORIENTED_EDGE ( 'NONE', *, *, #18044, .T. ) ;
#9028 = SURFACE_SIDE_STYLE ('',( #22563 ) ) ;
#9029 = DIRECTION ( 'NONE',  ( 0.000000000000000000, 1.224646799147353207E-16, -1.000000000000000000 ) ) ;
#9030 = CIRCLE ( 'NONE', #28916, 2.033421858999711951 ) ;
#9031 = ORIENTED_EDGE ( 'NONE', *, *, #33228, .F. ) ;
#9032 = CARTESIAN_POINT ( 'NONE',  ( 7.647434771771126672E-16, -7.837340408380152112, 29.64303704467396017 ) ) ;
#9033 = DIRECTION ( 'NONE',  ( -0.000000000000000000, -0.000000000000000000, 1.000000000000000000 ) ) ;
#9034 = CARTESIAN_POINT ( 'NONE',  ( -449.9999999999999432, 105.0000000000000142, -77.99999999999997158 ) ) ;
#9035 = EDGE_CURVE ( 'NONE', #25337, #35075, #21466, .T. ) ;
#9036 = EDGE_LOOP ( 'NONE', ( #23182, #101, #10298, #32927 ) ) ;
#9037=STYLED_ITEM('',(#35275),#10712);
#9038 = EDGE_CURVE ( 'NONE', #26426, #14044, #15163, .T. ) ;
#9039 = DIRECTION ( 'NONE',  ( 2.631201909438060585E-14, -5.396010391056496978E-16, 1.000000000000000000 ) ) ;
#9040 = DIRECTION ( 'NONE',  ( -1.000000000000000000, -0.000000000000000000, 0.000000000000000000 ) ) ;
#9041 = ADVANCED_FACE ( 'NONE', ( #34013 ), #25473, .F. ) ;
#9042 = VERTEX_POINT ( 'NONE', #1102 ) ;
#9043 = DIRECTION ( 'NONE',  ( -1.000000000000000000, -0.000000000000000000, -0.000000000000000000 ) ) ;
#9044 = VECTOR ( 'NONE', #25918, 1000.000000000000000 ) ;
#9045 = CARTESIAN_POINT ( 'NONE',  ( 2.719051661423419475, -31.66307346108433052, 1.400387680933883328 ) ) ;
#9046 = DIRECTION ( 'NONE',  ( -0.000000000000000000, -1.000000000000000000, -0.000000000000000000 ) ) ;
#9047 = DIRECTION ( 'NONE',  ( 0.000000000000000000, 0.000000000000000000, 1.000000000000000000 ) ) ;
#9048 = EDGE_LOOP ( 'NONE', ( #24737, #16653, #22932, #10755, #16559, #4994, #19193, #31457, #11567 ) ) ;
#9049 = ORIENTED_EDGE ( 'NONE', *, *, #13553, .F. ) ;
#9050 = ORIENTED_EDGE ( 'NONE', *, *, #3846, .T. ) ;
#9051 =( NAMED_UNIT ( * ) PLANE_ANGLE_UNIT ( ) SI_UNIT ( $, .RADIAN. ) );
#9052 = EDGE_CURVE ( 'NONE', #31799, #32157, #22649, .T. ) ;
#9053 = DIRECTION ( 'NONE',  ( 0.000000000000000000, 1.836970198721029441E-16, -1.000000000000000000 ) ) ;
#9054 = DIRECTION ( 'NONE',  ( -1.000000000000000000, -0.000000000000000000, -0.000000000000000000 ) ) ;
#9055 = AXIS2_PLACEMENT_3D ( 'NONE', #19442, #5884, #24574 ) ;
#9056 = CARTESIAN_POINT ( 'NONE',  ( 0.006871054653494480455, 14.58967697705840827, -27.20420702726686102 ) ) ;
#9057 = VERTEX_POINT ( 'NONE', #1618 ) ;
#9058 = ORIENTED_EDGE ( 'NONE', *, *, #22055, .F. ) ;
#9059 = CARTESIAN_POINT ( 'NONE',  ( -7.700000000000000178, 0.000000000000000000, 0.000000000000000000 ) ) ;
#9060 = DIRECTION ( 'NONE',  ( 0.000000000000000000, 0.000000000000000000, 1.000000000000000000 ) ) ;
#9061 = ORIENTED_EDGE ( 'NONE', *, *, #31648, .T. ) ;
#9062 = DIRECTION ( 'NONE',  ( 3.697785493223492838E-32, 1.934419779023891545E-16, -1.000000000000000000 ) ) ;
#9063 = DIRECTION ( 'NONE',  ( -1.000000000000000000, -0.000000000000000000, -0.000000000000000000 ) ) ;
#9064 = ORIENTED_EDGE ( 'NONE', *, *, #22865, .T. ) ;
#9065 = AXIS2_PLACEMENT_3D ( 'NONE', #15626, #26459, #23796 ) ;
#9066 = VERTEX_POINT ( 'NONE', #31176 ) ;
#9067 = DIRECTION ( 'NONE',  ( -1.000000000000000000, 0.000000000000000000, 0.000000000000000000 ) ) ;
#9068 = DIRECTION ( 'NONE',  ( 1.000000000000000000, 0.000000000000000000, 0.000000000000000000 ) ) ;
#9069 = ORIENTED_EDGE ( 'NONE', *, *, #17948, .F. ) ;
#9070 = FACE_OUTER_BOUND ( 'NONE', #33542, .T. ) ;
#9071 = PLANE ( 'NONE',  #7483 ) ;
#9072 = DIRECTION ( 'NONE',  ( -1.000000000000000000, 0.000000000000000000, -0.000000000000000000 ) ) ;
#9073 = CIRCLE ( 'NONE', #8506, 2.000000000000001776 ) ;
#9074 = CARTESIAN_POINT ( 'NONE',  ( -107.5741775841794095, -4.432411119407283273, 11.68939833797860395 ) ) ;
#9075 = CARTESIAN_POINT ( 'NONE',  ( -361.0000000000000000, -125.0000000000000284, 181.0000000000000000 ) ) ;
#9076 = EDGE_CURVE ( 'NONE', #21855, #26665, #26001, .T. ) ;
#9077 = ORIENTED_EDGE ( 'NONE', *, *, #31570, .F. ) ;
#9078 = VECTOR ( 'NONE', #2866, 1000.000000000000000 ) ;
#9079 = ORIENTED_EDGE ( 'NONE', *, *, #8929, .F. ) ;
#9080 = CARTESIAN_POINT ( 'NONE',  ( 852.7739704483359446, 977.1998846704070729, 1753.598338701303192 ) ) ;
#9081 = ADVANCED_FACE ( 'NONE', ( #31000 ), #33487, .T. ) ;
#9082 = ORIENTED_EDGE ( 'NONE', *, *, #5390, .T. ) ;
#9083 = VERTEX_POINT ( 'NONE', #23332 ) ;
#9084 = ADVANCED_FACE ( 'NONE', ( #34185 ), #20491, .T. ) ;
#9085 = LINE ( 'NONE', #33293, #6713 ) ;
#9086 = EDGE_CURVE ( 'NONE', #34350, #31695, #29419, .T. ) ;
#9087 = DIRECTION ( 'NONE',  ( -1.000000000000000000, -0.000000000000000000, -0.000000000000000000 ) ) ;
#9088 = ADVANCED_FACE ( 'NONE', ( #1449 ), #11799, .T. ) ;
#9089 = EDGE_LOOP ( 'NONE', ( #3233, #23049, #12736, #34475, #4519, #4512, #1182, #10642 ) ) ;
#9090 = CARTESIAN_POINT ( 'NONE',  ( -442.0000000000000000, 104.9999999999999858, -187.0000000000000000 ) ) ;
#9091 =( NAMED_UNIT ( * ) SI_UNIT ( $, .STERADIAN. ) SOLID_ANGLE_UNIT ( ) );
#9092 = EDGE_CURVE ( 'NONE', #5761, #30633, #17839, .T. ) ;
#9093 = AXIS2_PLACEMENT_3D ( 'NONE', #1383, #14752, #25575 ) ;
#9095 = CARTESIAN_POINT ( 'NONE',  ( 2.789999999999999147, -29.63162325403014208, -6.967017504692083918 ) ) ;
#9094 = CARTESIAN_POINT ( 'NONE',  ( 19.99999999999998934, -145.0000000000000000, 162.9999999999999716 ) ) ;
#9096 = VERTEX_POINT ( 'NONE', #9634 ) ;
#9097 = ORIENTED_EDGE ( 'NONE', *, *, #3946, .F. ) ;
#9098 = DIRECTION ( 'NONE',  ( -0.000000000000000000, -1.000000000000000000, -0.000000000000000000 ) ) ;
#9099 = CARTESIAN_POINT ( 'NONE',  ( -37.85301660235036536, 0.7430237821112573027, 68.31122994652405112 ) ) ;
#9100 = DIRECTION ( 'NONE',  ( 0.000000000000000000, -1.000000000000000000, 0.000000000000000000 ) ) ;
#9101 = DIRECTION ( 'NONE',  ( 0.000000000000000000, 1.131431318426415506E-52, 1.000000000000000000 ) ) ;
#9102 = EDGE_LOOP ( 'NONE', ( #8079, #32276, #3620, #6862, #5560, #12250, #19867, #26518 ) ) ;
#9103 = DIRECTION ( 'NONE',  ( -1.000000000000000000, 0.000000000000000000, -0.000000000000000000 ) ) ;
#9104 = CARTESIAN_POINT ( 'NONE',  ( -6.500000000000000000, 0.000000000000000000, 3.180000000000000160 ) ) ;
#9105 = ORIENTED_EDGE ( 'NONE', *, *, #31119, .F. ) ;
#9106 = DIRECTION ( 'NONE',  ( -0.000000000000000000, 1.836970198721029934E-16, -1.000000000000000000 ) ) ;
#9107 = DIRECTION ( 'NONE',  ( -1.000000000000000000, 0.000000000000000000, 0.000000000000000000 ) ) ;
#9108 = CARTESIAN_POINT ( 'NONE',  ( 19.99999999999998934, -115.0000000000000000, -155.0000000000000284 ) ) ;
#9110 = CARTESIAN_POINT ( 'NONE',  ( -143.0000000000000568, -78.33668825982573480, -63.00000000000000000 ) ) ;
#9109 = FACE_OUTER_BOUND ( 'NONE', #31764, .T. ) ;
#9111 = DIRECTION ( 'NONE',  ( -1.000000000000000000, 0.000000000000000000, 0.000000000000000000 ) ) ;
#9112 = CARTESIAN_POINT ( 'NONE',  ( 0.5248941919440579529, -23.79505697368676209, 23.40952781232645918 ) ) ;
#9113 = EDGE_LOOP ( 'NONE', ( #7463, #9681, #19053, #14479 ) ) ;
#9114 = CARTESIAN_POINT ( 'NONE',  ( -5.210000000000000853, 0.000000000000000000, 0.000000000000000000 ) ) ;
#9115 = CARTESIAN_POINT ( 'NONE',  ( 0.006871166293030922176, 11.66139262930058962, 28.58215465626868834 ) ) ;
#9116 = VECTOR ( 'NONE', #33112, 1000.000000000000000 ) ;
#9117 = EDGE_LOOP ( 'NONE', ( #1674, #2503, #685, #20378 ) ) ;
#9118 = ORIENTED_EDGE ( 'NONE', *, *, #11509, .T. ) ;
#9119 = VECTOR ( 'NONE', #20275, 1000.000000000000000 ) ;
#9120 = EDGE_CURVE ( 'NONE', #34290, #10259, #6945, .T. ) ;
#9121 = EDGE_CURVE ( 'NONE', #18796, #29323, #12382, .T. ) ;
#9122 = ORIENTED_EDGE ( 'NONE', *, *, #33628, .T. ) ;
#9123 = CARTESIAN_POINT ( 'NONE',  ( 19.99999999999998934, -145.0000000000000000, 187.0000000000000000 ) ) ;
#9124 = ORIENTED_EDGE ( 'NONE', *, *, #30126, .T. ) ;
#9125 = ORIENTED_EDGE ( 'NONE', *, *, #25006, .F. ) ;
#9126 = CARTESIAN_POINT ( 'NONE',  ( -12.00000000000001066, 134.9999999999998863, 155.0000000000000000 ) ) ;
#9127 = ORIENTED_EDGE ( 'NONE', *, *, #22428, .T. ) ;
#9128 = DIRECTION ( 'NONE',  ( -0.000000000000000000, -0.000000000000000000, -1.000000000000000000 ) ) ;
#9129 = FACE_OUTER_BOUND ( 'NONE', #25219, .T. ) ;
#9130 = ORIENTED_EDGE ( 'NONE', *, *, #2514, .F. ) ;
#9131 = ORIENTED_EDGE ( 'NONE', *, *, #7533, .T. ) ;
#9132 = CARTESIAN_POINT ( 'NONE',  ( -6.500000000000000000, 0.000000000000000000, 4.679999999999999716 ) ) ;
#9134 = DIRECTION ( 'NONE',  ( -0.9289767198167918627, 0.3701381553399132329, 6.799327607689958420E-17 ) ) ;
#9133 = VECTOR ( 'NONE', #25196, 1000.000000000000000 ) ;
#9135 = CARTESIAN_POINT ( 'NONE',  ( -500.0000000000000000, 112.9999999999999574, 155.0000000000000000 ) ) ;
#9137 = EDGE_CURVE ( 'NONE', #5761, #469, #16938, .T. ) ;
#9136 = CARTESIAN_POINT ( 'NONE',  ( 5.021133111224679091, 28.08988295778447508, -67.50000000000000000 ) ) ;
#9138 = DIRECTION ( 'NONE',  ( 1.000000000000000000, 0.000000000000000000, -0.000000000000000000 ) ) ;
#9139 = ORIENTED_EDGE ( 'NONE', *, *, #9673, .T. ) ;
#9140 = AXIS2_PLACEMENT_3D ( 'NONE', #25229, #13124, #10266 ) ;
#9141 = CARTESIAN_POINT ( 'NONE',  ( 19.99999999999998934, -32.99999999999997158, -154.9999999999999716 ) ) ;
#9142 = DIRECTION ( 'NONE',  ( 0.000000000000000000, -1.000000000000000000, 0.000000000000000000 ) ) ;
#9143 = EDGE_LOOP ( 'NONE', ( #11380, #17826, #25441, #7077, #7234, #9240 ) ) ;
#9144 = CARTESIAN_POINT ( 'NONE',  ( 0.5248942741096497278, -32.12939361471808297, 9.050569439367455615 ) ) ;
#9146 = ADVANCED_FACE ( 'NONE', ( #26524, #12664 ), #10331, .F. ) ;
#9145 = CARTESIAN_POINT ( 'NONE',  ( 0.000000000000000000, 23.53611639059741378, -19.35207786518964213 ) ) ;
#9147 = CARTESIAN_POINT ( 'NONE',  ( -5.021133111225092982, -11.61907005722761177, -87.50000000000000000 ) ) ;
#9148 = ADVANCED_FACE ( 'NONE', ( #4976 ), #7650, .F. ) ;
#9149 = CARTESIAN_POINT ( 'NONE',  ( 101.5050109452463403, 4.564908081027950537, -5.956352141036524550 ) ) ;
#9150 = DIRECTION ( 'NONE',  ( -0.000000000000000000, -0.000000000000000000, -1.000000000000000000 ) ) ;
#9151 = EDGE_CURVE ( 'NONE', #22010, #5671, #29203, .T. ) ;
#9152 = VECTOR ( 'NONE', #16962, 1000.000000000000000 ) ;
#9153 = AXIS2_PLACEMENT_3D ( 'NONE', #12764, #9563, #18280 ) ;
#9154 = CARTESIAN_POINT ( 'NONE',  ( 2.789999999999999147, 12.39602498911182593, -27.80127684205855942 ) ) ;
#9155 = B_SPLINE_CURVE_WITH_KNOTS ( 'NONE', 3,
 ( #30358, #13748, #16260, #24769, #5367, #10559 ),
 .UNSPECIFIED., .F., .F.,
 ( 4, 2, 4 ),
 ( 4.404817204422397961E-07, 0.001874269756547598462, 0.003748099031374754753 ),
 .UNSPECIFIED. ) ;
#9157 = VERTEX_POINT ( 'NONE', #18548 ) ;
#9156=STYLED_ITEM('',(#35282),#33646);
#9158 = CARTESIAN_POINT ( 'NONE',  ( 10.17231796313411429, 13.56412600238610189, -77.50000000000000000 ) ) ;
#9160 = CARTESIAN_POINT ( 'NONE',  ( 0.000000000000000000, 3.524919873834583163E-15, 68.31122994652405112 ) ) ;
#9159 = CARTESIAN_POINT ( 'NONE',  ( -5.614556921127968003, -37.45022281665699637, 68.31122994652405112 ) ) ;
#9161 = EDGE_CURVE ( 'NONE', #19763, #32511, #22588, .T. ) ;
#9162 = ORIENTED_EDGE ( 'NONE', *, *, #3950, .F. ) ;
#9163 = LINE ( 'NONE', #30880, #9184 ) ;
#9164 = VECTOR ( 'NONE', #1654, 1000.000000000000000 ) ;
#9165 = ORIENTED_EDGE ( 'NONE', *, *, #19121, .T. ) ;
#9166 = VERTEX_POINT ( 'NONE', #13020 ) ;
#9167 = CIRCLE ( 'NONE', #22230, 30.47050528711511674 ) ;
#9168 = ADVANCED_FACE ( 'NONE', ( #13191 ), #15505, .T. ) ;
#9169 = ORIENTED_EDGE ( 'NONE', *, *, #33540, .T. ) ;
#9170 = CARTESIAN_POINT ( 'NONE',  ( -410.0000000000000568, -124.9999999999999716, 132.0000000000000000 ) ) ;
#9171 = ORIENTED_EDGE ( 'NONE', *, *, #8835, .T. ) ;
#9172 = ORIENTED_EDGE ( 'NONE', *, *, #9581, .T. ) ;
#9173 = CARTESIAN_POINT ( 'NONE',  ( 9.199999999999999289, 11.69134295108991317, -6.750000000000016875 ) ) ;
#9174 = PRODUCT_DEFINITION_SHAPE ( 'NONE', 'NONE',  #35189 ) ;
#9175 = CYLINDRICAL_SURFACE ( 'NONE', #31765, 2.525000000000001243 ) ;
#9176 = PLANE ( 'NONE',  #5462 ) ;
#9177 = CIRCLE ( 'NONE', #6873, 7.999999999999979572 ) ;
#9178 = DIRECTION ( 'NONE',  ( -0.000000000000000000, 0.000000000000000000, -1.000000000000000000 ) ) ;
#9179 = ORIENTED_EDGE ( 'NONE', *, *, #17332, .T. ) ;
#9180 = VERTEX_POINT ( 'NONE', #5150 ) ;
#9181 = AXIS2_PLACEMENT_3D ( 'NONE', #12812, #28987, #1587 ) ;
#9182 = CARTESIAN_POINT ( 'NONE',  ( -410.0000000000000568, -125.0000000000000000, 187.0000000000000000 ) ) ;
#9183 = PLANE ( 'NONE',  #24848 ) ;
#9184 = VECTOR ( 'NONE', #2934, 1000.000000000000000 ) ;
#9185 = PRESENTATION_LAYER_ASSIGNMENT (  '', '', ( #33623 ) ) ;
#9186 = DIRECTION ( 'NONE',  ( -0.000000000000000000, 1.000000000000000000, -0.000000000000000000 ) ) ;
#9187 = DIRECTION ( 'NONE',  ( -1.000000000000000000, 0.000000000000000000, 0.000000000000000000 ) ) ;
#9188 = DIRECTION ( 'NONE',  ( 0.000000000000000000, -1.000000000000000000, 3.374343856708137958E-53 ) ) ;
#9189 = LINE ( 'NONE', #1010, #19655 ) ;
#9190 = PLANE ( 'NONE',  #19831 ) ;
#9191 = ORIENTED_EDGE ( 'NONE', *, *, #17768, .T. ) ;
#9192 = B_SPLINE_CURVE_WITH_KNOTS ( 'NONE', 3,
 ( #31787, #17952, #6871, #4376 ),
 .UNSPECIFIED., .F., .F.,
 ( 4, 4 ),
 ( 2.702373194995081723E-07, 0.0006880065385067430078 ),
 .UNSPECIFIED. ) ;
#9193 = DIRECTION ( 'NONE',  ( 0.9985334138511239299, -0.05413890858541752643, -0.000000000000000000 ) ) ;
#9194 = CARTESIAN_POINT ( 'NONE',  ( -70.00000000000000000, 75.55999999999990280, 172.9900000000000091 ) ) ;
#9195 = VECTOR ( 'NONE', #10007, 1000.000000000000000 ) ;
#9196 = EDGE_CURVE ( 'NONE', #25155, #23608, #8402, .T. ) ;
#9197 = PLANE ( 'NONE',  #13231 ) ;
#9198 = ORIENTED_EDGE ( 'NONE', *, *, #13058, .T. ) ;
#9199 = ADVANCED_FACE ( 'NONE', ( #4796 ), #35079, .F. ) ;
#9200 = DIRECTION ( 'NONE',  ( 1.000000000000000000, 0.000000000000000000, 1.300283923313630633E-47 ) ) ;
#9201 = EDGE_LOOP ( 'NONE', ( #10758, #13153, #14179, #4391 ) ) ;
#9202 = FILL_AREA_STYLE_COLOUR ( '', #5377 ) ;
#9203 = DIRECTION ( 'NONE',  ( 0.000000000000000000, -0.000000000000000000, -1.000000000000000000 ) ) ;
#9204 = VECTOR ( 'NONE', #3200, 1000.000000000000000 ) ;
#9206 = ORIENTED_EDGE ( 'NONE', *, *, #20665, .F. ) ;
#9205 = VECTOR ( 'NONE', #3838, 1000.000000000000114 ) ;
#9207 = AXIS2_PLACEMENT_3D ( 'NONE', #20595, #34465, #17951 ) ;
#9208 = CARTESIAN_POINT ( 'NONE',  ( -445.9999999999999432, -125.0000000000000000, 107.9999999999999858 ) ) ;
#9209 = AXIS2_PLACEMENT_3D ( 'NONE', #33793, #3875, #19750 ) ;
#9210 = DIRECTION ( 'NONE',  ( -1.000000000000000000, 0.000000000000000000, 0.000000000000000000 ) ) ;
#9211 = CARTESIAN_POINT ( 'NONE',  ( -445.9999999999999432, 105.0000000000000142, -101.9999999999999858 ) ) ;
#9212 = VECTOR ( 'NONE', #30435, 1000.000000000000000 ) ;
#9213 = ORIENTED_EDGE ( 'NONE', *, *, #2461, .T. ) ;
#9214 = CARTESIAN_POINT ( 'NONE',  ( 781.5882212615997560, 1107.084089814588197, 1753.598338701303419 ) ) ;
#9215 = CARTESIAN_POINT ( 'NONE',  ( -15.99999999999998579, 75.55999999999990280, 177.7400000000000091 ) ) ;
#9216 = VERTEX_POINT ( 'NONE', #4610 ) ;
#9217 = DIRECTION ( 'NONE',  ( 0.6473862847818266930, 0.7621620551276372391, 1.400068981865444109E-16 ) ) ;
#9218 = CARTESIAN_POINT ( 'NONE',  ( -35.00000000000000000, 0.000000000000000000, 0.000000000000000000 ) ) ;
#9219 = CARTESIAN_POINT ( 'NONE',  ( -130.6469666100234406, 6.000000000000000000, -62.49999999999999289 ) ) ;
#9220 = DIRECTION ( 'NONE',  ( -1.000000000000000000, 0.000000000000000000, 0.000000000000000000 ) ) ;
#9221 = CONTEXT_DEPENDENT_SHAPE_REPRESENTATION ( #14226, #12913 ) ;
#9222 = VERTEX_POINT ( 'NONE', #4446 ) ;
#9224 = ORIENTED_EDGE ( 'NONE', *, *, #34025, .F. ) ;
#9223 =( REPRESENTATION_RELATIONSHIP ('NONE','NONE', #23037, #28231 ) REPRESENTATION_RELATIONSHIP_WITH_TRANSFORMATION ( #8428 )SHAPE_REPRESENTATION_RELATIONSHIP( ) );
#9225 = EDGE_LOOP ( 'NONE', ( #25932, #27080, #20555, #24426, #29238, #22489 ) ) ;
#9226 = CARTESIAN_POINT ( 'NONE',  ( -19.99999999999998934, -134.9999999999999716, 187.0000000000000000 ) ) ;
#9227 = FACE_OUTER_BOUND ( 'NONE', #28123, .T. ) ;
#9228 = CIRCLE ( 'NONE', #33101, 2.525000000000001688 ) ;
#9229 = DIRECTION ( 'NONE',  ( 0.000000000000000000, 0.000000000000000000, 1.000000000000000000 ) ) ;
#9230 = CARTESIAN_POINT ( 'NONE',  ( 10.17231796313409298, 4.274639749586563120, -87.50000000000000000 ) ) ;
#9231 = CIRCLE ( 'NONE', #7510, 2.525000000000002132 ) ;
#9232 = ORIENTED_EDGE ( 'NONE', *, *, #3023, .T. ) ;
#9233 = PLANE ( 'NONE',  #24246 ) ;
#9234 = VECTOR ( 'NONE', #24491, 1000.000000000000000 ) ;
#9235 = CARTESIAN_POINT ( 'NONE',  ( 55.00000000000000711, 0.000000000000000000, 0.000000000000000000 ) ) ;
#9236 = ORIENTED_EDGE ( 'NONE', *, *, #7817, .F. ) ;
#9237 = EDGE_CURVE ( 'NONE', #20173, #8317, #30568, .T. ) ;
#9238 = DIRECTION ( 'NONE',  ( 0.000000000000000000, 1.000000000000000000, 5.145227585319922065E-49 ) ) ;
#9239 = CARTESIAN_POINT ( 'NONE',  ( -42.55956070192386420, -17.65143121711728469, 20.00000000000000000 ) ) ;
#9240 = ORIENTED_EDGE ( 'NONE', *, *, #20397, .T. ) ;
#9241 = EDGE_CURVE ( 'NONE', #4681, #27224, #24018, .T. ) ;
#9242 = ORIENTED_EDGE ( 'NONE', *, *, #14817, .T. ) ;
#9243 = LINE ( 'NONE', #32911, #7777 ) ;
#9244 = ADVANCED_FACE ( 'NONE', ( #34903 ), #32035, .T. ) ;
#9245 = CARTESIAN_POINT ( 'NONE',  ( -130.6469666100234406, -6.000000000000000000, -62.49999999999999289 ) ) ;
#9246 = VERTEX_POINT ( 'NONE', #21374 ) ;
#9247 = ADVANCED_FACE ( 'NONE', ( #32219 ), #7830, .F. ) ;
#9248 = DIRECTION ( 'NONE',  ( 1.000000000000000000, 0.000000000000000000, 0.000000000000000000 ) ) ;
#9249 = DIRECTION ( 'NONE',  ( 0.000000000000000000, 0.000000000000000000, -1.000000000000000000 ) ) ;
#9250 = DIRECTION ( 'NONE',  ( 0.000000000000000000, 0.000000000000000000, -1.000000000000000000 ) ) ;
#9251 = CARTESIAN_POINT ( 'NONE',  ( -109.0610159990791175, -3.127506413740516411, 12.10571963949989005 ) ) ;
#9252 = CARTESIAN_POINT ( 'NONE',  ( 11.99999999999999645, 144.9999999999999716, -158.9999999999999716 ) ) ;
#9253 = DIRECTION ( 'NONE',  ( 0.000000000000000000, -1.000000000000000000, 0.000000000000000000 ) ) ;
#9254 = ORIENTED_EDGE ( 'NONE', *, *, #19106, .T. ) ;
#9255 = VERTEX_POINT ( 'NONE', #28845 ) ;
#9256 = AXIS2_PLACEMENT_3D ( 'NONE', #27752, #11220, #16398 ) ;
#9257 = AXIS2_PLACEMENT_3D ( 'NONE', #33498, #13942, #24952 ) ;
#9258 = DIRECTION ( 'NONE',  ( -0.1063910735369017202, 0.9943243633099136947, -1.000770725407181676E-14 ) ) ;
#9259 = VECTOR ( 'NONE', #13102, 1000.000000000000000 ) ;
#9260 = ORIENTED_EDGE ( 'NONE', *, *, #27993, .T. ) ;
#9261 = CARTESIAN_POINT ( 'NONE',  ( -365.0000000000000000, -131.0000000000000000, 126.0000000000000000 ) ) ;
#9262 = DIRECTION ( 'NONE',  ( 0.000000000000000000, 1.000000000000000000, 1.310824597558155437E-49 ) ) ;
#9263 = ITEM_DEFINED_TRANSFORMATION ( 'NONE', 'NONE', #13804,  #28566 ) ;
#9264 = VERTEX_POINT ( 'NONE', #1787 ) ;
#9265 = DIRECTION ( 'NONE',  ( -1.000000000000000000, 0.000000000000000000, 0.000000000000000000 ) ) ;
#9266 = CARTESIAN_POINT ( 'NONE',  ( -100.0523001014507827, -1.340877102867427562, -12.43231962408541769 ) ) ;
#9267 = CONTEXT_DEPENDENT_SHAPE_REPRESENTATION ( #2402, #19906 ) ;
#9268 = AXIS2_PLACEMENT_3D ( 'NONE', #26741, #23550, #1663 ) ;
#9270 = DIRECTION ( 'NONE',  ( 0.1617819965527648451, 0.9868265225415261410, 1.812770913216290044E-16 ) ) ;
#9269 = DIRECTION ( 'NONE',  ( -0.000000000000000000, -0.000000000000000000, 1.000000000000000000 ) ) ;
#9271 = ORIENTED_EDGE ( 'NONE', *, *, #11727, .T. ) ;
#9272 = ORIENTED_EDGE ( 'NONE', *, *, #7902, .T. ) ;
#9273 = CARTESIAN_POINT ( 'NONE',  ( -12.00000000000001066, -145.0000000000000000, 194.9999999999999716 ) ) ;
#9274 = EDGE_CURVE ( 'NONE', #3106, #26431, #32831, .T. ) ;
#9275 = EDGE_CURVE ( 'NONE', #14377, #25358, #7293, .T. ) ;
#9276 = CARTESIAN_POINT ( 'NONE',  ( 9.630725478591894984, 36.62364762272929397, 68.31122994652405112 ) ) ;
#9277 = FACE_BOUND ( 'NONE', #26803, .T. ) ;
#9278 = EDGE_LOOP ( 'NONE', ( #3183, #24989, #30938, #30551 ) ) ;
#9279 = AXIS2_PLACEMENT_3D ( 'NONE', #1247, #23475, #34336 ) ;
#9280 = CARTESIAN_POINT ( 'NONE',  ( -5.021133111224886036, 6.201984591278717041, -67.50000000000000000 ) ) ;
#9281 = DIRECTION ( 'NONE',  ( -1.000000000000000000, 6.792721752314501023E-48, -3.697785493223492838E-32 ) ) ;
#9282 = AXIS2_PLACEMENT_3D ( 'NONE', #33573, #9200, #30915 ) ;
#9283 = AXIS2_PLACEMENT_3D ( 'NONE', #32602, #8408, #19281 ) ;
#9284 = VERTEX_POINT ( 'NONE', #12844 ) ;
#9285 = B_SPLINE_CURVE_WITH_KNOTS ( 'NONE', 3,
 ( #24351, #32719, #21864, #5482, #7979, #27732, #13863, #156, #5304, #27555, #21687, #4253, #32536, #11371, #6005, #18863, #30060, #5827, #24702, #8158, #13683, #3171, #27377, #2816, #8516, #11198, #341, #13350, #16197, #27206, #19384, #8341, #30224, #16723, #14042, #24879, #10676, #19043, #22222, #11015, #2648, #29885, #5650, #33063 ),
 .UNSPECIFIED., .F., .F.,
 ( 4, 2, 2, 2, 2, 2, 2, 2, 2, 2, 2, 2, 2, 2, 2, 2, 2, 2, 2, 2, 2, 4 ),
 ( 0.01657113979051928407, 0.01708818281900468042, 0.01760522584749007330, 0.01863931190446085559, 0.01915635493294623806, 0.01967339796143162400, 0.02070748401840238895, 0.02174157007537315736, 0.02277565613234392577, 0.02380974218931469419, 0.02484382824628546260, 0.02536087127477082426, 0.02587791430325619285, 0.02691200036022687453, 0.02794608641719755968, 0.02898017247416824482, 0.02949721550265357872, 0.03001425853113890568, 0.03104834458810954573, 0.03156538761659487269, 0.03208243064508019965, 0.03311651670205084663 ),
 .UNSPECIFIED. ) ;
#9286 = ADVANCED_FACE ( 'NONE', ( #34538 ), #10155, .T. ) ;
#9287 = CARTESIAN_POINT ( 'NONE',  ( 212.5000000000000000, 1.224646799147353256E-15, -10.00000000000000000 ) ) ;
#9288 = DIRECTION ( 'NONE',  ( -1.000000000000000000, 0.000000000000000000, 0.000000000000000000 ) ) ;
#9289 = CARTESIAN_POINT ( 'NONE',  ( 0.7561992213566378629, 33.71011734938328175, 3.723857881850638041 ) ) ;
#9291 = CARTESIAN_POINT ( 'NONE',  ( 145.0000000000000568, -174.9263417920030577, -39.67942821175577706 ) ) ;
#9290 = CARTESIAN_POINT ( 'NONE',  ( 27.99209646187092559, 25.49206711720156093, 68.31122994652405112 ) ) ;
#9292 = EDGE_CURVE ( 'NONE', #26696, #10620, #16968, .T. ) ;
#9293 = CARTESIAN_POINT ( 'NONE',  ( 0.07098926918644703210, 12.21472555652512426, -29.24628546289449105 ) ) ;
#9294 = LINE ( 'NONE', #11142, #14835 ) ;
#9295 = ORIENTED_EDGE ( 'NONE', *, *, #20714, .T. ) ;
#9296 = CARTESIAN_POINT ( 'NONE',  ( 11.99999999999999645, -145.0000000000000000, -190.9999999999999432 ) ) ;
#9297 = DIRECTION ( 'NONE',  ( -0.000000000000000000, -0.000000000000000000, -1.000000000000000000 ) ) ;
#9298 = EDGE_CURVE ( 'NONE', #25980, #7524, #24542, .T. ) ;
#9299 = EDGE_CURVE ( 'NONE', #33401, #21805, #182, .T. ) ;
#9300 = VECTOR ( 'NONE', #922, 1000.000000000000000 ) ;
#9301 = ORIENTED_EDGE ( 'NONE', *, *, #4562, .F. ) ;
#9302 = ORIENTED_EDGE ( 'NONE', *, *, #11924, .F. ) ;
#9303 = AXIS2_PLACEMENT_3D ( 'NONE', #12863, #15355, #10178 ) ;
#9304 = VECTOR ( 'NONE', #34457, 1000.000000000000000 ) ;
#9305 = VECTOR ( 'NONE', #25609, 1000.000000000000000 ) ;
#9306 = ORIENTED_EDGE ( 'NONE', *, *, #34407, .T. ) ;
#9307 = CARTESIAN_POINT ( 'NONE',  ( 0.000000000000000000, 0.000000000000000000, 0.000000000000000000 ) ) ;
#9308 = EDGE_LOOP ( 'NONE', ( #33651, #23780 ) ) ;
#9309 = ORIENTED_EDGE ( 'NONE', *, *, #12190, .T. ) ;
#9310 = CARTESIAN_POINT ( 'NONE',  ( -29.72561944762171393, -13.25111019240559251, 68.31122994652405112 ) ) ;
#9311 = ITEM_DEFINED_TRANSFORMATION ( 'NONE', 'NONE', #4183,  #28566 ) ;
#9312 = ORIENTED_EDGE ( 'NONE', *, *, #14771, .F. ) ;
#9313 = DIRECTION ( 'NONE',  ( -0.000000000000000000, -1.836970198721029688E-16, 1.000000000000000000 ) ) ;
#9314 = CARTESIAN_POINT ( 'NONE',  ( -8.323328165997453710E-14, 29.09328061627312678, -9.684256520155496872 ) ) ;
#9315 = ORIENTED_EDGE ( 'NONE', *, *, #23237, .F. ) ;
#9316 = VERTEX_POINT ( 'NONE', #27754 ) ;
#9317 = DIRECTION ( 'NONE',  ( -0.9635499925192230197, 0.2675283385292207550, 0.000000000000000000 ) ) ;
#9318 = LINE ( 'NONE', #17699, #29534 ) ;
#9319 = DIRECTION ( 'NONE',  ( 1.000000000000000000, 0.000000000000000000, 0.000000000000000000 ) ) ;
#9320 = CARTESIAN_POINT ( 'NONE',  ( 2.789999999999999147, 28.95078156989557527, 9.502838467758159879 ) ) ;
#9321 = VERTEX_POINT ( 'NONE', #538 ) ;
#9322 = CARTESIAN_POINT ( 'NONE',  ( -145.0000000000000568, -174.9263417920030577, -39.67942821175577706 ) ) ;
#9323 = DIRECTION ( 'NONE',  ( -3.040835319149746528E-31, -1.000000000000000000, 0.000000000000000000 ) ) ;
#9324 = CIRCLE ( 'NONE', #34887, 7.999999999999979572 ) ;
#9325 = CARTESIAN_POINT ( 'NONE',  ( 2.789999999999999147, -27.53147453683415335, -13.05640081644869532 ) ) ;
#9326 = VERTEX_POINT ( 'NONE', #3194 ) ;
#9327 = CARTESIAN_POINT ( 'NONE',  ( 11.99999999999999645, 140.9999999999999716, -155.0000000000000000 ) ) ;
#9328 = DIRECTION ( 'NONE',  ( 1.000000000000000000, 0.000000000000000000, 0.000000000000000000 ) ) ;
#9329 = CARTESIAN_POINT ( 'NONE',  ( -12.00000000000001066, 144.9999999999999716, 187.0000000000000000 ) ) ;
#9330 = EDGE_CURVE ( 'NONE', #20393, #34350, #5502, .T. ) ;
#9331 = EDGE_CURVE ( 'NONE', #469, #5761, #6393, .T. ) ;
#9332 = DIRECTION ( 'NONE',  ( -1.000000000000000000, 0.000000000000000000, 0.000000000000000000 ) ) ;
#9334 = LINE ( 'NONE', #24985, #34981 ) ;
#9333 = CARTESIAN_POINT ( 'NONE',  ( -117.4999999999997442, 1.530808498934191521E-15, -12.50000000000000000 ) ) ;
#9335 = AXIS2_PLACEMENT_3D ( 'NONE', #1109, #30832, #17327 ) ;
#9336 = EDGE_CURVE ( 'NONE', #34071, #17516, #19068, .T. ) ;
#9337 = EDGE_CURVE ( 'NONE', #4220, #1172, #10103, .T. ) ;
#9338 = AXIS2_PLACEMENT_3D ( 'NONE', #3631, #25703, #28557 ) ;
#9339 = CARTESIAN_POINT ( 'NONE',  ( 11.99999999999999645, -145.0000000000000000, 194.9999999999999716 ) ) ;
#9340 = ORIENTED_EDGE ( 'NONE', *, *, #11464, .F. ) ;
#9341 = FACE_OUTER_BOUND ( 'NONE', #22628, .T. ) ;
#9343 = CARTESIAN_POINT ( 'NONE',  ( 2.789999999999999147, 11.30192140231272191, -28.29696565125058072 ) ) ;
#9342 = CARTESIAN_POINT ( 'NONE',  ( -9.978866888775632660, -1.691831803474588058, -87.50000000000000000 ) ) ;
#9344 = AXIS2_PLACEMENT_3D ( 'NONE', #770, #11637, #22487 ) ;
#9345 = ORIENTED_EDGE ( 'NONE', *, *, #11981, .T. ) ;
#9346 = CARTESIAN_POINT ( 'NONE',  ( -35.00000000000000000, 16.36947364650383818, -36.69637551990492597 ) ) ;
#9347 = VERTEX_POINT ( 'NONE', #32557 ) ;
#9348 = EDGE_CURVE ( 'NONE', #13256, #32232, #23194, .T. ) ;
#9349 = AXIS2_PLACEMENT_3D ( 'NONE', #32151, #15974, #21643 ) ;
#9350 = VERTEX_POINT ( 'NONE', #22073 ) ;
#9351 = FACE_OUTER_BOUND ( 'NONE', #24890, .T. ) ;
#9352 = ORIENTED_EDGE ( 'NONE', *, *, #14795, .F. ) ;
#9353 = B_SPLINE_CURVE_WITH_KNOTS ( 'NONE', 3,
 ( #9738, #31446, #28954, #29127 ),
 .UNSPECIFIED., .F., .F.,
 ( 4, 4 ),
 ( 0.005298612564832102384, 0.005985477723952492904 ),
 .UNSPECIFIED. ) ;
#9354 = ORIENTED_EDGE ( 'NONE', *, *, #35020, .F. ) ;
#9355 = CARTESIAN_POINT ( 'NONE',  ( -365.0000000000000000, 132.9999999999999716, 126.0000000000000000 ) ) ;
#9356 = AXIS2_PLACEMENT_3D ( 'NONE', #7107, #4081, #14977 ) ;
#9357 = ADVANCED_FACE ( 'NONE', ( #27403 ), #21889, .T. ) ;
#9358 = DIRECTION ( 'NONE',  ( 1.000000000000000000, 0.000000000000000000, -1.848892746611746966E-32 ) ) ;
#9359 = CARTESIAN_POINT ( 'NONE',  ( 1.749999999999999778, 22.14447232807506438, 26.34405054495565679 ) ) ;
#9360 = EDGE_CURVE ( 'NONE', #29353, #16028, #26584, .T. ) ;
#9361 = AXIS2_PLACEMENT_3D ( 'NONE', #34949, #21416, #18761 ) ;
#9363 = ADVANCED_FACE ( 'NONE', ( #5672 ), #8180, .F. ) ;
#9362 = CYLINDRICAL_SURFACE ( 'NONE', #14565, 16.19999999999999929 ) ;
#9364 = DIRECTION ( 'NONE',  ( 0.1081190184239419622, -0.9941379571543595972, 0.000000000000000000 ) ) ;
#9365 = ORIENTED_EDGE ( 'NONE', *, *, #1439, .F. ) ;
#9366 = ORIENTED_EDGE ( 'NONE', *, *, #34187, .F. ) ;
#9367 = AXIS2_PLACEMENT_3D ( 'NONE', #16804, #11274, #27629 ) ;
#9368 = DIRECTION ( 'NONE',  ( -1.000000000000000000, 0.000000000000000000, 0.000000000000000000 ) ) ;
#9369 = DIRECTION ( 'NONE',  ( 1.000000000000000000, 0.000000000000000000, -1.848892746611746966E-32 ) ) ;
#9370 = DIRECTION ( 'NONE',  ( -0.000000000000000000, -0.000000000000000000, 1.000000000000000000 ) ) ;
#9371 = AXIS2_PLACEMENT_3D ( 'NONE', #23997, #9046, #3170 ) ;
#9372 = ADVANCED_FACE ( 'NONE', ( #16573 ), #8535, .F. ) ;
#9373 = DIRECTION ( 'NONE',  ( 1.232595164407830946E-32, 0.000000000000000000, 1.000000000000000000 ) ) ;
#9374 = DIRECTION ( 'NONE',  ( 0.000000000000000000, 0.000000000000000000, -1.000000000000000000 ) ) ;
#9375 = CARTESIAN_POINT ( 'NONE',  ( 0.000000000000000000, 1.974842713994612024E-15, 76.74945698428001606 ) ) ;
#9376 = CARTESIAN_POINT ( 'NONE',  ( -14.49673343639653744, 34.98409864655521773, 68.31122994652405112 ) ) ;
#9377 = ORIENTED_EDGE ( 'NONE', *, *, #34026, .T. ) ;
#9378 = DIRECTION ( 'NONE',  ( 0.000000000000000000, 0.000000000000000000, 1.000000000000000000 ) ) ;
#9379 = CARTESIAN_POINT ( 'NONE',  ( -365.0000000000000000, -119.0000000000000000, 109.9999999999999858 ) ) ;
#9380 = FACE_BOUND ( 'NONE', #24612, .T. ) ;
#9381 = ORIENTED_EDGE ( 'NONE', *, *, #24609, .T. ) ;
#9382 = VECTOR ( 'NONE', #10222, 1000.000000000000000 ) ;
#9383 = EDGE_CURVE ( 'NONE', #11080, #13888, #23748, .T. ) ;
#9384 = EDGE_CURVE ( 'NONE', #15134, #32629, #7836, .T. ) ;
#9385 = DIRECTION ( 'NONE',  ( 1.000000000000000000, 0.000000000000000000, 0.000000000000000000 ) ) ;
#9386 = EDGE_LOOP ( 'NONE', ( #27120, #12237, #4504, #3154, #6143, #23618 ) ) ;
#9387 = LINE ( 'NONE', #25030, #287 ) ;
#9388 = CIRCLE ( 'NONE', #21321, 2.525000000000002576 ) ;
#9389 = LINE ( 'NONE', #20250, #15981 ) ;
#9390 = EDGE_CURVE ( 'NONE', #3106, #13445, #8452, .T. ) ;
#9391 = AXIS2_PLACEMENT_3D ( 'NONE', #8669, #19897, #25389 ) ;
#9392 = ORIENTED_EDGE ( 'NONE', *, *, #3056, .T. ) ;
#9393 = AXIS2_PLACEMENT_3D ( 'NONE', #28469, #34684, #12981 ) ;
#9394 = DIRECTION ( 'NONE',  ( 0.000000000000000000, 0.000000000000000000, 1.000000000000000000 ) ) ;
#9395 = CARTESIAN_POINT ( 'NONE',  ( -5.021133111224782120, 14.09580098603202458, -67.50000000000000000 ) ) ;
#9396 = DIRECTION ( 'NONE',  ( 0.000000000000000000, -2.309213040847544338E-50, -1.000000000000000000 ) ) ;
#9397 = AXIS2_PLACEMENT_3D ( 'NONE', #31731, #29061, #7339 ) ;
#9398 = EDGE_LOOP ( 'NONE', ( #3085, #21517, #19902, #28574 ) ) ;
#9399 = DIRECTION ( 'NONE',  ( -0.1063910735369225230, 0.9943243633099118073, -1.000770725407345128E-14 ) ) ;
#9400 = CARTESIAN_POINT ( 'NONE',  ( -449.9999999999999432, -105.0000000000000142, -77.99999999999997158 ) ) ;
#9401 = VERTEX_POINT ( 'NONE', #32386 ) ;
#9402 = CARTESIAN_POINT ( 'NONE',  ( 3.985664461616347742E-15, -32.54542015209057126, 76.74945698428001606 ) ) ;
#9403 = EDGE_CURVE ( 'NONE', #5171, #5918, #5850, .T. ) ;
#9404 = DIRECTION ( 'NONE',  ( 0.000000000000000000, 0.000000000000000000, 1.000000000000000000 ) ) ;
#9405 = EDGE_CURVE ( 'NONE', #23614, #29353, #21713, .T. ) ;
#9406 = CIRCLE ( 'NONE', #8806, 4.750000000000004441 ) ;
#9407 = DIRECTION ( 'NONE',  ( 0.000000000000000000, 2.309213040847544338E-50, 1.000000000000000000 ) ) ;
#9408 = DIRECTION ( 'NONE',  ( -1.000000000000000000, 0.000000000000000000, 0.000000000000000000 ) ) ;
#9409 = ORIENTED_EDGE ( 'NONE', *, *, #18470, .T. ) ;
#9410 = ORIENTED_EDGE ( 'NONE', *, *, #34407, .F. ) ;
#9411 = VERTEX_POINT ( 'NONE', #8711 ) ;
#9412 = AXIS2_PLACEMENT_3D ( 'NONE', #17582, #28419, #25738 ) ;
#9413 = VECTOR ( 'NONE', #27172, 1000.000000000000000 ) ;
#9414 = EDGE_CURVE ( 'NONE', #12936, #980, #21548, .T. ) ;
#9415 = DIRECTION ( 'NONE',  ( -0.000000000000000000, 1.000000000000000000, -0.000000000000000000 ) ) ;
#9416 = VERTEX_POINT ( 'NONE', #5388 ) ;
#9417 = LINE ( 'NONE', #12445, #25272 ) ;
#9418 = CARTESIAN_POINT ( 'NONE',  ( -500.0000000000000000, -113.0000000000000000, 155.0000000000000000 ) ) ;
#9419 = AXIS2_PLACEMENT_3D ( 'NONE', #2070, #15092, #34466 ) ;
#9420 = CARTESIAN_POINT ( 'NONE',  ( -430.0000000000000000, 118.9999999999999716, 109.9999999999999858 ) ) ;
#9421 = CARTESIAN_POINT ( 'NONE',  ( -45.05956070192387841, -32.65143121711728469, 20.00000000000000000 ) ) ;
#9422 = ORIENTED_EDGE ( 'NONE', *, *, #5872, .F. ) ;
#9423 = EDGE_CURVE ( 'NONE', #8068, #14037, #12963, .T. ) ;
#9424 = CIRCLE ( 'NONE', #32699, 1.999999999999999556 ) ;
#9425 = AXIS2_PLACEMENT_3D ( 'NONE', #12325, #31182, #4100 ) ;
#9426 = CARTESIAN_POINT ( 'NONE',  ( 104.0527614346196970, 5.662516510817761528, 11.14395138485681791 ) ) ;
#9427 = VERTEX_POINT ( 'NONE', #3888 ) ;
#9428 = FACE_OUTER_BOUND ( 'NONE', #20626, .T. ) ;
#9429 = CARTESIAN_POINT ( 'NONE',  ( -12.00000000000001066, 144.9999999999999716, -194.9999999999999432 ) ) ;
#9430 = ORIENTED_EDGE ( 'NONE', *, *, #20060, .F. ) ;
#9431 = LINE ( 'NONE', #31139, #4397 ) ;
#9432 =( LENGTH_UNIT ( ) NAMED_UNIT ( * ) SI_UNIT ( .MILLI., .METRE. ) );
#9433 = CARTESIAN_POINT ( 'NONE',  ( 2.765921099433441110, 14.63235270440936731, 27.43224275967444470 ) ) ;
#9434 = AXIS2_PLACEMENT_3D ( 'NONE', #10634, #15983, #18825 ) ;
#9435 = CARTESIAN_POINT ( 'NONE',  ( -110.1150203881707910, 3.166944581793445397E-20, 12.50000000000000000 ) ) ;
#9436 = DIRECTION ( 'NONE',  ( -1.232595164407830946E-32, -3.421138828918010427E-49, 1.000000000000000000 ) ) ;
#9437 = EDGE_CURVE ( 'NONE', #15497, #5208, #9431, .T. ) ;
#9438 = DIRECTION ( 'NONE',  ( 0.000000000000000000, 1.000000000000000000, 1.224646799147353207E-16 ) ) ;
#9439 = AXIS2_PLACEMENT_3D ( 'NONE', #21228, #13405, #32255 ) ;
#9440 = VERTEX_POINT ( 'NONE', #17464 ) ;
#9441 = EDGE_LOOP ( 'NONE', ( #11859, #34213, #13046, #18356 ) ) ;
#9442 = DIRECTION ( 'NONE',  ( -0.9037832198196827926, 0.4279905274329873222, -3.068311030645359541E-14 ) ) ;
#9443 =( REPRESENTATION_RELATIONSHIP ('NONE','NONE', #23037, #15767 ) REPRESENTATION_RELATIONSHIP_WITH_TRANSFORMATION ( #26505 )SHAPE_REPRESENTATION_RELATIONSHIP( ) );
#9444 = VERTEX_POINT ( 'NONE', #3722 ) ;
#9445 = VECTOR ( 'NONE', #9899, 1000.000000000000000 ) ;
#9446 = ADVANCED_FACE ( 'NONE', ( #9070 ), #11757, .T. ) ;
#9447 = EDGE_CURVE ( 'NONE', #7199, #33055, #30961, .T. ) ;
#9448 = FACE_OUTER_BOUND ( 'NONE', #19792, .T. ) ;
#9449 = CIRCLE ( 'NONE', #7157, 7.999999999999979572 ) ;
#9450 = EDGE_CURVE ( 'NONE', #1617, #24520, #15292, .T. ) ;
#9451 = LINE ( 'NONE', #6401, #3971 ) ;
#9452 = VERTEX_POINT ( 'NONE', #25607 ) ;
#9453 = DIRECTION ( 'NONE',  ( 0.000000000000000000, -7.888609052210118054E-31, -1.000000000000000000 ) ) ;
#9454 = CARTESIAN_POINT ( 'NONE',  ( -101.1502780286438679, -3.384384043357604011, -12.03563115889556379 ) ) ;
#9455 = VECTOR ( 'NONE', #2559, 1000.000000000000000 ) ;
#9457 = DIRECTION ( 'NONE',  ( 0.000000000000000000, 1.000000000000000000, 0.000000000000000000 ) ) ;
#9456 = CARTESIAN_POINT ( 'NONE',  ( -499.9999999999999432, 108.9999999999999858, -187.0000000000000000 ) ) ;
#9458 = VERTEX_POINT ( 'NONE', #6566 ) ;
#9459 = ORIENTED_EDGE ( 'NONE', *, *, #426, .T. ) ;
#9460 = DIRECTION ( 'NONE',  ( 0.000000000000000000, 0.6845471059286788451, 0.7289686274214207673 ) ) ;
#9461 = DIRECTION ( 'NONE',  ( 0.000000000000000000, 0.000000000000000000, -1.000000000000000000 ) ) ;
#9462 = DIRECTION ( 'NONE',  ( -1.000000000000000000, 0.000000000000000000, -0.000000000000000000 ) ) ;
#9463 = VERTEX_POINT ( 'NONE', #33273 ) ;
#9464 = DIRECTION ( 'NONE',  ( -0.000000000000000000, -0.000000000000000000, -1.000000000000000000 ) ) ;
#9465 = DIRECTION ( 'NONE',  ( 0.000000000000000000, 0.000000000000000000, 1.000000000000000000 ) ) ;
#9466 = VERTEX_POINT ( 'NONE', #11933 ) ;
#9467 = CIRCLE ( 'NONE', #2642, 2.525000000000001243 ) ;
#9468 = CARTESIAN_POINT ( 'NONE',  ( -499.9999999999999432, 136.9999999999999432, -162.9999999999999716 ) ) ;
#9469 = CARTESIAN_POINT ( 'NONE',  ( 0.000000000000000000, -14.75935258146395412, -26.65732927035534416 ) ) ;
#9470 = CARTESIAN_POINT ( 'NONE',  ( 0.02407890056655564992, 31.00221527374952046, 2.344426712874309260 ) ) ;
#9472 = DIRECTION ( 'NONE',  ( 1.000000000000000000, 0.000000000000000000, 0.000000000000000000 ) ) ;
#9471 = DIRECTION ( 'NONE',  ( 0.000000000000000000, 0.000000000000000000, -1.000000000000000000 ) ) ;
#9473 = DIRECTION ( 'NONE',  ( 0.000000000000000000, 1.000000000000000000, -2.309213040847544338E-50 ) ) ;
#9474 = CARTESIAN_POINT ( 'NONE',  ( 2.589916064955228858, 29.62776403357759492, 13.00174666746595342 ) ) ;
#9475 = ORIENTED_EDGE ( 'NONE', *, *, #21255, .F. ) ;
#9476 = CARTESIAN_POINT ( 'NONE',  ( 0.000000000000000000, 3.214697847761802057E-14, -87.50000000000000000 ) ) ;
#9477 = CARTESIAN_POINT ( 'NONE',  ( 0.1859802913914470612, -27.68787216339148571, -16.59794162419619568 ) ) ;
#9478 = PRODUCT_DEFINITION_SHAPE ( 'NONE', 'NONE',  #35176 ) ;
#9479 = VECTOR ( 'NONE', #7323, 1000.000000000000114 ) ;
#9480 = ORIENTED_EDGE ( 'NONE', *, *, #14642, .T. ) ;
#9481 = ADVANCED_FACE ( 'NONE', ( #12285 ), #12108, .F. ) ;
#9482 = VERTEX_POINT ( 'NONE', #28462 ) ;
#9483 = EDGE_CURVE ( 'NONE', #34419, #30924, #6386, .T. ) ;
#9484 = EDGE_CURVE ( 'NONE', #15525, #19346, #14950, .T. ) ;
#9485 = DIRECTION ( 'NONE',  ( 0.000000000000000000, 2.309213040847544338E-50, 1.000000000000000000 ) ) ;
#9486 = ORIENTED_EDGE ( 'NONE', *, *, #23530, .T. ) ;
#9487 = ORIENTED_EDGE ( 'NONE', *, *, #33279, .F. ) ;
#9488 = EDGE_LOOP ( 'NONE', ( #29837, #9906, #21153, #12648, #15072, #5387 ) ) ;
#9489 = EDGE_CURVE ( 'NONE', #15441, #33917, #3542, .T. ) ;
#9490 = DIRECTION ( 'NONE',  ( 0.000000000000000000, 0.000000000000000000, 1.000000000000000000 ) ) ;
#9491 = VECTOR ( 'NONE', #10034, 1000.000000000000000 ) ;
#9492 = ORIENTED_EDGE ( 'NONE', *, *, #13001, .F. ) ;
#9493 = DIRECTION ( 'NONE',  ( 0.000000000000000000, -1.000000000000000000, 0.000000000000000000 ) ) ;
#9494 = FACE_OUTER_BOUND ( 'NONE', #11208, .T. ) ;
#9495 = ORIENTED_EDGE ( 'NONE', *, *, #17447, .T. ) ;
#9496 = VERTEX_POINT ( 'NONE', #30611 ) ;
#9497 = CARTESIAN_POINT ( 'NONE',  ( -19.99999999999998934, 112.9999999999999574, 155.0000000000000000 ) ) ;
#9498 = DIRECTION ( 'NONE',  ( -1.000000000000000000, 0.000000000000000000, 0.000000000000000000 ) ) ;
#9499 = AXIS2_PLACEMENT_3D ( 'NONE', #6027, #19583, #33088 ) ;
#9500 = EDGE_CURVE ( 'NONE', #30129, #32360, #6203, .T. ) ;
#9501 = DIRECTION ( 'NONE',  ( 1.000000000000000000, 0.000000000000000000, 0.000000000000000000 ) ) ;
#9502 = CARTESIAN_POINT ( 'NONE',  ( -30.58418286738120884, -22.31615353445080174, 68.31122994652405112 ) ) ;
#9503 = DIRECTION ( 'NONE',  ( 0.000000000000000000, 0.000000000000000000, 1.000000000000000000 ) ) ;
#9504 = ORIENTED_EDGE ( 'NONE', *, *, #9000, .T. ) ;
#9505 = CARTESIAN_POINT ( 'NONE',  ( 44.94043929807611448, -20.15143121711728469, 0.000000000000000000 ) ) ;
#9507 = CARTESIAN_POINT ( 'NONE',  ( -35.00000000000000000, 8.360858262960551457, 68.31122994652405112 ) ) ;
#9506 = CIRCLE ( 'NONE', #15844, 8.000000000000000000 ) ;
#9508 = DIRECTION ( 'NONE',  ( -0.000000000000000000, -0.000000000000000000, -1.000000000000000000 ) ) ;
#9509 = EDGE_LOOP ( 'NONE', ( #3264, #2042, #19117, #17931 ) ) ;
#9510 = DIRECTION ( 'NONE',  ( 1.000000000000000000, 0.000000000000000000, 0.000000000000000000 ) ) ;
#9511 = CARTESIAN_POINT ( 'NONE',  ( 0.02407890056655695096, -26.45933846664182099, -16.32596387352474565 ) ) ;
#9512 = CARTESIAN_POINT ( 'NONE',  ( 30.98406361983693103, 9.959526819984921175, 68.31122994652405112 ) ) ;
#9513 = CARTESIAN_POINT ( 'NONE',  ( -9.978866888775733912, -11.61907005722761532, -67.50000000000000000 ) ) ;
#9515 = CARTESIAN_POINT ( 'NONE',  ( -7.654999999999999361, 0.000000000000000000, 3.931000000000000494 ) ) ;
#9514 = DIRECTION ( 'NONE',  ( 0.000000000000000000, 0.000000000000000000, 1.000000000000000000 ) ) ;
#9516 = DIRECTION ( 'NONE',  ( -1.000000000000000000, -0.000000000000000000, -0.000000000000000000 ) ) ;
#9517 = EDGE_LOOP ( 'NONE', ( #468, #8345, #25002, #17879 ) ) ;
#9518 = DIRECTION ( 'NONE',  ( 0.000000000000000000, -1.000000000000000000, 0.000000000000000000 ) ) ;
#9520 = CARTESIAN_POINT ( 'NONE',  ( 0.7564103440434756243, -2.658578268447333581, 33.81118535743536313 ) ) ;
#9519 = DIRECTION ( 'NONE',  ( 0.000000000000000000, 1.000000000000000000, 0.000000000000000000 ) ) ;
#9521 = VECTOR ( 'NONE', #9369, 1000.000000000000000 ) ;
#9522 = EDGE_LOOP ( 'NONE', ( #15414, #11002, #5444, #34777 ) ) ;
#9523 = PRODUCT_DEFINITION_SHAPE ( 'NONE', 'NONE',  #35108 ) ;
#9524 = LINE ( 'NONE', #17721, #19432 ) ;
#9525 = EDGE_LOOP ( 'NONE', ( #4787, #8724, #10418, #34158 ) ) ;
#9526 = EDGE_CURVE ( 'NONE', #25899, #20834, #11574, .T. ) ;
#9527 = VECTOR ( 'NONE', #10463, 1000.000000000000000 ) ;
#9528 = AXIS2_PLACEMENT_3D ( 'NONE', #2876, #19806, #32601 ) ;
#9529 = ORIENTED_EDGE ( 'NONE', *, *, #22258, .T. ) ;
#9530 = CARTESIAN_POINT ( 'NONE',  ( 102.0964664041139542, -4.962105133902832144, -5.629733210525461828 ) ) ;
#9531 = EDGE_LOOP ( 'NONE', ( #21872, #11708, #13263, #20041 ) ) ;
#9532 = EDGE_LOOP ( 'NONE', ( #31156, #9392, #27208, #1319 ) ) ;
#9533 = EDGE_CURVE ( 'NONE', #31862, #9166, #17099, .T. ) ;
#9534 = CARTESIAN_POINT ( 'NONE',  ( 0.7564103432032210916, -18.61839266759128009, 28.34818773854056673 ) ) ;
#9535 = EDGE_CURVE ( 'NONE', #33194, #31447, #1067, .T. ) ;
#9537 = DIRECTION ( 'NONE',  ( 1.000000000000000000, 0.000000000000000000, -0.000000000000000000 ) ) ;
#9536 =( GEOMETRIC_REPRESENTATION_CONTEXT ( 3 ) GLOBAL_UNCERTAINTY_ASSIGNED_CONTEXT ( ( #12745 ) ) GLOBAL_UNIT_ASSIGNED_CONTEXT ( ( #33072, #9051, #30761 ) ) REPRESENTATION_CONTEXT ( 'NONE', 'WORKASPACE' ) );
#9538 = DIRECTION ( 'NONE',  ( 0.000000000000000000, 0.000000000000000000, 1.000000000000000000 ) ) ;
#9539 = CARTESIAN_POINT ( 'NONE',  ( -418.0000000000000000, 105.0000000000000000, -73.99999999999998579 ) ) ;
#9540 = ADVANCED_FACE ( 'NONE', ( #33624 ), #20113, .F. ) ;
#9541 = ORIENTED_EDGE ( 'NONE', *, *, #19499, .T. ) ;
#9542 = EDGE_CURVE ( 'NONE', #14486, #18246, #33023, .T. ) ;
#9543 = ORIENTED_EDGE ( 'NONE', *, *, #34846, .T. ) ;
#9544 = DIRECTION ( 'NONE',  ( 0.000000000000000000, -0.9980267284282717810, 0.06279051952931077873 ) ) ;
#9545 = DIRECTION ( 'NONE',  ( 0.000000000000000000, -6.123233995736766036E-17, -1.000000000000000000 ) ) ;
#9546 = CARTESIAN_POINT ( 'NONE',  ( -365.0000000000000000, 134.9999999999999716, 126.0000000000000000 ) ) ;
#9547 = DIRECTION ( 'NONE',  ( 0.000000000000000000, 1.836970198721029934E-16, -1.000000000000000000 ) ) ;
#9548 = DIRECTION ( 'NONE',  ( -0.000000000000000000, -0.000000000000000000, 1.000000000000000000 ) ) ;
#9549 = CARTESIAN_POINT ( 'NONE',  ( -418.0000000000000000, 137.0000000000000000, -175.0000000000000000 ) ) ;
#9550 = CIRCLE ( 'NONE', #26982, 4.000000000000003553 ) ;
#9551 = CARTESIAN_POINT ( 'NONE',  ( 0.000000000000000000, -11.69134295108990607, 6.750000000000024869 ) ) ;
#9552 = ORIENTED_EDGE ( 'NONE', *, *, #19216, .F. ) ;
#9553 = DIRECTION ( 'NONE',  ( 0.000000000000000000, 1.836970198721029688E-16, -1.000000000000000000 ) ) ;
#9554 = DIRECTION ( 'NONE',  ( -0.3203292411224473168, 0.8039657716618124894, -0.5010271602200255803 ) ) ;
#9555 = EDGE_CURVE ( 'NONE', #3078, #3836, #828, .T. ) ;
#9556 = DIRECTION ( 'NONE',  ( 0.8568571761675904952, -0.5155538571770196254, -0.000000000000000000 ) ) ;
#9557 = ORIENTED_EDGE ( 'NONE', *, *, #17768, .F. ) ;
#9558 = AXIS2_PLACEMENT_3D ( 'NONE', #23993, #32196, #23833 ) ;
#9559 = AXIS2_PLACEMENT_3D ( 'NONE', #26876, #24202, #26166 ) ;
#9560 = CARTESIAN_POINT ( 'NONE',  ( -349.0000000000000000, -125.0000000000000284, 183.0000000000000000 ) ) ;
#9561 = ORIENTED_EDGE ( 'NONE', *, *, #12159, .T. ) ;
#9562 = CARTESIAN_POINT ( 'NONE',  ( 11.99999999999999645, -124.9999999999999432, -154.9999999999999716 ) ) ;
#9563 = DIRECTION ( 'NONE',  ( -0.000000000000000000, 0.000000000000000000, -1.000000000000000000 ) ) ;
#9564 = VECTOR ( 'NONE', #8604, 1000.000000000000000 ) ;
#9565 = EDGE_CURVE ( 'NONE', #32705, #30129, #19527, .T. ) ;
#9566 = EDGE_CURVE ( 'NONE', #4598, #16921, #30587, .T. ) ;
#9567 = ORIENTED_EDGE ( 'NONE', *, *, #7865, .T. ) ;
#9568 = CARTESIAN_POINT ( 'NONE',  ( 11.99999999999999645, 134.9999999999999432, -186.9999999999999716 ) ) ;
#9569 = DIRECTION ( 'NONE',  ( -0.000000000000000000, -1.000000000000000000, -0.000000000000000000 ) ) ;
#9570 = ORIENTED_EDGE ( 'NONE', *, *, #29949, .T. ) ;
#9571 = VECTOR ( 'NONE', #21778, 1000.000000000000000 ) ;
#9572 = CARTESIAN_POINT ( 'NONE',  ( 780.2051380588591201, 1120.010299497888809, 1753.598338701303646 ) ) ;
#9573 = DIRECTION ( 'NONE',  ( 0.000000000000000000, 0.000000000000000000, 1.000000000000000000 ) ) ;
#9574 = ORIENTED_EDGE ( 'NONE', *, *, #893, .F. ) ;
#9575 = CARTESIAN_POINT ( 'NONE',  ( 1.040000000000000258, 22.14447232807544452, -26.34405054495532639 ) ) ;
#9576 = LINE ( 'NONE', #15275, #4443 ) ;
#9577 = VECTOR ( 'NONE', #26502, 1000.000000000000000 ) ;
#9578 = FACE_OUTER_BOUND ( 'NONE', #15485, .T. ) ;
#9579 = CARTESIAN_POINT ( 'NONE',  ( -10.00000000000000000, 0.000000000000000000, 0.000000000000000000 ) ) ;
#9580 = CONTEXT_DEPENDENT_SHAPE_REPRESENTATION ( #33068, #27922 ) ;
#9581 = EDGE_CURVE ( 'NONE', #25253, #16922, #14188, .T. ) ;
#9582 = ORIENTED_EDGE ( 'NONE', *, *, #1751, .T. ) ;
#9583 = EDGE_CURVE ( 'NONE', #10395, #7236, #10674, .T. ) ;
#9584 = EDGE_LOOP ( 'NONE', ( #813, #33558 ) ) ;
#9585 = AXIS2_PLACEMENT_3D ( 'NONE', #10844, #2822, #24186 ) ;
#9586 = VERTEX_POINT ( 'NONE', #16336 ) ;
#9587 = CARTESIAN_POINT ( 'NONE',  ( 0.02407890056655738464, 26.03801215795517621, 16.98986790278620873 ) ) ;
#9588 = CARTESIAN_POINT ( 'NONE',  ( -355.0000000000000000, -131.0000000000000000, 128.0000000000000000 ) ) ;
#9589 = CONICAL_SURFACE ( 'NONE', #15263, 6.898500000000000298, 0.7853981633974428389 ) ;
#9590 = CARTESIAN_POINT ( 'NONE',  ( -12.00000000000001066, -56.99999999999997868, 154.9999999999999716 ) ) ;
#9591 = DIRECTION ( 'NONE',  ( -1.000000000000000000, 6.792721752314501023E-48, -3.697785493223492838E-32 ) ) ;
#9592 = CARTESIAN_POINT ( 'NONE',  ( -5.021133111225196011, -21.54630831098063837, -67.50000000000000000 ) ) ;
#9593 = CARTESIAN_POINT ( 'NONE',  ( 2.789999999999999147, -25.77598557799237255, -16.24962337825830616 ) ) ;
#9594 = ORIENTED_EDGE ( 'NONE', *, *, #29299, .T. ) ;
#9595 = CARTESIAN_POINT ( 'NONE',  ( 106.3182022809973546, 5.587831648195837886, 11.18158713856774966 ) ) ;
#9596 = CIRCLE ( 'NONE', #12452, 2.033421858999710619 ) ;
#9597 = ORIENTED_EDGE ( 'NONE', *, *, #11078, .T. ) ;
#9598 = CARTESIAN_POINT ( 'NONE',  ( -19.99999999999996092, -141.0000000000000000, 162.9999999999999716 ) ) ;
#9599 = AXIS2_PLACEMENT_3D ( 'NONE', #11957, #20138, #25630 ) ;
#9600 = DIRECTION ( 'NONE',  ( 0.000000000000000000, 1.000000000000000000, 5.053935297177146739E-49 ) ) ;
#9601 = ORIENTED_EDGE ( 'NONE', *, *, #130, .F. ) ;
#9602 = DIRECTION ( 'NONE',  ( 0.000000000000000000, -3.374343856708137958E-53, 1.000000000000000000 ) ) ;
#9603 = EDGE_CURVE ( 'NONE', #31232, #27516, #16376, .T. ) ;
#9604 = CARTESIAN_POINT ( 'NONE',  ( 0.02407890056655911937, -15.32140196853734970, -27.05343472113007763 ) ) ;
#9605 = EDGE_CURVE ( 'NONE', #13218, #19961, #11165, .T. ) ;
#9606 = ADVANCED_FACE ( 'NONE', ( #649 ), #16869, .F. ) ;
#9607 = CYLINDRICAL_SURFACE ( 'NONE', #9181, 2.033421858999711951 ) ;
#9608 = UNCERTAINTY_MEASURE_WITH_UNIT (LENGTH_MEASURE( 1.000000000000000082E-05 ), #24956, 'distance_accuracy_value', 'NONE');
#9609 = CARTESIAN_POINT ( 'NONE',  ( 0.006871061880576827090, -0.3206953221633991324, -30.86785892350566129 ) ) ;
#9610 = CARTESIAN_POINT ( 'NONE',  ( -45.05956070192387841, -20.15143121711730245, 0.000000000000000000 ) ) ;
#9611 = EDGE_CURVE ( 'NONE', #25692, #10763, #19704, .T. ) ;
#9612 = ORIENTED_EDGE ( 'NONE', *, *, #30090, .T. ) ;
#9613 = ORIENTED_EDGE ( 'NONE', *, *, #5479, .F. ) ;
#9614 = CARTESIAN_POINT ( 'NONE',  ( 793.3444284848958432, 997.2113075065323073, 1753.598338701303419 ) ) ;
#9615 = ORIENTED_EDGE ( 'NONE', *, *, #20466, .T. ) ;
#9616 = DIRECTION ( 'NONE',  ( 0.000000000000000000, 0.000000000000000000, 1.000000000000000000 ) ) ;
#9617 = AXIS2_PLACEMENT_3D ( 'NONE', #29542, #22549, #32204 ) ;
#9618 = CARTESIAN_POINT ( 'NONE',  ( -418.0000000000000568, -105.0000000000000142, 159.0000000000000000 ) ) ;
#9619 = ORIENTED_EDGE ( 'NONE', *, *, #2951, .F. ) ;
#9620 = CARTESIAN_POINT ( 'NONE',  ( -20.00000000000001776, -124.9999999999999432, -162.9999999999999432 ) ) ;
#9621 = CARTESIAN_POINT ( 'NONE',  ( 14.70109753509668948, 34.88954974633767137, -36.68877005347593467 ) ) ;
#9622 = VECTOR ( 'NONE', #32319, 1000.000000000000000 ) ;
#9624 = FACE_OUTER_BOUND ( 'NONE', #33796, .T. ) ;
#9623 = DIRECTION ( 'NONE',  ( 0.000000000000000000, 1.000000000000000000, 5.053935297177146739E-49 ) ) ;
#9625 = ORIENTED_EDGE ( 'NONE', *, *, #12360, .T. ) ;
#9626 = ORIENTED_EDGE ( 'NONE', *, *, #18110, .T. ) ;
#9627 = DIRECTION ( 'NONE',  ( -1.000000000000000000, -0.000000000000000000, 0.000000000000000000 ) ) ;
#9628 = CARTESIAN_POINT ( 'NONE',  ( 2.789999999999999147, -15.78270255339054451, -26.02842157509105547 ) ) ;
#9629 = DIRECTION ( 'NONE',  ( 0.000000000000000000, 0.000000000000000000, 1.000000000000000000 ) ) ;
#9630 = ORIENTED_EDGE ( 'NONE', *, *, #33754, .F. ) ;
#9631 = AXIS2_PLACEMENT_3D ( 'NONE', #4880, #32461, #29808 ) ;
#9632 = DIRECTION ( 'NONE',  ( -1.000000000000000000, 6.792721752314501023E-48, -3.697785493223492838E-32 ) ) ;
#9633 = ORIENTED_EDGE ( 'NONE', *, *, #34600, .F. ) ;
#9634 = CARTESIAN_POINT ( 'NONE',  ( -414.0000000000000000, -105.0000000000000142, 132.0000000000000000 ) ) ;
#9635 = CARTESIAN_POINT ( 'NONE',  ( 1.040000000000003810, -2.430610048905784915, -34.32897884578301984 ) ) ;
#9636 = FACE_OUTER_BOUND ( 'NONE', #8476, .T. ) ;
#9637 = EDGE_CURVE ( 'NONE', #32232, #2295, #7627, .T. ) ;
#9639 = CARTESIAN_POINT ( 'NONE',  ( 50.00050000000000239, 12.80000000000000071, -3.000000000000000000 ) ) ;
#9638 = CARTESIAN_POINT ( 'NONE',  ( 2.033800774102392683, 33.57713782924216872, 4.776499238012976711 ) ) ;
#9640 = ADVANCED_FACE ( 'NONE', ( #3134 ), #6145, .F. ) ;
#9641 = VECTOR ( 'NONE', #12520, 1000.000000000000227 ) ;
#9642 = APPLICATION_CONTEXT ( 'automotive_design' ) ;
#9643 = LINE ( 'NONE', #4452, #11603 ) ;
#9644 = CARTESIAN_POINT ( 'NONE',  ( 3.235562306570555532E-30, 14.09580098603202636, -87.50000000000000000 ) ) ;
#9645 = DIRECTION ( 'NONE',  ( 0.000000000000000000, -1.224646799147353207E-16, 1.000000000000000000 ) ) ;
#9646 = FACE_OUTER_BOUND ( 'NONE', #21186, .T. ) ;
#9647 = ORIENTED_EDGE ( 'NONE', *, *, #10587, .T. ) ;
#9648 = ORIENTED_EDGE ( 'NONE', *, *, #29791, .F. ) ;
#9649 = VERTEX_POINT ( 'NONE', #24663 ) ;
#9650 = AXIS2_PLACEMENT_3D ( 'NONE', #20709, #33704, #7159 ) ;
#9651 = DIRECTION ( 'NONE',  ( 0.000000000000000000, 0.000000000000000000, -1.000000000000000000 ) ) ;
#9652 = ORIENTED_EDGE ( 'NONE', *, *, #31968, .T. ) ;
#9653 = ORIENTED_EDGE ( 'NONE', *, *, #18373, .F. ) ;
#9654 = ORIENTED_EDGE ( 'NONE', *, *, #18230, .T. ) ;
#9655 = FACE_OUTER_BOUND ( 'NONE', #34843, .T. ) ;
#9656 = ORIENTED_EDGE ( 'NONE', *, *, #11143, .T. ) ;
#9657 = DIRECTION ( 'NONE',  ( 0.000000000000000000, -1.000000000000000000, 6.123233995736766036E-17 ) ) ;
#9658 = CARTESIAN_POINT ( 'NONE',  ( 0.000000000000000000, -115.0000000000000000, 0.000000000000000000 ) ) ;
#9659 = ORIENTED_EDGE ( 'NONE', *, *, #34677, .F. ) ;
#9660 = ORIENTED_EDGE ( 'NONE', *, *, #26542, .F. ) ;
#9661 = PLANE ( 'NONE',  #32181 ) ;
#9662 = DIRECTION ( 'NONE',  ( 0.000000000000000000, -2.309213040847544338E-50, -1.000000000000000000 ) ) ;
#9663 = DIRECTION ( 'NONE',  ( 0.000000000000000000, 1.000000000000000000, 0.000000000000000000 ) ) ;
#9664 = LINE ( 'NONE', #7151, #15977 ) ;
#9665 = LINE ( 'NONE', #31377, #4037 ) ;
#9666 = ORIENTED_EDGE ( 'NONE', *, *, #34712, .F. ) ;
#9667 = DIRECTION ( 'NONE',  ( 0.000000000000000000, 0.000000000000000000, -1.000000000000000000 ) ) ;
#9668 = DIRECTION ( 'NONE',  ( -2.530127506375325574E-80, 1.000000000000000000, 6.842277657836020854E-49 ) ) ;
#9669 = FACE_OUTER_BOUND ( 'NONE', #11735, .T. ) ;
#9670 = ORIENTED_EDGE ( 'NONE', *, *, #12341, .T. ) ;
#9671 = CARTESIAN_POINT ( 'NONE',  ( 0.02849990174189795042, 12.35429686688392259, 5.601730134768050817 ) ) ;
#9672 = CARTESIAN_POINT ( 'NONE',  ( -9.144464960067640646, -31.23432620483745836, 68.31122994652405112 ) ) ;
#9673 = EDGE_CURVE ( 'NONE', #26771, #33889, #20930, .T. ) ;
#9674 = CARTESIAN_POINT ( 'NONE',  ( 22.10765473302597073, -12.47301499840864025, -77.50000000000000000 ) ) ;
#9675 = AXIS2_PLACEMENT_3D ( 'NONE', #20472, #6758, #14448 ) ;
#9676 = DIRECTION ( 'NONE',  ( 0.000000000000000000, 0.000000000000000000, -1.000000000000000000 ) ) ;
#9678 = CARTESIAN_POINT ( 'NONE',  ( -12.00000000000001066, 134.9999999999998863, 162.9999999999999716 ) ) ;
#9677 = CARTESIAN_POINT ( 'NONE',  ( 1.394999999999999574, 21.72796464722008380, 26.68861566460903489 ) ) ;
#9679 = ADVANCED_FACE ( 'NONE', ( #13827 ), #2782, .T. ) ;
#9680 = CARTESIAN_POINT ( 'NONE',  ( 2.765921099433441999, -0.3931553186915530129, 31.08824725498900321 ) ) ;
#9681 = ORIENTED_EDGE ( 'NONE', *, *, #18034, .T. ) ;
#9682 = PRODUCT_RELATED_PRODUCT_CATEGORY ( 'part', '', ( #8627 ) ) ;
#9683 = DIRECTION ( 'NONE',  ( -1.000000000000000000, -0.000000000000000000, -0.000000000000000000 ) ) ;
#9685 = CARTESIAN_POINT ( 'NONE',  ( 28.11866956577617316, 16.38733641342590985, 68.31122994652405112 ) ) ;
#9684 = CYLINDRICAL_SURFACE ( 'NONE', #20618, 4.750000000000004441 ) ;
#9686 = EDGE_LOOP ( 'NONE', ( #32033, #1867, #946, #380, #23424, #8656, #11856, #13878, #6554, #7884, #7646, #21099 ) ) ;
#9687 =( REPRESENTATION_RELATIONSHIP ('NONE','NONE', #23037, #28231 ) REPRESENTATION_RELATIONSHIP_WITH_TRANSFORMATION ( #26191 )SHAPE_REPRESENTATION_RELATIONSHIP( ) );
#9688 = LINE ( 'NONE', #20550, #14305 ) ;
#9689 = ORIENTED_EDGE ( 'NONE', *, *, #21684, .F. ) ;
#9690 = ORIENTED_EDGE ( 'NONE', *, *, #27157, .T. ) ;
#9691 = CARTESIAN_POINT ( 'NONE',  ( -414.0000000000000568, -137.0000000000000000, 154.9999999999999716 ) ) ;
#9692 = ORIENTED_EDGE ( 'NONE', *, *, #27854, .F. ) ;
#9693 = ORIENTED_EDGE ( 'NONE', *, *, #234, .F. ) ;
#9694 = AXIS2_PLACEMENT_3D ( 'NONE', #22728, #9548, #22897 ) ;
#9695 = DIRECTION ( 'NONE',  ( -1.000000000000000000, -0.000000000000000000, -0.000000000000000000 ) ) ;
#9696 = VECTOR ( 'NONE', #7062, 1000.000000000000000 ) ;
#9697 = DIRECTION ( 'NONE',  ( -1.000000000000000000, 0.000000000000000000, 0.000000000000000000 ) ) ;
#9698 = DIRECTION ( 'NONE',  ( 0.000000000000000000, 5.145227585319922065E-49, 1.000000000000000000 ) ) ;
#9699 = ORIENTED_EDGE ( 'NONE', *, *, #18980, .F. ) ;
#9700 = ORIENTED_EDGE ( 'NONE', *, *, #22833, .F. ) ;
#9701 = DIRECTION ( 'NONE',  ( 0.9635499925192229087, -0.2675283385292207550, 0.000000000000000000 ) ) ;
#9702 = CARTESIAN_POINT ( 'NONE',  ( 145.0000000000000568, -85.49999999999998579, 51.88904920397798293 ) ) ;
#9703 = DIRECTION ( 'NONE',  ( 0.000000000000000000, 0.000000000000000000, 1.000000000000000000 ) ) ;
#9704 = LINE ( 'NONE', #22727, #18725 ) ;
#9705 = DIRECTION ( 'NONE',  ( 0.000000000000000000, -2.309213040847544338E-50, -1.000000000000000000 ) ) ;
#9706 = ORIENTED_EDGE ( 'NONE', *, *, #29976, .F. ) ;
#9707 = DIRECTION ( 'NONE',  ( -1.000000000000000000, 0.000000000000000000, 0.000000000000000000 ) ) ;
#9708 = FACE_OUTER_BOUND ( 'NONE', #34410, .T. ) ;
#9709 = ORIENTED_EDGE ( 'NONE', *, *, #10622, .F. ) ;
#9710 = AXIS2_PLACEMENT_3D ( 'NONE', #20937, #1715, #34460 ) ;
#9711 = CIRCLE ( 'NONE', #30190, 13.50000000000000178 ) ;
#9712 = FACE_OUTER_BOUND ( 'NONE', #13982, .T. ) ;
#9713 = CARTESIAN_POINT ( 'NONE',  ( -15.99999999999998579, 75.55999999999990280, 172.9900000000000091 ) ) ;
#9714 = EDGE_CURVE ( 'NONE', #24468, #26932, #5788, .T. ) ;
#9715 = FACE_OUTER_BOUND ( 'NONE', #34562, .T. ) ;
#9716 = VERTEX_POINT ( 'NONE', #21825 ) ;
#9717 = DIRECTION ( 'NONE',  ( 0.000000000000000000, 1.000000000000000000, 1.224646799147353207E-16 ) ) ;
#9718 = ORIENTED_EDGE ( 'NONE', *, *, #12979, .T. ) ;
#9719 = AXIS2_PLACEMENT_3D ( 'NONE', #6506, #17408, #28237 ) ;
#9720 = EDGE_CURVE ( 'NONE', #11190, #32452, #2725, .T. ) ;
#9722 = CARTESIAN_POINT ( 'NONE',  ( -442.0000000000000000, -125.0000000000000000, 104.0000000000000142 ) ) ;
#9721 = DIRECTION ( 'NONE',  ( -0.000000000000000000, 0.000000000000000000, -1.000000000000000000 ) ) ;
#9723 = FACE_OUTER_BOUND ( 'NONE', #16217, .T. ) ;
#9724 = EDGE_CURVE ( 'NONE', #7256, #23038, #27520, .T. ) ;
#9725 = AXIS2_PLACEMENT_3D ( 'NONE', #26417, #20562, #23580 ) ;
#9726 = ORIENTED_EDGE ( 'NONE', *, *, #11608, .T. ) ;
#9727 = EDGE_CURVE ( 'NONE', #25531, #18737, #33111, .T. ) ;
#9728 = ADVANCED_FACE ( 'NONE', ( #14262 ), #25090, .T. ) ;
#9729 = CARTESIAN_POINT ( 'NONE',  ( -418.0000000000000000, -105.0000000000000142, -73.99999999999998579 ) ) ;
#9730 = DIRECTION ( 'NONE',  ( 0.000000000000000000, 1.000000000000000000, 2.309213040847544338E-50 ) ) ;
#9731 = EDGE_CURVE ( 'NONE', #196, #27359, #34007, .T. ) ;
#9732 = ORIENTED_EDGE ( 'NONE', *, *, #31314, .T. ) ;
#9733 = VECTOR ( 'NONE', #8741, 1000.000000000000000 ) ;
#9734 = DIRECTION ( 'NONE',  ( -7.893605728314051750E-14, 1.618803117314786530E-15, 1.000000000000000000 ) ) ;
#9735 = AXIS2_PLACEMENT_3D ( 'NONE', #34546, #29388, #15343 ) ;
#9737 = VERTEX_POINT ( 'NONE', #3904 ) ;
#9736 = AXIS2_PLACEMENT_3D ( 'NONE', #4021, #17599, #4539 ) ;
#9738 = CARTESIAN_POINT ( 'NONE',  ( 2.789999999999999147, -0.09145294252654824485, -30.47036804522408460 ) ) ;
#9739 = ORIENTED_EDGE ( 'NONE', *, *, #1120, .F. ) ;
#9740 = VECTOR ( 'NONE', #7121, 1000.000000000000000 ) ;
#9741 = FACE_OUTER_BOUND ( 'NONE', #14669, .T. ) ;
#9742 = LINE ( 'NONE', #12599, #32320 ) ;
#9743 = DIRECTION ( 'NONE',  ( -0.000000000000000000, -0.000000000000000000, -1.000000000000000000 ) ) ;
#9744 = CARTESIAN_POINT ( 'NONE',  ( 1.040000000000002256, 27.68252950111368094, -20.44661865013457813 ) ) ;
#9745 = EDGE_LOOP ( 'NONE', ( #30235, #700, #24938, #11771 ) ) ;
#9746 = ORIENTED_EDGE ( 'NONE', *, *, #446, .T. ) ;
#9747 = ORIENTED_EDGE ( 'NONE', *, *, #21165, .F. ) ;
#9748 = AXIS2_PLACEMENT_3D ( 'NONE', #14503, #25333, #9503 ) ;
#9749 = DIRECTION ( 'NONE',  ( 3.697785493223492838E-32, 1.934419779023891545E-16, -1.000000000000000000 ) ) ;
#9751 = AXIS2_PLACEMENT_3D ( 'NONE', #11205, #16553, #29892 ) ;
#9750 = DIRECTION ( 'NONE',  ( 0.000000000000000000, 0.000000000000000000, -1.000000000000000000 ) ) ;
#9752 = LINE ( 'NONE', #1221, #22440 ) ;
#9753 = CARTESIAN_POINT ( 'NONE',  ( -26.18205399241665177, -19.33143609808336549, 68.31122994652405112 ) ) ;
#9754 = DIRECTION ( 'NONE',  ( -3.469446951953832974E-18, -1.000000000000000000, -7.888609052210116302E-31 ) ) ;
#9755 = CARTESIAN_POINT ( 'NONE',  ( -445.9999999999999432, 124.9999999999999574, -187.0000000000000000 ) ) ;
#9756 = VERTEX_POINT ( 'NONE', #11404 ) ;
#9757 = PRODUCT_DEFINITION_SHAPE ( 'NONE', 'NONE',  #35154 ) ;
#9758 = CARTESIAN_POINT ( 'NONE',  ( 110.4374853395854643, 1.870982065537967420, 12.36420004006153839 ) ) ;
#9759 = AXIS2_PLACEMENT_3D ( 'NONE', #19288, #27630, #30487 ) ;
#9760 = ORIENTED_EDGE ( 'NONE', *, *, #5076, .F. ) ;
#9761 = AXIS2_PLACEMENT_3D ( 'NONE', #32172, #28803, #15296 ) ;
#9762 = AXIS2_PLACEMENT_3D ( 'NONE', #28429, #28774, #7393 ) ;
#9764 = AXIS2_PLACEMENT_3D ( 'NONE', #9753, #23292, #34851 ) ;
#9763 = CARTESIAN_POINT ( 'NONE',  ( -445.9999999999999432, -124.9999999999999716, 132.0000000000000000 ) ) ;
#9765 = ORIENTED_EDGE ( 'NONE', *, *, #23235, .F. ) ;
#9766 = VECTOR ( 'NONE', #22777, 1000.000000000000000 ) ;
#9767 = DIRECTION ( 'NONE',  ( -1.000000000000000000, 0.000000000000000000, 0.000000000000000000 ) ) ;
#9768 = EDGE_CURVE ( 'NONE', #31064, #31497, #15734, .T. ) ;
#9769 = LINE ( 'NONE', #17633, #31480 ) ;
#9770 = EDGE_CURVE ( 'NONE', #14536, #3150, #25275, .T. ) ;
#9771 = EDGE_CURVE ( 'NONE', #15713, #13338, #14626, .T. ) ;
#9772 = CARTESIAN_POINT ( 'NONE',  ( 0.000000000000000000, -33.69708579775584667, 49.43553178847298568 ) ) ;
#9773 = CARTESIAN_POINT ( 'NONE',  ( 12.00000000000001066, 144.9999999999999716, -154.9999999999999716 ) ) ;
#9774 = SURFACE_STYLE_USAGE ( .BOTH. , #28301 ) ;
#9775 = ORIENTED_EDGE ( 'NONE', *, *, #6327, .F. ) ;
#9776 = CIRCLE ( 'NONE', #18805, 2.033421858999711951 ) ;
#9777 = ORIENTED_EDGE ( 'NONE', *, *, #28737, .T. ) ;
#9778 = CARTESIAN_POINT ( 'NONE',  ( 778.1305132547480525, 1139.399614022839842, 1753.598338701303192 ) ) ;
#9779 = ORIENTED_EDGE ( 'NONE', *, *, #29342, .T. ) ;
#9780 = EDGE_CURVE ( 'NONE', #23416, #5771, #22791, .T. ) ;
#9781 = AXIS2_PLACEMENT_3D ( 'NONE', #34871, #20984, #31823 ) ;
#9782 = LINE ( 'NONE', #25976, #29471 ) ;
#9783 = CARTESIAN_POINT ( 'NONE',  ( 107.9035335958860173, -4.962105133902832144, 5.629733210525461828 ) ) ;
#9784 = VECTOR ( 'NONE', #18154, 1000.000000000000000 ) ;
#9785 = ORIENTED_EDGE ( 'NONE', *, *, #2767, .T. ) ;
#9786 = B_SPLINE_CURVE_WITH_KNOTS ( 'NONE', 3,
 ( #9551, #12236, #26255, #4525, #23254, #20410, #25734, #31253 ),
 .UNSPECIFIED., .F., .F.,
 ( 4, 2, 2, 4 ),
 ( 0.007886720825438849058, 0.009850969036564048015, 0.01181521724768924697, 0.01574371366993964488 ),
 .UNSPECIFIED. ) ;
#9787 = DIRECTION ( 'NONE',  ( -0.000000000000000000, -1.000000000000000000, -0.000000000000000000 ) ) ;
#9788 = CARTESIAN_POINT ( 'NONE',  ( -418.0000000000000568, 141.0000000000000000, -155.0000000000000000 ) ) ;
#9789 = ADVANCED_FACE ( 'NONE', ( #11593 ), #8905, .T. ) ;
#9790 = EDGE_CURVE ( 'NONE', #26110, #2088, #12126, .T. ) ;
#9792 = CARTESIAN_POINT ( 'NONE',  ( 10.62930655775863364, -36.34639295086972766, 68.31122994652405112 ) ) ;
#9791 = CARTESIAN_POINT ( 'NONE',  ( 5.021133111224576062, 18.16264470403145381, -87.50000000000000000 ) ) ;
#9793 = ORIENTED_EDGE ( 'NONE', *, *, #24341, .F. ) ;
#9794 = ORIENTED_EDGE ( 'NONE', *, *, #28371, .F. ) ;
#9795 = CARTESIAN_POINT ( 'NONE',  ( -12.00000000000001066, 124.9999999999999716, 162.9999999999999716 ) ) ;
#9796 = ORIENTED_EDGE ( 'NONE', *, *, #18407, .F. ) ;
#9797 = EDGE_CURVE ( 'NONE', #24623, #24780, #9085, .T. ) ;
#9798 = DIRECTION ( 'NONE',  ( -1.000000000000000000, -0.000000000000000000, 0.000000000000000000 ) ) ;
#9799 = CARTESIAN_POINT ( 'NONE',  ( -4.850000000000000533, 0.000000000000000000, 0.000000000000000000 ) ) ;
#9800 = ORIENTED_EDGE ( 'NONE', *, *, #7704, .F. ) ;
#9801 = DIRECTION ( 'NONE',  ( 0.000000000000000000, 1.131431318426415506E-52, 1.000000000000000000 ) ) ;
#9802 = PRODUCT_DEFINITION_SHAPE ( 'NONE', 'NONE',  #35122 ) ;
#9803 = VERTEX_POINT ( 'NONE', #30628 ) ;
#9804 = DIRECTION ( 'NONE',  ( 0.000000000000000000, 0.000000000000000000, -1.000000000000000000 ) ) ;
#9805 = DIRECTION ( 'NONE',  ( 0.000000000000000000, 1.836970198721029441E-16, -1.000000000000000000 ) ) ;
#9806 = CARTESIAN_POINT ( 'NONE',  ( 0.000000000000000000, 29.94779062842797401, -5.619744560738746841 ) ) ;
#9808 = CARTESIAN_POINT ( 'NONE',  ( -449.9999999999999432, -125.0000000000000000, 107.9999999999999858 ) ) ;
#9807 = CARTESIAN_POINT ( 'NONE',  ( -365.0000000000000000, -125.0000000000000000, 113.9999999999999858 ) ) ;
#9809 = VECTOR ( 'NONE', #25964, 1000.000000000000000 ) ;
#9810 = ADVANCED_FACE ( 'NONE', ( #6220, #14794 ), #17115, .T. ) ;
#9811 = CIRCLE ( 'NONE', #6953, 0.3000000000000016542 ) ;
#9812 = DIRECTION ( 'NONE',  ( -1.000000000000000000, 0.000000000000000000, 0.000000000000000000 ) ) ;
#9813 = LINE ( 'NONE', #4983, #4025 ) ;
#9814 = CARTESIAN_POINT ( 'NONE',  ( -20.00000000000001776, -141.0000000000000000, -186.9999999999999716 ) ) ;
#9815 = VERTEX_POINT ( 'NONE', #5866 ) ;
#9816 =( NAMED_UNIT ( * ) PLANE_ANGLE_UNIT ( ) SI_UNIT ( $, .RADIAN. ) );
#9817 = ORIENTED_EDGE ( 'NONE', *, *, #721, .T. ) ;
#9818 = ORIENTED_EDGE ( 'NONE', *, *, #31569, .T. ) ;
#9819 = CARTESIAN_POINT ( 'NONE',  ( 0.000000000000000000, 0.000000000000000000, -62.49999999999999289 ) ) ;
#9820 = ORIENTED_EDGE ( 'NONE', *, *, #22567, .F. ) ;
#9821 = VERTEX_POINT ( 'NONE', #17298 ) ;
#9822 = ORIENTED_EDGE ( 'NONE', *, *, #13916, .F. ) ;
#9823 = CARTESIAN_POINT ( 'NONE',  ( -19.99999999999998934, -137.0000000000000000, 187.0000000000000000 ) ) ;
#9824 = EDGE_CURVE ( 'NONE', #25488, #32966, #27596, .T. ) ;
#9825 = AXIS2_PLACEMENT_3D ( 'NONE', #11943, #20642, #12468 ) ;
#9826 = EDGE_CURVE ( 'NONE', #23287, #20094, #30978, .T. ) ;
#9827 = ORIENTED_EDGE ( 'NONE', *, *, #1886, .F. ) ;
#9828 = DIRECTION ( 'NONE',  ( 0.000000000000000000, 0.000000000000000000, 1.000000000000000000 ) ) ;
#9829 = AXIS2_PLACEMENT_3D ( 'NONE', #21284, #18797, #12577 ) ;
#9830 = DIRECTION ( 'NONE',  ( -0.000000000000000000, -0.000000000000000000, -1.000000000000000000 ) ) ;
#9831 = EDGE_LOOP ( 'NONE', ( #31530, #28247, #28011, #7008 ) ) ;
#9832=STYLED_ITEM('',(#35254),#34584);
#9833 = ORIENTED_EDGE ( 'NONE', *, *, #22980, .T. ) ;
#9834 = VECTOR ( 'NONE', #27095, 1000.000000000000000 ) ;
#9835 = DIRECTION ( 'NONE',  ( -0.9985334138511239299, 0.05413890858541762358, 0.000000000000000000 ) ) ;
#9836 = CARTESIAN_POINT ( 'NONE',  ( 0.02407890056655738464, -27.96208973699912548, 13.59246946040177129 ) ) ;
#9837 = CARTESIAN_POINT ( 'NONE',  ( -29.68486519896224962, 23.49918569563713078, -36.68877005347593467 ) ) ;
#9838 = LINE ( 'NONE', #33697, #11415 ) ;
#9839 = CARTESIAN_POINT ( 'NONE',  ( 2.790000000000081748, 25.77088461036980505, 16.61521147790390884 ) ) ;
#9840 = VERTEX_POINT ( 'NONE', #24916 ) ;
#9841 = LINE ( 'NONE', #23542, #6095 ) ;
#9842 = CARTESIAN_POINT ( 'NONE',  ( -42.55956070192387841, -20.15143121711728469, 20.00000000000000000 ) ) ;
#9843 = CYLINDRICAL_SURFACE ( 'NONE', #9650, 3.999999999999976019 ) ;
#9844 = ORIENTED_EDGE ( 'NONE', *, *, #19064, .T. ) ;
#9845 = EDGE_CURVE ( 'NONE', #23220, #32949, #6581, .T. ) ;
#9846 = LINE ( 'NONE', #23372, #24173 ) ;
#9847 = LINE ( 'NONE', #7513, #21205 ) ;
#9848 = CARTESIAN_POINT ( 'NONE',  ( 110.7380848894539866, -2.712459438615764475E-14, -7.500000000000241585 ) ) ;
#9850 = CARTESIAN_POINT ( 'NONE',  ( -110.1150203881708194, 0.3508469386294343906, -7.500000000000001776 ) ) ;
#9849 = DIRECTION ( 'NONE',  ( 0.000000000000000000, 0.000000000000000000, 1.000000000000000000 ) ) ;
#9851 = VECTOR ( 'NONE', #23042, 1000.000000000000000 ) ;
#9852 = DIRECTION ( 'NONE',  ( -1.000000000000000000, -0.000000000000000000, -0.000000000000000000 ) ) ;
#9853 = ORIENTED_EDGE ( 'NONE', *, *, #15855, .F. ) ;
#9854 = CARTESIAN_POINT ( 'NONE',  ( 99.26191511054634020, 0.3849557905273010561, -12.50000000000000533 ) ) ;
#9856 = DIRECTION ( 'NONE',  ( 1.000000000000000000, 0.000000000000000000, 0.000000000000000000 ) ) ;
#9855 = CYLINDRICAL_SURFACE ( 'NONE', #8665, 22.50000000000000355 ) ;
#9857 = AXIS2_PLACEMENT_3D ( 'NONE', #14216, #25222, #5643 ) ;
#9859 = ORIENTED_EDGE ( 'NONE', *, *, #14620, .T. ) ;
#9858 = CIRCLE ( 'NONE', #17858, 7.999999999999979572 ) ;
#9860 = AXIS2_PLACEMENT_3D ( 'NONE', #25826, #26351, #31852 ) ;
#9861 = PRODUCT_DEFINITION_SHAPE ( 'NONE', 'NONE',  #35197 ) ;
#9862 = DIRECTION ( 'NONE',  ( 0.000000000000000000, -1.000000000000000000, 0.000000000000000000 ) ) ;
#9863 = EDGE_CURVE ( 'NONE', #35069, #25265, #12435, .T. ) ;
#9864 = ORIENTED_EDGE ( 'NONE', *, *, #12591, .F. ) ;
#9865 = VERTEX_POINT ( 'NONE', #16947 ) ;
#9866 = DIRECTION ( 'NONE',  ( 0.000000000000000000, 1.000000000000000000, -6.842277657836020854E-49 ) ) ;
#9867 = ORIENTED_EDGE ( 'NONE', *, *, #801, .F. ) ;
#9868 = ORIENTED_EDGE ( 'NONE', *, *, #2272, .T. ) ;
#9869 = DIRECTION ( 'NONE',  ( -0.000000000000000000, 1.000000000000000000, -0.000000000000000000 ) ) ;
#9870 = EDGE_CURVE ( 'NONE', #22350, #14078, #10134, .T. ) ;
#9871 = EDGE_CURVE ( 'NONE', #12372, #21269, #5004, .T. ) ;
#9872 = EDGE_CURVE ( 'NONE', #11743, #31368, #1767, .T. ) ;
#9873 = CONICAL_SURFACE ( 'NONE', #20127, 13.50000000000000000, 1.047197551196600296 ) ;
#9874 = CARTESIAN_POINT ( 'NONE',  ( -35.00000000000000000, -7.062798427011560243, 17.20188834027727154 ) ) ;
#9875 = DIRECTION ( 'NONE',  ( -0.000000000000000000, -0.000000000000000000, 1.000000000000000000 ) ) ;
#9876 = ORIENTED_EDGE ( 'NONE', *, *, #11333, .F. ) ;
#9877 = VERTEX_POINT ( 'NONE', #7096 ) ;
#9878 = CARTESIAN_POINT ( 'NONE',  ( 37.71145559917817280, 3.353962854566119756, 68.31122994652405112 ) ) ;
#9879 = CARTESIAN_POINT ( 'NONE',  ( 0.006892406498510319189, -30.26126365281900732, -6.099214421700076549 ) ) ;
#9880 = CARTESIAN_POINT ( 'NONE',  ( -355.0000000000000000, -117.0000000000000000, 113.9999999999999858 ) ) ;
#9881 = CARTESIAN_POINT ( 'NONE',  ( 2.783128942071183332, -30.82708482934415528, 1.618146408792505708 ) ) ;
#9882 = CARTESIAN_POINT ( 'NONE',  ( 15.99999999999998579, -32.99999999999997158, -154.9999999999999716 ) ) ;
#9883 = EDGE_LOOP ( 'NONE', ( #3072, #28088, #19507, #32124 ) ) ;
#9884 = PRODUCT_DEFINITION_FORMATION_WITH_SPECIFIED_SOURCE ( 'ANY', '', #16613, .NOT_KNOWN. ) ;
#9885 = ORIENTED_EDGE ( 'NONE', *, *, #21699, .T. ) ;
#9886 = CARTESIAN_POINT ( 'NONE',  ( -8.267476927982267298, 31.47782073335737962, -36.68877005347593467 ) ) ;
#9887 = AXIS2_PLACEMENT_3D ( 'NONE', #48, #13413, #27099 ) ;
#9888 = VECTOR ( 'NONE', #29343, 1000.000000000000114 ) ;
#9889 = CARTESIAN_POINT ( 'NONE',  ( 0.000000000000000000, -20.92506858792774338, 22.14933852381670221 ) ) ;
#9890 = ORIENTED_EDGE ( 'NONE', *, *, #8713, .F. ) ;
#9891 = DIRECTION ( 'NONE',  ( 0.000000000000000000, 0.000000000000000000, 1.000000000000000000 ) ) ;
#9892 = FACE_OUTER_BOUND ( 'NONE', #32212, .T. ) ;
#9893 = CARTESIAN_POINT ( 'NONE',  ( 2.789999999999999147, -26.45933846664205902, 16.32596387352436551 ) ) ;
#9894 = ORIENTED_EDGE ( 'NONE', *, *, #171, .F. ) ;
#9895 =( REPRESENTATION_RELATIONSHIP ('NONE','NONE', #23037, #28231 ) REPRESENTATION_RELATIONSHIP_WITH_TRANSFORMATION ( #29577 )SHAPE_REPRESENTATION_RELATIONSHIP( ) );
#9896 = DIRECTION ( 'NONE',  ( -1.000000000000000000, 0.000000000000000000, 0.000000000000000000 ) ) ;
#9897 = ORIENTED_EDGE ( 'NONE', *, *, #7162, .F. ) ;
#9899 = DIRECTION ( 'NONE',  ( -1.000000000000000000, -0.000000000000000000, 0.000000000000000000 ) ) ;
#9898 = CARTESIAN_POINT ( 'NONE',  ( -5.210000000000000853, 0.000000000000000000, 0.000000000000000000 ) ) ;
#9900 = DIRECTION ( 'NONE',  ( 1.000000000000000000, 0.000000000000000000, -0.000000000000000000 ) ) ;
#9901 = AXIS2_PLACEMENT_3D ( 'NONE', #5959, #16861, #22178 ) ;
#9902 = ORIENTED_EDGE ( 'NONE', *, *, #7, .F. ) ;
#9903 = FACE_OUTER_BOUND ( 'NONE', #34611, .T. ) ;
#9904 = CARTESIAN_POINT ( 'NONE',  ( -445.9999999999999432, -112.9999999999999858, -174.9999999999999716 ) ) ;
#9905 = CIRCLE ( 'NONE', #29799, 2.000000000000001776 ) ;
#9906 = ORIENTED_EDGE ( 'NONE', *, *, #24004, .F. ) ;
#9907 = DIRECTION ( 'NONE',  ( 0.000000000000000000, 0.000000000000000000, -1.000000000000000000 ) ) ;
#9908 = VECTOR ( 'NONE', #1152, 1000.000000000000000 ) ;
#9909 = CARTESIAN_POINT ( 'NONE',  ( 787.1205540725626406, 1055.379251081385291, 1753.598338701303419 ) ) ;
#9910 = AXIS2_PLACEMENT_3D ( 'NONE', #3246, #13764, #7885 ) ;
#9911 = EDGE_CURVE ( 'NONE', #32668, #15683, #26146, .T. ) ;
#9912 = ORIENTED_EDGE ( 'NONE', *, *, #5681, .T. ) ;
#9913 = CARTESIAN_POINT ( 'NONE',  ( 104.9965108525136372, -5.747432480335291416, 11.10030588989970468 ) ) ;
#9914 = ORIENTED_EDGE ( 'NONE', *, *, #6208, .F. ) ;
#9915 = FACE_OUTER_BOUND ( 'NONE', #30134, .T. ) ;
#9916 = VECTOR ( 'NONE', #11448, 1000.000000000000000 ) ;
#9917 = EDGE_CURVE ( 'NONE', #29345, #13451, #11051, .T. ) ;
#9918 = CARTESIAN_POINT ( 'NONE',  ( -361.0000000000000000, -125.0000000000000284, 168.9999999999999716 ) ) ;
#9919 = EDGE_CURVE ( 'NONE', #18651, #17757, #12994, .T. ) ;
#9920 = CARTESIAN_POINT ( 'NONE',  ( -110.0792196684870987, -0.6954373895739790479, -7.475453221064620735 ) ) ;
#9921 = FACE_OUTER_BOUND ( 'NONE', #27649, .T. ) ;
#9922 = CONTEXT_DEPENDENT_SHAPE_REPRESENTATION ( #30795, #31638 ) ;
#9923 = ORIENTED_EDGE ( 'NONE', *, *, #34707, .T. ) ;
#9924 = ORIENTED_EDGE ( 'NONE', *, *, #2365, .T. ) ;
#9925 = VERTEX_POINT ( 'NONE', #34161 ) ;
#9926 = ADVANCED_FACE ( 'NONE', ( #9448 ), #28820, .F. ) ;
#9927 = DIRECTION ( 'NONE',  ( 0.000000000000000000, -0.9961946980917453232, 0.08715574274766170471 ) ) ;
#9928 = FACE_OUTER_BOUND ( 'NONE', #9686, .T. ) ;
#9929 = VECTOR ( 'NONE', #8595, 1000.000000000000000 ) ;
#9930 = DIRECTION ( 'NONE',  ( -1.000000000000000000, 0.000000000000000000, 0.000000000000000000 ) ) ;
#9931 = DIRECTION ( 'NONE',  ( -1.000000000000000000, -3.040835319149746090E-31, -1.232595164407830946E-32 ) ) ;
#9932 = CARTESIAN_POINT ( 'NONE',  ( -365.0000000000000000, -133.0000000000000000, 113.9999999999999858 ) ) ;
#9933 = DIRECTION ( 'NONE',  ( 0.000000000000000000, 0.000000000000000000, -1.000000000000000000 ) ) ;
#9934 = EDGE_LOOP ( 'NONE', ( #4304, #33120, #33762, #2372, #2993, #19662 ) ) ;
#9935 = CIRCLE ( 'NONE', #29828, 2.036051781435508801 ) ;
#9936 = CARTESIAN_POINT ( 'NONE',  ( 1.749999999999999778, 32.09669216789236401, 12.41728656686386500 ) ) ;
#9937 = EDGE_CURVE ( 'NONE', #2161, #11922, #25838, .T. ) ;
#9938 = CARTESIAN_POINT ( 'NONE',  ( 0.02407890056655911937, -15.32140196853734970, -27.05343472113007763 ) ) ;
#9939 = AXIS2_PLACEMENT_3D ( 'NONE', #8212, #2521, #32771 ) ;
#9940 = VERTEX_POINT ( 'NONE', #7269 ) ;
#9941=STYLED_ITEM('',(#35289),#33586);
#9942 = VECTOR ( 'NONE', #24909, 1000.000000000000000 ) ;
#9943 = LINE ( 'NONE', #18157, #30876 ) ;
#9944 = ORIENTED_EDGE ( 'NONE', *, *, #1601, .T. ) ;
#9946 = AXIS2_PLACEMENT_3D ( 'NONE', #3865, #6359, #1727 ) ;
#9945 = DIRECTION ( 'NONE',  ( -3.469446951953832974E-18, -1.000000000000000000, -7.888609052210116302E-31 ) ) ;
#9947 = DIRECTION ( 'NONE',  ( -1.300283923313630633E-47, 0.000000000000000000, -1.000000000000000000 ) ) ;
#9948 = DIRECTION ( 'NONE',  ( -1.000000000000000000, 0.000000000000000000, 0.000000000000000000 ) ) ;
#9949 = LINE ( 'NONE', #6912, #7663 ) ;
#9950 = LINE ( 'NONE', #20294, #34787 ) ;
#9951 = ORIENTED_EDGE ( 'NONE', *, *, #27804, .T. ) ;
#9952 = VECTOR ( 'NONE', #27424, 1000.000000000000000 ) ;
#9953 = VERTEX_POINT ( 'NONE', #17998 ) ;
#9954 = DIRECTION ( 'NONE',  ( -0.2986177215767074067, -0.9543728078483458832, -1.401405946928635035E-14 ) ) ;
#9955 = AXIS2_PLACEMENT_3D ( 'NONE', #7917, #15953, #2057 ) ;
#9956 = ORIENTED_EDGE ( 'NONE', *, *, #25260, .F. ) ;
#9957 = AXIS2_PLACEMENT_3D ( 'NONE', #9549, #17579, #17410 ) ;
#9958 = CARTESIAN_POINT ( 'NONE',  ( -8.000000000000000000, 0.000000000000000000, 0.000000000000000000 ) ) ;
#9959 = LINE ( 'NONE', #9123, #21827 ) ;
#9960 = CARTESIAN_POINT ( 'NONE',  ( 109.9257156030288911, -2.949151772667967020, 6.898053038626237310 ) ) ;
#9961 = ORIENTED_EDGE ( 'NONE', *, *, #25922, .F. ) ;
#9962 = EDGE_CURVE ( 'NONE', #9066, #7094, #18169, .T. ) ;
#9963 = CARTESIAN_POINT ( 'NONE',  ( 0.000000000000000000, 3.524919873834583163E-15, 68.31122994652405112 ) ) ;
#9964 =( GEOMETRIC_REPRESENTATION_CONTEXT ( 3 ) GLOBAL_UNCERTAINTY_ASSIGNED_CONTEXT ( ( #10234 ) ) GLOBAL_UNIT_ASSIGNED_CONTEXT ( ( #3448, #6649, #14342 ) ) REPRESENTATION_CONTEXT ( 'NONE', 'WORKASPACE' ) );
#9965 = EDGE_CURVE ( 'NONE', #2856, #16456, #9782, .T. ) ;
#9967 = CARTESIAN_POINT ( 'NONE',  ( -12.00000000000001066, -124.9999999999999432, -162.9999999999999432 ) ) ;
#9966 = CARTESIAN_POINT ( 'NONE',  ( 0.000000000000000000, 33.69708579775584667, 49.43553178847298568 ) ) ;
#9968 = ORIENTED_EDGE ( 'NONE', *, *, #7606, .T. ) ;
#9969 = ORIENTED_EDGE ( 'NONE', *, *, #7545, .T. ) ;
#9970 = EDGE_CURVE ( 'NONE', #6016, #14870, #1600, .T. ) ;
#9971 = EDGE_CURVE ( 'NONE', #19731, #10833, #12985, .T. ) ;
#9972 = LINE ( 'NONE', #29190, #20848 ) ;
#9973 = ORIENTED_EDGE ( 'NONE', *, *, #15306, .F. ) ;
#9974 = CARTESIAN_POINT ( 'NONE',  ( 0.006892381195637166565, 30.78707849925352491, 2.258378142202824179 ) ) ;
#9975 = CARTESIAN_POINT ( 'NONE',  ( -8.204391965473290931E-14, -21.14989222980530670, -22.20103112977927395 ) ) ;
#9976 = VERTEX_POINT ( 'NONE', #26325 ) ;
#9977 = VECTOR ( 'NONE', #22724, 1000.000000000000000 ) ;
#9978 = CARTESIAN_POINT ( 'NONE',  ( -442.0000000000000000, -105.0000000000000142, 132.0000000000000000 ) ) ;
#9979 = VERTEX_POINT ( 'NONE', #20645 ) ;
#9980 = VECTOR ( 'NONE', #609, 1000.000000000000000 ) ;
#9981 = CARTESIAN_POINT ( 'NONE',  ( 0.000000000000000000, 0.000000000000000000, 0.000000000000000000 ) ) ;
#9982 = EDGE_CURVE ( 'NONE', #5461, #19524, #32225, .T. ) ;
#9983 = LINE ( 'NONE', #15696, #2459 ) ;
#9985 = CARTESIAN_POINT ( 'NONE',  ( -15.64512930492131382, -28.53829535743846435, 68.31122994652405112 ) ) ;
#9984 = DIRECTION ( 'NONE',  ( -1.000000000000000000, 0.000000000000000000, 0.000000000000000000 ) ) ;
#9986 = CARTESIAN_POINT ( 'NONE',  ( 2.789999999999999147, 7.489092610871509237, -29.53582882395378562 ) ) ;
#9987 = DIRECTION ( 'NONE',  ( -0.000000000000000000, -0.000000000000000000, 1.000000000000000000 ) ) ;
#9988 = CARTESIAN_POINT ( 'NONE',  ( -355.0000000000000000, -119.0000000000000000, 130.0000000000000000 ) ) ;
#9989 = CARTESIAN_POINT ( 'NONE',  ( 1.040000000000001590, -30.02688531850382958, -16.81585001935613022 ) ) ;
#9990 = VECTOR ( 'NONE', #14470, 1000.000000000000000 ) ;
#9991 = EDGE_CURVE ( 'NONE', #23775, #11101, #20990, .T. ) ;
#9992 = VERTEX_POINT ( 'NONE', #7444 ) ;
#9993 = EDGE_CURVE ( 'NONE', #7844, #25655, #8991, .T. ) ;
#9994 =( NAMED_UNIT ( * ) SI_UNIT ( $, .STERADIAN. ) SOLID_ANGLE_UNIT ( ) );
#9995 = ORIENTED_EDGE ( 'NONE', *, *, #12636, .F. ) ;
#9996 = ORIENTED_EDGE ( 'NONE', *, *, #28646, .T. ) ;
#9997 = CARTESIAN_POINT ( 'NONE',  ( -449.9999999999999432, 105.0000000000000142, -101.9999999999999858 ) ) ;
#9998 = DIRECTION ( 'NONE',  ( 0.1063910735369155841, -0.9943243633099125844, -3.335902418025060287E-15 ) ) ;
#9999 = ORIENTED_EDGE ( 'NONE', *, *, #28452, .T. ) ;
#10000 = VERTEX_POINT ( 'NONE', #20304 ) ;
#10001 = ORIENTED_EDGE ( 'NONE', *, *, #27373, .F. ) ;
#10002 = DIRECTION ( 'NONE',  ( 1.000000000000000000, 0.000000000000000000, -0.000000000000000000 ) ) ;
#10003 = CIRCLE ( 'NONE', #25941, 3.999999999999982681 ) ;
#10004 = CONTEXT_DEPENDENT_SHAPE_REPRESENTATION ( #9687, #15567 ) ;
#10005 = ORIENTED_EDGE ( 'NONE', *, *, #21025, .T. ) ;
#10006 = DIRECTION ( 'NONE',  ( -1.000000000000000000, -0.000000000000000000, -0.000000000000000000 ) ) ;
#10007 = DIRECTION ( 'NONE',  ( 0.000000000000000000, 1.000000000000000000, -3.374343856708137958E-53 ) ) ;
#10008 = VERTEX_POINT ( 'NONE', #31158 ) ;
#10009 = ORIENTED_EDGE ( 'NONE', *, *, #23785, .T. ) ;
#10010 = EDGE_CURVE ( 'NONE', #2254, #14577, #22642, .T. ) ;
#10011 = EDGE_CURVE ( 'NONE', #31407, #23007, #31316, .T. ) ;
#10012 = CARTESIAN_POINT ( 'NONE',  ( -35.55956070192387841, -32.65143121711728469, 10.00000000000000000 ) ) ;
#10013 = DIRECTION ( 'NONE',  ( -1.000000000000000000, -0.000000000000000000, -0.000000000000000000 ) ) ;
#10014 = CIRCLE ( 'NONE', #16851, 2.525000000000001688 ) ;
#10015 = CARTESIAN_POINT ( 'NONE',  ( 0.02407890056655651728, 29.44518845714764765, 9.980709654879525772 ) ) ;
#10016 = ADVANCED_FACE ( 'NONE', ( #16194 ), #10672, .F. ) ;
#10017 = DIRECTION ( 'NONE',  ( 0.2149704402110236556, 0.9766205557100866574, 0.000000000000000000 ) ) ;
#10018 = CARTESIAN_POINT ( 'NONE',  ( 2.783128888645070464, 25.89075856630346095, 16.81059844634668821 ) ) ;
#10019 = EDGE_LOOP ( 'NONE', ( #1200, #29014, #18652, #6599 ) ) ;
#10020 = DIRECTION ( 'NONE',  ( -0.000000000000000000, 5.145227585319922065E-49, 1.000000000000000000 ) ) ;
#10022 = AXIS2_PLACEMENT_3D ( 'NONE', #14888, #11688, #33555 ) ;
#10021 = CARTESIAN_POINT ( 'NONE',  ( -12.00000000000001066, 144.9999999999999716, -158.9999999999999716 ) ) ;
#10023 = VERTEX_POINT ( 'NONE', #5126 ) ;
#10024 = FACE_OUTER_BOUND ( 'NONE', #5946, .T. ) ;
#10025 = PLANE ( 'NONE',  #24035 ) ;
#10026 = CARTESIAN_POINT ( 'NONE',  ( 106.5416737992720755, 5.530333585247596773, -5.066783516361279993 ) ) ;
#10028 = CARTESIAN_POINT ( 'NONE',  ( -430.0000000000000000, -131.0000000000000000, 109.9999999999999858 ) ) ;
#10027 = CARTESIAN_POINT ( 'NONE',  ( -9.978866888775527855, 8.235406450278427215, -67.50000000000000000 ) ) ;
#10029 = CIRCLE ( 'NONE', #11183, 2.525000000000001688 ) ;
#10030 = CARTESIAN_POINT ( 'NONE',  ( -361.0000000000000000, -135.0000000000000000, 130.0000000000000000 ) ) ;
#10031 = ORIENTED_EDGE ( 'NONE', *, *, #2275, .T. ) ;
#10032 = CARTESIAN_POINT ( 'NONE',  ( 101.2072798900310175, 4.321688686550378300, -11.73238900788529904 ) ) ;
#10034 = DIRECTION ( 'NONE',  ( -0.000000000000000000, 1.000000000000000000, -0.000000000000000000 ) ) ;
#10033 = SURFACE_STYLE_FILL_AREA ( #18073 ) ;
#10035 = VECTOR ( 'NONE', #22155, 1000.000000000000000 ) ;
#10036 = EDGE_CURVE ( 'NONE', #14959, #13078, #8420, .T. ) ;
#10037 = EDGE_CURVE ( 'NONE', #9496, #21957, #26851, .T. ) ;
#10038 = ORIENTED_EDGE ( 'NONE', *, *, #9483, .T. ) ;
#10039 = CARTESIAN_POINT ( 'NONE',  ( 145.0000000000000568, -177.8172209610550851, -45.87893859614474223 ) ) ;
#10040 = AXIS2_PLACEMENT_3D ( 'NONE', #19504, #18977, #21988 ) ;
#10041 = ADVANCED_FACE ( 'NONE', ( #21861 ), #13861, .F. ) ;
#10042 = ORIENTED_EDGE ( 'NONE', *, *, #882, .T. ) ;
#10043 = ADVANCED_FACE ( 'NONE', ( #27375 ), #32362, .F. ) ;
#10044 = EDGE_CURVE ( 'NONE', #32813, #27322, #10127, .T. ) ;
#10045 = VERTEX_POINT ( 'NONE', #18861 ) ;
#10046 = CARTESIAN_POINT ( 'NONE',  ( 2.789999999999999147, -1.291199951813412738, 30.41225463960052267 ) ) ;
#10047 = VERTEX_POINT ( 'NONE', #32717 ) ;
#10048 = ORIENTED_EDGE ( 'NONE', *, *, #16649, .T. ) ;
#10049 = CARTESIAN_POINT ( 'NONE',  ( 0.000000000000000000, 49.99999999999999289, -9.999999999999998224 ) ) ;
#10050 = PRODUCT_DEFINITION_SHAPE ( 'NONE', 'NONE',  #35169 ) ;
#10051 = AXIS2_PLACEMENT_3D ( 'NONE', #13533, #19063, #8362 ) ;
#10052 = AXIS2_PLACEMENT_3D ( 'NONE', #4226, #33609, #879 ) ;
#10053 = CARTESIAN_POINT ( 'NONE',  ( 19.99999999999998934, 75.55999999999990280, -172.9900000000000091 ) ) ;
#10054 = CARTESIAN_POINT ( 'NONE',  ( 12.00000000000001066, -145.0000000000000000, 155.0000000000000000 ) ) ;
#10055 = VERTEX_POINT ( 'NONE', #5647 ) ;
#10056 = ORIENTED_EDGE ( 'NONE', *, *, #6279, .F. ) ;
#10057 = PLANE ( 'NONE',  #19648 ) ;
#10058 = DIRECTION ( 'NONE',  ( 0.000000000000000000, 1.836970198721029441E-16, -1.000000000000000000 ) ) ;
#10059 = DIRECTION ( 'NONE',  ( -1.000000000000000000, 0.000000000000000000, 0.000000000000000000 ) ) ;
#10060 = MANIFOLD_SOLID_BREP ( 'Boss-Extrude1', #33097 ) ;
#10061 = CARTESIAN_POINT ( 'NONE',  ( -19.99999999999998934, -32.99999999999997158, 154.9999999999999716 ) ) ;
#10062 = PLANE ( 'NONE',  #23361 ) ;
#10063 = ORIENTED_EDGE ( 'NONE', *, *, #2125, .T. ) ;
#10064 = ORIENTED_EDGE ( 'NONE', *, *, #10081, .T. ) ;
#10065 = CARTESIAN_POINT ( 'NONE',  ( -12.00000000000001243, 144.9999999999999716, -154.9999999999999716 ) ) ;
#10066 = CYLINDRICAL_SURFACE ( 'NONE', #541, 3.999999999999948042 ) ;
#10067 = ORIENTED_EDGE ( 'NONE', *, *, #16761, .F. ) ;
#10068 = CARTESIAN_POINT ( 'NONE',  ( -12.00000000000001066, -145.0000000000000000, -186.9999999999999716 ) ) ;
#10069 = CARTESIAN_POINT ( 'NONE',  ( 11.99999999999999645, 140.9999999999999716, -175.0000000000000284 ) ) ;
#10070 = ORIENTED_EDGE ( 'NONE', *, *, #17795, .T. ) ;
#10071 = CARTESIAN_POINT ( 'NONE',  ( -361.0000000000000000, -135.0000000000000000, 110.0000000000000000 ) ) ;
#10072 = ORIENTED_EDGE ( 'NONE', *, *, #22901, .T. ) ;
#10073 = CARTESIAN_POINT ( 'NONE',  ( -19.99999999999998934, -134.9999999999999716, 187.0000000000000000 ) ) ;
#10074 = ORIENTED_EDGE ( 'NONE', *, *, #6784, .F. ) ;
#10076 = CARTESIAN_POINT ( 'NONE',  ( 9.736651044630743712, -33.69708579775584667, 68.31122994652405112 ) ) ;
#10075 = CARTESIAN_POINT ( 'NONE',  ( 11.99999999999999645, -145.0000000000000000, 162.9999999999999716 ) ) ;
#10077 = CARTESIAN_POINT ( 'NONE',  ( -499.9999999999998863, -109.0000000000000142, -187.0000000000000000 ) ) ;
#10078 = VECTOR ( 'NONE', #7379, 1000.000000000000000 ) ;
#10079 = ADVANCED_FACE ( 'NONE', ( #16374 ), #27204, .F. ) ;
#10080 = AXIS2_PLACEMENT_3D ( 'NONE', #8310, #5273, #32334 ) ;
#10081 = EDGE_CURVE ( 'NONE', #4047, #6854, #16018, .T. ) ;
#10082 = ORIENTED_EDGE ( 'NONE', *, *, #16461, .T. ) ;
#10083 = CARTESIAN_POINT ( 'NONE',  ( -12.00000000000001066, -109.0000000000000142, -155.0000000000000284 ) ) ;
#10084 = CARTESIAN_POINT ( 'NONE',  ( -442.0000000000000000, -125.0000000000000000, 194.9999999999999716 ) ) ;
#10085 = ORIENTED_EDGE ( 'NONE', *, *, #5624, .F. ) ;
#10086 = AXIS2_PLACEMENT_3D ( 'NONE', #10977, #35024, #30021 ) ;
#10087 = DIRECTION ( 'NONE',  ( -0.1053217285638884393, 0.9944381999361825430, -9.979632055086323115E-15 ) ) ;
#10088 = ORIENTED_EDGE ( 'NONE', *, *, #6083, .F. ) ;
#10089 = CARTESIAN_POINT ( 'NONE',  ( 110.1379535922845463, -2.561659524636492602, 12.23586498300001679 ) ) ;
#10090 = ORIENTED_EDGE ( 'NONE', *, *, #9447, .T. ) ;
#10091 = DIRECTION ( 'NONE',  ( -1.000000000000000000, -0.000000000000000000, -0.000000000000000000 ) ) ;
#10092 = CARTESIAN_POINT ( 'NONE',  ( 1.040000000000000924, -10.37741591188871482, -32.81304455236878681 ) ) ;
#10093 = AXIS2_PLACEMENT_3D ( 'NONE', #1056, #33266, #6021 ) ;
#10094 = CARTESIAN_POINT ( 'NONE',  ( -104.3101933623550792, -5.079998963781827470, -5.518357322521168840 ) ) ;
#10095 = CARTESIAN_POINT ( 'NONE',  ( -449.9999999999999432, 137.0000000000000000, -175.0000000000000000 ) ) ;
#10096 = CONTEXT_DEPENDENT_SHAPE_REPRESENTATION ( #28765, #22537 ) ;
#10097 = VERTEX_POINT ( 'NONE', #13346 ) ;
#10098 = ORIENTED_EDGE ( 'NONE', *, *, #14068, .T. ) ;
#10099 = ORIENTED_EDGE ( 'NONE', *, *, #5359, .F. ) ;
#10100 = FACE_OUTER_BOUND ( 'NONE', #1647, .T. ) ;
#10101 = CARTESIAN_POINT ( 'NONE',  ( 5.021133111224576062, 14.09580098603202636, -87.50000000000000000 ) ) ;
#10102 = VECTOR ( 'NONE', #11081, 1000.000000000000114 ) ;
#10103 = CIRCLE ( 'NONE', #6694, 32.54542015209056416 ) ;
#10104 = CARTESIAN_POINT ( 'NONE',  ( -499.9999999999999432, 112.9999999999999574, -194.9999999999999716 ) ) ;
#10105 = DIRECTION ( 'NONE',  ( 0.000000000000000000, 0.000000000000000000, -1.000000000000000000 ) ) ;
#10107 = DIRECTION ( 'NONE',  ( 0.000000000000000000, -1.000000000000000000, 0.000000000000000000 ) ) ;
#10106 =( REPRESENTATION_RELATIONSHIP ('NONE','NONE', #23037, #15767 ) REPRESENTATION_RELATIONSHIP_WITH_TRANSFORMATION ( #14409 )SHAPE_REPRESENTATION_RELATIONSHIP( ) );
#10108 = ORIENTED_EDGE ( 'NONE', *, *, #5899, .F. ) ;
#10109 = CARTESIAN_POINT ( 'NONE',  ( 2.604019732385639330, 30.43784769162271076, 10.75394592869520594 ) ) ;
#10110 = CARTESIAN_POINT ( 'NONE',  ( 99.29916851150809975, 0.7568087271434508212, 12.48276086518024641 ) ) ;
#10111 = PRESENTATION_LAYER_ASSIGNMENT (  '', '', ( #20364 ) ) ;
#10112 = CARTESIAN_POINT ( 'NONE',  ( 5.021133111224265200, -15.68591377522703745, -67.50000000000000000 ) ) ;
#10113 = ORIENTED_EDGE ( 'NONE', *, *, #28366, .F. ) ;
#10114 = LINE ( 'NONE', #2106, #16664 ) ;
#10115 = ORIENTED_EDGE ( 'NONE', *, *, #18665, .T. ) ;
#10116 = CARTESIAN_POINT ( 'NONE',  ( 8.000000000000000000, 0.000000000000000000, 0.000000000000000000 ) ) ;
#10117 = EDGE_CURVE ( 'NONE', #31064, #14153, #35057, .T. ) ;
#10118 = CARTESIAN_POINT ( 'NONE',  ( 2.790000000000083080, 14.57875922523665047, 26.97523840778890047 ) ) ;
#10119 = ADVANCED_FACE ( 'NONE', ( #153 ), #26678, .T. ) ;
#10120 = VECTOR ( 'NONE', #17692, 1000.000000000000000 ) ;
#10121 = VERTEX_POINT ( 'NONE', #19912 ) ;
#10122 = CYLINDRICAL_SURFACE ( 'NONE', #5726, 3.999999999999976019 ) ;
#10123 = PLANE ( 'NONE',  #9393 ) ;
#10125 = EDGE_CURVE ( 'NONE', #14449, #25806, #689, .T. ) ;
#10124 = CARTESIAN_POINT ( 'NONE',  ( -23.93921925319781963, 29.33115633223347274, -36.68877005347593467 ) ) ;
#10126 = ORIENTED_EDGE ( 'NONE', *, *, #8259, .F. ) ;
#10127 = CIRCLE ( 'NONE', #30023, 4.750000000000004441 ) ;
#10128 = ORIENTED_EDGE ( 'NONE', *, *, #20900, .T. ) ;
#10129 = DIRECTION ( 'NONE',  ( 0.1063910735368947813, -0.9943243633099144718, -3.335902418024520312E-15 ) ) ;
#10130 = VECTOR ( 'NONE', #17265, 1000.000000000000000 ) ;
#10131 = ORIENTED_EDGE ( 'NONE', *, *, #9603, .T. ) ;
#10132 = EDGE_CURVE ( 'NONE', #30042, #527, #25858, .T. ) ;
#10133 = VECTOR ( 'NONE', #17355, 1000.000000000000114 ) ;
#10134 = LINE ( 'NONE', #12642, #32301 ) ;
#10135 = CARTESIAN_POINT ( 'NONE',  ( -5.021133111224782120, 18.16264470403145026, -67.50000000000000000 ) ) ;
#10136 = CARTESIAN_POINT ( 'NONE',  ( 99.26191511054601335, -2.804307960831458189E-14, 7.500000000000241585 ) ) ;
#10137 = CONTEXT_DEPENDENT_SHAPE_REPRESENTATION ( #14443, #1847 ) ;
#10138 = EDGE_LOOP ( 'NONE', ( #22939, #22401, #30702, #27350 ) ) ;
#10139 = DIRECTION ( 'NONE',  ( 0.000000000000000000, 0.000000000000000000, -1.000000000000000000 ) ) ;
#10140 = CIRCLE ( 'NONE', #10787, 3.999999999999948042 ) ;
#10142 = DIRECTION ( 'NONE',  ( 0.000000000000000000, 1.836970198721029441E-16, -1.000000000000000000 ) ) ;
#10141 = DIRECTION ( 'NONE',  ( 0.5611870653623822758, 0.8276889981568905652, -0.000000000000000000 ) ) ;
#10143 = AXIS2_PLACEMENT_3D ( 'NONE', #15902, #26724, #9828 ) ;
#10144 = EDGE_LOOP ( 'NONE', ( #8150, #5363, #7712, #19761 ) ) ;
#10145 = EDGE_LOOP ( 'NONE', ( #12310, #15522, #4076, #2166 ) ) ;
#10146 = DIRECTION ( 'NONE',  ( -0.6876994588534230957, -0.7259954919231310644, 0.000000000000000000 ) ) ;
#10147 = ORIENTED_EDGE ( 'NONE', *, *, #20197, .T. ) ;
#10148 = FACE_OUTER_BOUND ( 'NONE', #32442, .T. ) ;
#10149 = CARTESIAN_POINT ( 'NONE',  ( -418.0000000000000000, 104.9999999999999858, -162.9999999999999716 ) ) ;
#10150 = ORIENTED_EDGE ( 'NONE', *, *, #21782, .T. ) ;
#10151 = CIRCLE ( 'NONE', #13014, 10.00000000000000000 ) ;
#10152 = DIRECTION ( 'NONE',  ( -1.000000000000000000, -0.000000000000000000, -0.000000000000000000 ) ) ;
#10153 = PRODUCT_DEFINITION_SHAPE ( 'NONE', 'NONE',  #35217 ) ;
#10154 = ORIENTED_EDGE ( 'NONE', *, *, #3912, .T. ) ;
#10155 = PLANE ( 'NONE',  #11257 ) ;
#10156 = CARTESIAN_POINT ( 'NONE',  ( -499.9999999999999432, 104.9999999999999858, 162.9999999999999716 ) ) ;
#10157 = EDGE_CURVE ( 'NONE', #3997, #23842, #32882, .T. ) ;
#10158 = DIRECTION ( 'NONE',  ( 0.000000000000000000, 0.000000000000000000, -1.000000000000000000 ) ) ;
#10159 = AXIS2_PLACEMENT_3D ( 'NONE', #7245, #12277, #31291 ) ;
#10161 = CARTESIAN_POINT ( 'NONE',  ( 2.765921099433443775, -26.45933846664182099, -16.32596387352474565 ) ) ;
#10160 = DIRECTION ( 'NONE',  ( -0.000000000000000000, 1.836970198721029688E-16, -1.000000000000000000 ) ) ;
#10162 = LINE ( 'NONE', #34019, #25812 ) ;
#10163 = DIRECTION ( 'NONE',  ( -0.000000000000000000, 1.836970198721029934E-16, -1.000000000000000000 ) ) ;
#10164 = DIRECTION ( 'NONE',  ( 0.000000000000000000, 0.8958117331950893325, -0.4444337280967883275 ) ) ;
#10166 = ADVANCED_FACE ( 'NONE', ( #8684 ), #6540, .F. ) ;
#10165 = DIRECTION ( 'NONE',  ( -1.000000000000000000, -0.000000000000000000, -0.000000000000000000 ) ) ;
#10167 = EDGE_CURVE ( 'NONE', #9463, #16548, #22666, .T. ) ;
#10168 = VECTOR ( 'NONE', #9187, 1000.000000000000000 ) ;
#10169 = ORIENTED_EDGE ( 'NONE', *, *, #25348, .F. ) ;
#10170 = EDGE_CURVE ( 'NONE', #17629, #18432, #3169, .T. ) ;
#10171 = ADVANCED_FACE ( 'NONE', ( #28265 ), #14221, .F. ) ;
#10173 = VERTEX_POINT ( 'NONE', #30222 ) ;
#10172 = MANIFOLD_SOLID_BREP ( 'Boss-Extrude4[2]', #8657 ) ;
#10174 = ORIENTED_EDGE ( 'NONE', *, *, #2834, .T. ) ;
#10175 = EDGE_CURVE ( 'NONE', #25102, #23404, #20408, .T. ) ;
#10176 = PRESENTATION_LAYER_ASSIGNMENT (  '', '', ( #9037 ) ) ;
#10177 = DIRECTION ( 'NONE',  ( -1.000000000000000000, -0.000000000000000000, -0.000000000000000000 ) ) ;
#10178 = DIRECTION ( 'NONE',  ( 0.8867788707476064181, 0.4621939359139195513, 1.641173741546747897E-14 ) ) ;
#10179 = VERTEX_POINT ( 'NONE', #25227 ) ;
#10180 = ORIENTED_EDGE ( 'NONE', *, *, #15929, .T. ) ;
#10181 = EDGE_LOOP ( 'NONE', ( #13138, #25064, #16918, #21728 ) ) ;
#10182 = DIRECTION ( 'NONE',  ( -1.000000000000000000, 0.000000000000000000, 0.000000000000000000 ) ) ;
#10183 = PLANE ( 'NONE',  #17039 ) ;
#10184 = VECTOR ( 'NONE', #10942, 1000.000000000000000 ) ;
#10185 = ITEM_DEFINED_TRANSFORMATION ( 'NONE', 'NONE', #5321,  #28566 ) ;
#10186 = VERTEX_POINT ( 'NONE', #863 ) ;
#10187 = DIRECTION ( 'NONE',  ( 1.000000000000000000, 0.000000000000000000, 0.000000000000000000 ) ) ;
#10188 = CARTESIAN_POINT ( 'NONE',  ( 0.000000000000000000, 28.95078156989571738, -9.502838467757779739 ) ) ;
#10189 = EDGE_LOOP ( 'NONE', ( #19227, #6936, #33110, #4210, #24558 ) ) ;
#10190 = EDGE_LOOP ( 'NONE', ( #18358, #7019, #30378, #14147 ) ) ;
#10191 = CARTESIAN_POINT ( 'NONE',  ( -6.500000000000000000, 0.000000000000000000, 5.429999999999999716 ) ) ;
#10192 = DIRECTION ( 'NONE',  ( -0.000000000000000000, 1.000000000000000000, 0.000000000000000000 ) ) ;
#10193 = CARTESIAN_POINT ( 'NONE',  ( -20.63749999999999929, 0.000000000000000000, -9.999999999999996447 ) ) ;
#10194 = CARTESIAN_POINT ( 'NONE',  ( 25.76952721012208514, 19.87802405277947315, 68.31122994652405112 ) ) ;
#10195 = CARTESIAN_POINT ( 'NONE',  ( 42.44043929807611448, -17.65143121711728469, 20.00000000000000000 ) ) ;
#10196 = ORIENTED_EDGE ( 'NONE', *, *, #29369, .F. ) ;
#10197 = LINE ( 'NONE', #26386, #18058 ) ;
#10198 = CARTESIAN_POINT ( 'NONE',  ( -5.614556921127968003, -37.45022281665697506, -36.68877005347593467 ) ) ;
#10199 = AXIS2_PLACEMENT_3D ( 'NONE', #22502, #3959, #17358 ) ;
#10200 = LINE ( 'NONE', #29765, #27585 ) ;
#10201 = FACE_OUTER_BOUND ( 'NONE', #17098, .T. ) ;
#10202 = CARTESIAN_POINT ( 'NONE',  ( -45.05956070192387841, -32.65143121711728469, 0.000000000000000000 ) ) ;
#10204 = DIRECTION ( 'NONE',  ( -1.000000000000000000, -0.000000000000000000, -0.000000000000000000 ) ) ;
#10203 = LINE ( 'NONE', #15552, #29807 ) ;
#10205 = VECTOR ( 'NONE', #13391, 1000.000000000000000 ) ;
#10206 = FACE_OUTER_BOUND ( 'NONE', #19535, .T. ) ;
#10207 = ORIENTED_EDGE ( 'NONE', *, *, #29532, .F. ) ;
#10208 = CARTESIAN_POINT ( 'NONE',  ( 107.8898084714338523, 4.971174042719110453, -11.47116230092015066 ) ) ;
#10210 = DIRECTION ( 'NONE',  ( -0.000000000000000000, -0.000000000000000000, -1.000000000000000000 ) ) ;
#10209 = DIRECTION ( 'NONE',  ( -1.000000000000000000, 6.792721752314501023E-48, -3.697785493223492838E-32 ) ) ;
#10211 = VECTOR ( 'NONE', #31792, 1000.000000000000000 ) ;
#10212 = ORIENTED_EDGE ( 'NONE', *, *, #26086, .T. ) ;
#10213 = EDGE_CURVE ( 'NONE', #6336, #24518, #5031, .T. ) ;
#10214 = EDGE_CURVE ( 'NONE', #1917, #6409, #512, .T. ) ;
#10215 = DIRECTION ( 'NONE',  ( -0.000000000000000000, -0.000000000000000000, -1.000000000000000000 ) ) ;
#10216 = VERTEX_POINT ( 'NONE', #6358 ) ;
#10217 = VECTOR ( 'NONE', #1960, 1000.000000000000000 ) ;
#10218 = VERTEX_POINT ( 'NONE', #30754 ) ;
#10219 = CARTESIAN_POINT ( 'NONE',  ( 2.783128948903274669, -29.45617853245872553, 9.233693611949725266 ) ) ;
#10220 = VERTEX_POINT ( 'NONE', #25406 ) ;
#10221 = ORIENTED_EDGE ( 'NONE', *, *, #13190, .T. ) ;
#10222 = DIRECTION ( 'NONE',  ( 0.000000000000000000, -2.465190328815661892E-32, -1.000000000000000000 ) ) ;
#10223 = ADVANCED_FACE ( 'NONE', ( #1036 ), #20436, .F. ) ;
#10224 = CARTESIAN_POINT ( 'NONE',  ( -21.41424479178920492, -24.50784553716282232, 68.31122994652405112 ) ) ;
#10225 = PLANE ( 'NONE',  #32448 ) ;
#10226 = EDGE_LOOP ( 'NONE', ( #6029, #13381, #14983, #8399 ) ) ;
#10227 = ORIENTED_EDGE ( 'NONE', *, *, #24124, .T. ) ;
#10228 = CARTESIAN_POINT ( 'NONE',  ( -9.978866888775527855, 6.201984591278720593, -87.50000000000000000 ) ) ;
#10229 = CARTESIAN_POINT ( 'NONE',  ( 2.789999999999999147, 0.000000000000000000, 0.000000000000000000 ) ) ;
#10230 = DIRECTION ( 'NONE',  ( 1.000000000000000000, 0.000000000000000000, -0.000000000000000000 ) ) ;
#10231 = ADVANCED_FACE ( 'NONE', ( #12781 ), #31796, .T. ) ;
#10232 = DIRECTION ( 'NONE',  ( 0.000000000000000000, -0.5288966977476834419, -0.8486862100397269959 ) ) ;
#10233 = DIRECTION ( 'NONE',  ( 1.000000000000000000, -0.000000000000000000, -0.000000000000000000 ) ) ;
#10234 = UNCERTAINTY_MEASURE_WITH_UNIT (LENGTH_MEASURE( 1.000000000000000082E-05 ), #3448, 'distance_accuracy_value', 'NONE');
#10235 = ORIENTED_EDGE ( 'NONE', *, *, #33095, .T. ) ;
#10236 = VECTOR ( 'NONE', #16379, 1000.000000000000000 ) ;
#10237 = ADVANCED_FACE ( 'NONE', ( #1387 ), #19854, .T. ) ;
#10238 = ADVANCED_FACE ( 'NONE', ( #12259 ), #17773, .F. ) ;
#10239 = DIRECTION ( 'NONE',  ( -1.000000000000000000, -0.000000000000000000, -0.000000000000000000 ) ) ;
#10240 = ORIENTED_EDGE ( 'NONE', *, *, #10487, .F. ) ;
#10241 = DIRECTION ( 'NONE',  ( 1.000000000000000000, -0.000000000000000000, -0.000000000000000000 ) ) ;
#10242 = ADVANCED_FACE ( 'NONE', ( #17609, #23110 ), #33954, .F. ) ;
#10243 = PLANE ( 'NONE',  #34231 ) ;
#10244 = DIRECTION ( 'NONE',  ( 0.000000000000000000, 1.836970198721029441E-16, -1.000000000000000000 ) ) ;
#10245 = VERTEX_POINT ( 'NONE', #7230 ) ;
#10246 = CARTESIAN_POINT ( 'NONE',  ( 129.3530333899765594, 6.000000000000000000, -62.49999999999999289 ) ) ;
#10247 = ORIENTED_EDGE ( 'NONE', *, *, #7251, .F. ) ;
#10248 = CARTESIAN_POINT ( 'NONE',  ( -35.00000000000000000, -12.29554237047778287, 20.46290632209285576 ) ) ;
#10249 = ORIENTED_EDGE ( 'NONE', *, *, #6405, .T. ) ;
#10251 = DIRECTION ( 'NONE',  ( 0.000000000000000000, -1.000000000000000000, -2.132064625830773463E-16 ) ) ;
#10250 = DIRECTION ( 'NONE',  ( 0.000000000000000000, -1.000000000000000000, 0.000000000000000000 ) ) ;
#10252 = ORIENTED_EDGE ( 'NONE', *, *, #15815, .T. ) ;
#10253 = EDGE_CURVE ( 'NONE', #31150, #26496, #9576, .T. ) ;
#10254 = CARTESIAN_POINT ( 'NONE',  ( -430.0000000000000000, 118.9999999999999716, 130.0000000000000000 ) ) ;
#10255 = DIRECTION ( 'NONE',  ( 0.8276889981568904542, 0.5611870653623824978, -0.000000000000000000 ) ) ;
#10256 = ORIENTED_EDGE ( 'NONE', *, *, #3516, .T. ) ;
#10257 = VECTOR ( 'NONE', #15978, 1000.000000000000000 ) ;
#10258 = DIRECTION ( 'NONE',  ( -7.893605728314051750E-14, 1.618803117314786530E-15, 1.000000000000000000 ) ) ;
#10259 = VERTEX_POINT ( 'NONE', #15446 ) ;
#10260 = CARTESIAN_POINT ( 'NONE',  ( -410.0000000000000568, 113.0000000000000000, 154.9999999999999716 ) ) ;
#10261 = ORIENTED_EDGE ( 'NONE', *, *, #24371, .F. ) ;
#10262 = DIRECTION ( 'NONE',  ( 1.000000000000000000, -0.000000000000000000, -0.000000000000000000 ) ) ;
#10263 = CARTESIAN_POINT ( 'NONE',  ( 3.235562306570555532E-30, 18.16264470403145026, -67.50000000000000000 ) ) ;
#10264 = DIRECTION ( 'NONE',  ( -1.000000000000000000, 0.000000000000000000, 0.000000000000000000 ) ) ;
#10265 = VECTOR ( 'NONE', #22408, 1000.000000000000114 ) ;
#10266 = DIRECTION ( 'NONE',  ( -1.000000000000000000, 0.000000000000000000, 0.000000000000000000 ) ) ;
#10267 = EDGE_LOOP ( 'NONE', ( #33817, #23943, #14335, #24138, #13010, #17686 ) ) ;
#10268 = VERTEX_POINT ( 'NONE', #10092 ) ;
#10269 = VECTOR ( 'NONE', #18458, 1000.000000000000000 ) ;
#10270 = ORIENTED_EDGE ( 'NONE', *, *, #13618, .F. ) ;
#10271 = DIRECTION ( 'NONE',  ( -1.000000000000000000, 0.000000000000000000, 0.000000000000000000 ) ) ;
#10272 = EDGE_CURVE ( 'NONE', #18752, #27262, #24923, .T. ) ;
#10273 = B_SPLINE_CURVE_WITH_KNOTS ( 'NONE', 3,
 ( #9435, #31146, #25077, #28300, #896, #22780, #17104, #3894, #22612, #33454, #33629, #9251, #6570, #33096, #11937, #9074, #11582, #27937, #25261, #6035, #715, #4063, #11763, #6389, #20119, #28116, #16932, #14435, #25439, #3729, #6745, #30965, #17287, #25791, #25612, #19769, #19940, #30788, #3375, #17470 ),
 .UNSPECIFIED., .F., .F.,
 ( 4, 2, 2, 2, 2, 2, 2, 2, 2, 2, 2, 2, 2, 2, 2, 2, 2, 2, 2, 4 ),
 ( 0.01617148595533309322, 0.01667647242675793923, 0.01718145889818278524, 0.01819143184103248073, 0.01869641831245732674, 0.01920140478388217276, 0.02021137772673184396, 0.02122135066958151517, 0.02223132361243118638, 0.02324129655528085758, 0.02425126949813052879, 0.02526124244098020000, 0.02627121538382987120, 0.02728118832667954241, 0.02829116126952921362, 0.02879614774095406310, 0.02930113421237891258, 0.03031110715522861154, 0.03132108009807831051, 0.03233105304092800947 ),
 .UNSPECIFIED. ) ;
#10274 = CARTESIAN_POINT ( 'NONE',  ( 2.765921099433441999, 7.350529080603541487, 30.20932655202940254 ) ) ;
#10275 = EDGE_CURVE ( 'NONE', #11988, #11647, #28613, .T. ) ;
#10276 = EDGE_CURVE ( 'NONE', #29324, #19338, #1070, .T. ) ;
#10277 = CARTESIAN_POINT ( 'NONE',  ( -430.0000000000000000, -119.0000000000000000, 126.0000000000000000 ) ) ;
#10278 = CARTESIAN_POINT ( 'NONE',  ( -418.0000000000000000, 124.9999999999999574, -194.9999999999999716 ) ) ;
#10279 = DIRECTION ( 'NONE',  ( 1.000000000000000000, 0.000000000000000000, 5.546364386991661285E-52 ) ) ;
#10280 = VERTEX_POINT ( 'NONE', #20951 ) ;
#10281 = CIRCLE ( 'NONE', #27318, 2.525000000000001243 ) ;
#10282 = FACE_OUTER_BOUND ( 'NONE', #30498, .T. ) ;
#10283 = CARTESIAN_POINT ( 'NONE',  ( 1.749999999999999778, 0.000000000000000000, 0.000000000000000000 ) ) ;
#10284 = CIRCLE ( 'NONE', #23367, 4.000000000000003553 ) ;
#10285 = DIRECTION ( 'NONE',  ( -0.000000000000000000, -0.000000000000000000, -1.000000000000000000 ) ) ;
#10286 = EDGE_LOOP ( 'NONE', ( #12652, #21109, #13555, #534 ) ) ;
#10287 = CARTESIAN_POINT ( 'NONE',  ( 2.789999999999999147, 30.40449935640660684, -2.004522720844263084 ) ) ;
#10288 = ORIENTED_EDGE ( 'NONE', *, *, #29502, .T. ) ;
#10289 = DIRECTION ( 'NONE',  ( 0.000000000000000000, -1.000000000000000000, -1.836970198721029934E-16 ) ) ;
#10290 = FACE_OUTER_BOUND ( 'NONE', #6928, .T. ) ;
#10292 = ORIENTED_EDGE ( 'NONE', *, *, #14063, .T. ) ;
#10291 = AXIS2_PLACEMENT_3D ( 'NONE', #12003, #1484, #4309 ) ;
#10293 = CARTESIAN_POINT ( 'NONE',  ( 0.000000000000000000, 0.000000000000000000, 20.00000000000000000 ) ) ;
#10294 = VECTOR ( 'NONE', #2406, 1000.000000000000000 ) ;
#10295 = CARTESIAN_POINT ( 'NONE',  ( -410.0000000000000568, 105.0000000000000142, -175.0000000000000000 ) ) ;
#10296 = CARTESIAN_POINT ( 'NONE',  ( -3.250000000000000000, 5.404196845913421754, -0.7500000000000000000 ) ) ;
#10297 = ORIENTED_EDGE ( 'NONE', *, *, #13498, .T. ) ;
#10298 = ORIENTED_EDGE ( 'NONE', *, *, #34751, .F. ) ;
#10299 = DIRECTION ( 'NONE',  ( -7.893605728314050488E-14, 1.618803117314786135E-15, 0.9999999999999998890 ) ) ;
#10301 = EDGE_CURVE ( 'NONE', #30602, #18391, #27779, .T. ) ;
#10300 = VECTOR ( 'NONE', #4310, 1000.000000000000000 ) ;
#10302 = VERTEX_POINT ( 'NONE', #25943 ) ;
#10303 = FACE_OUTER_BOUND ( 'NONE', #4300, .T. ) ;
#10304 = VECTOR ( 'NONE', #11738, 1000.000000000000000 ) ;
#10305 = SURFACE_STYLE_USAGE ( .BOTH. , #34692 ) ;
#10306 = DIRECTION ( 'NONE',  ( 0.000000000000000000, 0.000000000000000000, -1.000000000000000000 ) ) ;
#10307 = FACE_BOUND ( 'NONE', #7110, .T. ) ;
#10308 = CONTEXT_DEPENDENT_SHAPE_REPRESENTATION ( #8966, #23448 ) ;
#10309 = APPLICATION_CONTEXT ( 'automotive_design' ) ;
#10310 = ORIENTED_EDGE ( 'NONE', *, *, #681, .T. ) ;
#10311 = LINE ( 'NONE', #7450, #20385 ) ;
#10312 = EDGE_CURVE ( 'NONE', #4500, #27567, #28903, .T. ) ;
#10313 = EDGE_CURVE ( 'NONE', #11417, #32678, #33780, .T. ) ;
#10314 = EDGE_CURVE ( 'NONE', #18883, #31191, #9742, .T. ) ;
#10316 = CARTESIAN_POINT ( 'NONE',  ( -499.9999999999999432, 108.9999999999999858, 162.9999999999999716 ) ) ;
#10315 = PLANE ( 'NONE',  #26979 ) ;
#10318 = VERTEX_POINT ( 'NONE', #29130 ) ;
#10317 = VECTOR ( 'NONE', #10511, 1000.000000000000000 ) ;
#10319 = VERTEX_POINT ( 'NONE', #14756 ) ;
#10320 = CARTESIAN_POINT ( 'NONE',  ( -145.0000000000000568, -12.50000000000001066, 1.224646799147353217E-14 ) ) ;
#10321 = ORIENTED_EDGE ( 'NONE', *, *, #18290, .F. ) ;
#10322 = AXIS2_PLACEMENT_3D ( 'NONE', #5075, #32661, #2243 ) ;
#10323 = EDGE_CURVE ( 'NONE', #14417, #7139, #10151, .T. ) ;
#10324 = MECHANICAL_DESIGN_GEOMETRIC_PRESENTATION_REPRESENTATION (  '', ( #33623 ), #10885 ) ;
#10325 = DIRECTION ( 'NONE',  ( 0.000000000000000000, 0.000000000000000000, 1.000000000000000000 ) ) ;
#10326 = LINE ( 'NONE', #24194, #22242 ) ;
#10327 = ORIENTED_EDGE ( 'NONE', *, *, #22490, .F. ) ;
#10328 = DIRECTION ( 'NONE',  ( -0.000000000000000000, 0.000000000000000000, 1.000000000000000000 ) ) ;
#10329 = LINE ( 'NONE', #21546, #25714 ) ;
#10330 = VERTEX_POINT ( 'NONE', #22925 ) ;
#10331 = PLANE ( 'NONE',  #28822 ) ;
#10332 =( NAMED_UNIT ( * ) PLANE_ANGLE_UNIT ( ) SI_UNIT ( $, .RADIAN. ) );
#10333 = CARTESIAN_POINT ( 'NONE',  ( -442.0000000000000000, -104.9999999999999858, -194.9999999999999716 ) ) ;
#10335 = LINE ( 'NONE', #13371, #23067 ) ;
#10334 = PLANE ( 'NONE',  #4811 ) ;
#10336 = DIRECTION ( 'NONE',  ( -0.1081190184239433083, 0.9941379571543594862, 1.826201800709962632E-16 ) ) ;
#10337 = DIRECTION ( 'NONE',  ( -1.997825486195707906E-17, 0.000000000000000000, 1.000000000000000000 ) ) ;
#10338 = CARTESIAN_POINT ( 'NONE',  ( -12.00000000000001066, -145.0000000000000000, 187.0000000000000000 ) ) ;
#10339 = AXIS2_PLACEMENT_3D ( 'NONE', #20806, #15838, #21342 ) ;
#10340 = VERTEX_POINT ( 'NONE', #28438 ) ;
#10341 = VECTOR ( 'NONE', #9063, 1000.000000000000000 ) ;
#10342 = VECTOR ( 'NONE', #19330, 999.9999999999998863 ) ;
#10343 = AXIS2_PLACEMENT_3D ( 'NONE', #14951, #9602, #1750 ) ;
#10345 = ORIENTED_EDGE ( 'NONE', *, *, #18471, .F. ) ;
#10344 = MANIFOLD_SOLID_BREP ( 'Square tube 20 X 20 X 2(1)[4]', #22482 ) ;
#10346 = ORIENTED_EDGE ( 'NONE', *, *, #26150, .F. ) ;
#10347 = CARTESIAN_POINT ( 'NONE',  ( -12.00000000000001066, -112.9999999999999858, 155.0000000000000000 ) ) ;
#10348 = EDGE_CURVE ( 'NONE', #5234, #13672, #4031, .T. ) ;
#10349 = ORIENTED_EDGE ( 'NONE', *, *, #17479, .F. ) ;
#10350 = ORIENTED_EDGE ( 'NONE', *, *, #30883, .T. ) ;
#10351 = LINE ( 'NONE', #7853, #21315 ) ;
#10352 = CARTESIAN_POINT ( 'NONE',  ( 2.719051665953501562, 21.26181984063893893, 23.50417665062026273 ) ) ;
#10353 = ADVANCED_FACE ( 'NONE', ( #29662 ), #3891, .T. ) ;
#10354 = CONTEXT_DEPENDENT_SHAPE_REPRESENTATION ( #12876, #2487 ) ;
#10355 = DIRECTION ( 'NONE',  ( 0.9476531711828023452, -0.3193015301359802827, -5.865473952658207447E-17 ) ) ;
#10356 = CARTESIAN_POINT ( 'NONE',  ( -19.99999999999998934, 136.9999999999999716, 155.0000000000000000 ) ) ;
#10357 = ORIENTED_EDGE ( 'NONE', *, *, #4592, .F. ) ;
#10358 = EDGE_LOOP ( 'NONE', ( #28928, #26404, #12720, #20054 ) ) ;
#10359 =( REPRESENTATION_RELATIONSHIP ('NONE','NONE', #23037, #28231 ) REPRESENTATION_RELATIONSHIP_WITH_TRANSFORMATION ( #19264 )SHAPE_REPRESENTATION_RELATIONSHIP( ) );
#10360 = DIRECTION ( 'NONE',  ( -1.000000000000000000, 0.000000000000000000, 0.000000000000000000 ) ) ;
#10361 = CLOSED_SHELL ( 'NONE', ( #9446, #376, #3253, #15406, #24092, #18099, #58, #30733, #3038, #16366, #13200, #31367, #21586, #2156, #6326, #8851, #15656, #15369, #16651, #9810, #31269, #10237, #1255, #7652, #4622, #4239, #3852, #27622, #12640, #13749, #16504, #14399, #28170, #22336, #20493, #4721, #17402, #16411 ) ) ;
#10362 = LINE ( 'NONE', #32066, #21524 ) ;
#10363 = EDGE_CURVE ( 'NONE', #14361, #108, #6197, .T. ) ;
#10364 = PLANE ( 'NONE',  #5627 ) ;
#10365 = CARTESIAN_POINT ( 'NONE',  ( 2.789999999999999147, -29.00730259674831757, -9.328884633909261481 ) ) ;
#10366 = DIRECTION ( 'NONE',  ( -0.000000000000000000, -1.000000000000000000, -0.000000000000000000 ) ) ;
#10367 = ORIENTED_EDGE ( 'NONE', *, *, #2037, .T. ) ;
#10368 = CARTESIAN_POINT ( 'NONE',  ( 1.999999999999999556, 0.000000000000000000, -0.7500000000000000000 ) ) ;
#10369 = DIRECTION ( 'NONE',  ( -1.000000000000000000, -0.000000000000000000, -0.000000000000000000 ) ) ;
#10370 = VECTOR ( 'NONE', #5413, 1000.000000000000000 ) ;
#10371 = EDGE_CURVE ( 'NONE', #32902, #33119, #33029, .T. ) ;
#10372 = AXIS2_PLACEMENT_3D ( 'NONE', #5940, #32647, #10607 ) ;
#10373 = DIRECTION ( 'NONE',  ( -0.7621620551276367950, -0.6473862847818272481, 0.000000000000000000 ) ) ;
#10374 = DIRECTION ( 'NONE',  ( 0.000000000000000000, 0.000000000000000000, 1.000000000000000000 ) ) ;
#10375 = EDGE_CURVE ( 'NONE', #15121, #8787, #21124, .T. ) ;
#10376 = EDGE_CURVE ( 'NONE', #10121, #10892, #5088, .T. ) ;
#10377 = CARTESIAN_POINT ( 'NONE',  ( 109.2888833233461980, 3.828784459365716319, -6.456053091683092049 ) ) ;
#10379 = CARTESIAN_POINT ( 'NONE',  ( 55.00000000000000711, 0.000000000000000000, 0.000000000000000000 ) ) ;
#10378 = CARTESIAN_POINT ( 'NONE',  ( 2.789999999999999147, 31.93991905851385837, 0.000000000000000000 ) ) ;
#10380 = CARTESIAN_POINT ( 'NONE',  ( -20.00000000000007461, 136.9999999999999432, -187.0000000000000000 ) ) ;
#10381 = EDGE_LOOP ( 'NONE', ( #20423, #24808, #15057, #30265 ) ) ;
#10382 = CARTESIAN_POINT ( 'NONE',  ( 0.000000000000000000, 0.000000000000000000, 3.180000000000000160 ) ) ;
#10384 = DIRECTION ( 'NONE',  ( 1.300283923313630633E-47, 0.000000000000000000, 1.000000000000000000 ) ) ;
#10383 = DIRECTION ( 'NONE',  ( 0.000000000000000000, 0.000000000000000000, 1.000000000000000000 ) ) ;
#10385 = ORIENTED_EDGE ( 'NONE', *, *, #29287, .F. ) ;
#10386 =( NAMED_UNIT ( * ) SI_UNIT ( $, .STERADIAN. ) SOLID_ANGLE_UNIT ( ) );
#10387 = ORIENTED_EDGE ( 'NONE', *, *, #31227, .F. ) ;
#10388 = B_SPLINE_CURVE_WITH_KNOTS ( 'NONE', 3,
 ( #11160, #32849, #27687, #24471, #5783, #27330 ),
 .UNSPECIFIED., .F., .F.,
 ( 4, 2, 4 ),
 ( 2.248981763129426848E-07, 0.001873423219693743378, 0.003746621541211173859 ),
 .UNSPECIFIED. ) ;
#10389 = AXIS2_PLACEMENT_3D ( 'NONE', #19082, #24388, #4814 ) ;
#10390 = AXIS2_PLACEMENT_3D ( 'NONE', #27579, #24540, #8363 ) ;
#10391 = CIRCLE ( 'NONE', #25173, 32.54542015209057126 ) ;
#10392 = AXIS2_PLACEMENT_3D ( 'NONE', #8800, #19676, #22696 ) ;
#10393 = ORIENTED_EDGE ( 'NONE', *, *, #557, .F. ) ;
#10394 = CARTESIAN_POINT ( 'NONE',  ( 2.765921099435497243, 28.29688452313399338, 12.88099432405614309 ) ) ;
#10395 = VERTEX_POINT ( 'NONE', #16330 ) ;
#10396 = ORIENTED_EDGE ( 'NONE', *, *, #7358, .T. ) ;
#10397 = DIRECTION ( 'NONE',  ( 1.000000000000000000, 0.000000000000000000, 0.000000000000000000 ) ) ;
#10398 = DIRECTION ( 'NONE',  ( 3.697785493223492838E-32, 1.934419779023891545E-16, -1.000000000000000000 ) ) ;
#10399 = DIRECTION ( 'NONE',  ( 0.000000000000000000, -1.000000000000000000, -1.224646799147353207E-16 ) ) ;
#10400 = VERTEX_POINT ( 'NONE', #27158 ) ;
#10401 = ORIENTED_EDGE ( 'NONE', *, *, #9917, .F. ) ;
#10402 = CARTESIAN_POINT ( 'NONE',  ( 0.1835379100341435199, -28.84240889917319706, -14.47562221546578343 ) ) ;
#10403 = CARTESIAN_POINT ( 'NONE',  ( -418.0000000000000000, -105.0000000000000142, 187.0000000000000000 ) ) ;
#10404 = DIRECTION ( 'NONE',  ( 1.000000000000000000, 0.000000000000000000, 0.000000000000000000 ) ) ;
#10405 = EDGE_CURVE ( 'NONE', #25011, #5512, #8473, .T. ) ;
#10406 = CARTESIAN_POINT ( 'NONE',  ( 35.63428259149704758, -12.79065496477508823, 68.31122994652405112 ) ) ;
#10407 = CARTESIAN_POINT ( 'NONE',  ( 55.00000000000000711, 0.000000000000000000, 0.000000000000000000 ) ) ;
#10408 = ORIENTED_EDGE ( 'NONE', *, *, #7754, .F. ) ;
#10409 = CARTESIAN_POINT ( 'NONE',  ( 2.789999999999999147, -14.75935258146429341, 26.65732927035513811 ) ) ;
#10410 = MECHANICAL_DESIGN_GEOMETRIC_PRESENTATION_REPRESENTATION (  '', ( #34291 ), #14976 ) ;
#10411 = EDGE_CURVE ( 'NONE', #8166, #3093, #24470, .T. ) ;
#10412 = EDGE_CURVE ( 'NONE', #31468, #5130, #10546, .T. ) ;
#10413 = LINE ( 'NONE', #27298, #14755 ) ;
#10414 = ORIENTED_EDGE ( 'NONE', *, *, #26467, .F. ) ;
#10415 = CARTESIAN_POINT ( 'NONE',  ( 5.021133111224473033, 4.168562732279004202, -67.50000000000000000 ) ) ;
#10416 = DIRECTION ( 'NONE',  ( -1.000000000000000000, 0.000000000000000000, 0.000000000000000000 ) ) ;
#10417 = DIRECTION ( 'NONE',  ( 0.000000000000000000, -0.000000000000000000, 1.000000000000000000 ) ) ;
#10418 = ORIENTED_EDGE ( 'NONE', *, *, #4623, .F. ) ;
#10419 = AXIS2_PLACEMENT_3D ( 'NONE', #24693, #16716, #14035 ) ;
#10420 = DIRECTION ( 'NONE',  ( -1.000000000000000000, -0.000000000000000000, -0.000000000000000000 ) ) ;
#10421 = ORIENTED_EDGE ( 'NONE', *, *, #12637, .F. ) ;
#10422 = CIRCLE ( 'NONE', #14986, 3.999999999999989786 ) ;
#10423 = AXIS2_PLACEMENT_3D ( 'NONE', #10740, #18927, #24414 ) ;
#10424 = CARTESIAN_POINT ( 'NONE',  ( -7.654999999999999361, 1.414467053015192657E-16, 0.000000000000000000 ) ) ;
#10425 = ORIENTED_EDGE ( 'NONE', *, *, #21600, .T. ) ;
#10427 = PLANE ( 'NONE',  #26500 ) ;
#10426 = CARTESIAN_POINT ( 'NONE',  ( -1.250599194761023927E-17, -3.625355760179439280, -30.44651458975035396 ) ) ;
#10428 = CARTESIAN_POINT ( 'NONE',  ( -19.99999999999998934, -137.0000000000000000, 155.0000000000000000 ) ) ;
#10429 = EDGE_CURVE ( 'NONE', #995, #32238, #8295, .T. ) ;
#10430 = VERTEX_POINT ( 'NONE', #19175 ) ;
#10431 = DIRECTION ( 'NONE',  ( 0.000000000000000000, 0.000000000000000000, -1.000000000000000000 ) ) ;
#10432 = DIRECTION ( 'NONE',  ( 0.000000000000000000, -0.000000000000000000, 1.000000000000000000 ) ) ;
#10433 = B_SPLINE_CURVE_WITH_KNOTS ( 'NONE', 3,
 ( #23957, #32321, #15809, #12956, #5089, #15976, #26639, #4731, #7580, #7942, #13469, #12782, #2252, #23626, #15627, #34838, #5258, #31626, #7762, #10094, #10629, #18818, #34657, #10448, #2422, #18481, #13122, #2600, #13305, #32154, #18649, #29495, #29663, #26813, #16151, #24134, #35016, #21481, #4910, #26994, #24307, #9920, #20780, #7232 ),
 .UNSPECIFIED., .F., .F.,
 ( 4, 2, 2, 2, 2, 2, 2, 2, 2, 2, 2, 2, 2, 2, 2, 2, 2, 2, 2, 2, 2, 4 ),
 ( 0.01657113979051930489, 0.01708818281900469430, 0.01760522584749008371, 0.01863931190446085212, 0.01915635493294623806, 0.01967339796143162400, 0.02070748401840239589, 0.02174157007537316777, 0.02277565613234393965, 0.02380974218931471154, 0.02484382824628548342, 0.02536087127477085201, 0.02587791430325621367, 0.02691200036022690575, 0.02794608641719759437, 0.02898017247416828646, 0.02949721550265361689, 0.03001425853113894732, 0.03104834458810958736, 0.03156538761659492126, 0.03208243064508024822, 0.03311651670205089520 ),
 .UNSPECIFIED. ) ;
#10434 = EDGE_CURVE ( 'NONE', #2726, #4948, #21304, .T. ) ;
#10435 = ORIENTED_EDGE ( 'NONE', *, *, #7336, .T. ) ;
#10436 = EDGE_CURVE ( 'NONE', #8062, #14584, #12955, .T. ) ;
#10437 = AXIS2_PLACEMENT_3D ( 'NONE', #6176, #10091, #33952 ) ;
#10438 = EDGE_CURVE ( 'NONE', #10763, #24914, #14750, .T. ) ;
#10439 = DIRECTION ( 'NONE',  ( -7.893605728314051750E-14, 1.618803117314786530E-15, 1.000000000000000000 ) ) ;
#10440 = ORIENTED_EDGE ( 'NONE', *, *, #20627, .T. ) ;
#10441 = DIRECTION ( 'NONE',  ( -0.6051742151937650194, 0.7960930657056437543, 0.000000000000000000 ) ) ;
#10442 = ORIENTED_EDGE ( 'NONE', *, *, #2763, .T. ) ;
#10443 = FACE_OUTER_BOUND ( 'NONE', #22886, .T. ) ;
#10444 = EDGE_CURVE ( 'NONE', #15156, #2086, #15975, .T. ) ;
#10445 = AXIS2_PLACEMENT_3D ( 'NONE', #18129, #10439, #7572 ) ;
#10446 = DIRECTION ( 'NONE',  ( -0.000000000000000000, 1.000000000000000000, -0.000000000000000000 ) ) ;
#10447 = AXIS2_PLACEMENT_3D ( 'NONE', #1668, #31901, #34770 ) ;
#10448 = CARTESIAN_POINT ( 'NONE',  ( -105.6966460872811524, -5.070312235224274211, -5.526528498279826174 ) ) ;
#10449 = DIRECTION ( 'NONE',  ( -1.000000000000000000, -0.000000000000000000, -0.000000000000000000 ) ) ;
#10450 = ORIENTED_EDGE ( 'NONE', *, *, #34381, .T. ) ;
#10451 = ORIENTED_EDGE ( 'NONE', *, *, #2612, .T. ) ;
#10452 = CIRCLE ( 'NONE', #34899, 15.69999999999999929 ) ;
#10453 = PRODUCT_DEFINITION_SHAPE ( 'NONE', 'NONE',  #35237 ) ;
#10454 = ORIENTED_EDGE ( 'NONE', *, *, #30479, .T. ) ;
#10455 = LINE ( 'NONE', #2781, #17409 ) ;
#10456 = B_SPLINE_CURVE_WITH_KNOTS ( 'NONE', 3,
 ( #17890, #30003, #21807, #10960, #8107, #16492 ),
 .UNSPECIFIED., .F., .F.,
 ( 4, 2, 4 ),
 ( 4.404817080687146341E-07, 0.001874269664496245377, 0.003748098847284421931 ),
 .UNSPECIFIED. ) ;
#10457 = LINE ( 'NONE', #21826, #439 ) ;
#10458 = DIRECTION ( 'NONE',  ( 0.8854131517428555087, -0.2458337514780907784, -0.3944734685057935675 ) ) ;
#10459 = CARTESIAN_POINT ( 'NONE',  ( 145.0000000000000568, -87.50000000000000000, 65.00000000000000000 ) ) ;
#10460 = FACE_OUTER_BOUND ( 'NONE', #32174, .T. ) ;
#10461 = ADVANCED_FACE ( 'NONE', ( #25007 ), #9175, .F. ) ;
#10462 = ADVANCED_FACE ( 'NONE', ( #642 ), #19342, .T. ) ;
#10463 = DIRECTION ( 'NONE',  ( -1.000000000000000000, 6.792721752314501023E-48, -3.697785493223492838E-32 ) ) ;
#10464 = CARTESIAN_POINT ( 'NONE',  ( -430.0000000000000000, -131.0000000000000000, 111.9999999999999858 ) ) ;
#10465 = VERTEX_POINT ( 'NONE', #30547 ) ;
#10466 = CARTESIAN_POINT ( 'NONE',  ( 1.395000000000002238, 34.10861917999622506, -4.581348211831717698 ) ) ;
#10467 = CARTESIAN_POINT ( 'NONE',  ( -8.216995152909043008E-14, -30.07763130521195549, 5.961539033704580604 ) ) ;
#10468 = EDGE_CURVE ( 'NONE', #7115, #21282, #3648, .T. ) ;
#10469 = CARTESIAN_POINT ( 'NONE',  ( 0.000000000000000000, 9.797174393178825657E-16, -8.000000000000000000 ) ) ;
#10470 = VERTEX_POINT ( 'NONE', #22180 ) ;
#10471 = AXIS2_PLACEMENT_3D ( 'NONE', #294, #14362, #19519 ) ;
#10472 = PLANE ( 'NONE',  #12121 ) ;
#10473 = ORIENTED_EDGE ( 'NONE', *, *, #26035, .T. ) ;
#10474 = VECTOR ( 'NONE', #33998, 1000.000000000000000 ) ;
#10475 = LINE ( 'NONE', #29868, #27395 ) ;
#10476 = DIRECTION ( 'NONE',  ( 0.2149704402110243495, 0.9766205557100865464, 0.000000000000000000 ) ) ;
#10477 = VERTEX_POINT ( 'NONE', #16097 ) ;
#10478 = VECTOR ( 'NONE', #7299, 1000.000000000000000 ) ;
#10479 = VERTEX_POINT ( 'NONE', #3472 ) ;
#10480 = AXIS2_PLACEMENT_3D ( 'NONE', #4240, #34326, #9947 ) ;
#10481 = PLANE ( 'NONE',  #27393 ) ;
#10482 = LINE ( 'NONE', #32353, #16827 ) ;
#10483 = PLANE ( 'NONE',  #6921 ) ;
#10484 = CIRCLE ( 'NONE', #23562, 32.54542015209055705 ) ;
#10485 = ORIENTED_EDGE ( 'NONE', *, *, #5283, .F. ) ;
#10486 = EDGE_CURVE ( 'NONE', #32001, #1801, #22005, .T. ) ;
#10487 = EDGE_CURVE ( 'NONE', #11116, #26377, #30013, .T. ) ;
#10488 = ORIENTED_EDGE ( 'NONE', *, *, #23625, .T. ) ;
#10489 = CARTESIAN_POINT ( 'NONE',  ( 771.2150972410445320, 1204.030662439342905, 1753.598338701303419 ) ) ;
#10490 = ORIENTED_EDGE ( 'NONE', *, *, #8887, .T. ) ;
#10491 = CARTESIAN_POINT ( 'NONE',  ( 22.10765473302597073, -16.64466345897532662, -77.50000000000000000 ) ) ;
#10492 = EDGE_CURVE ( 'NONE', #26511, #27718, #819, .T. ) ;
#10493 = CARTESIAN_POINT ( 'NONE',  ( -6.500000000000000000, 0.000000000000000000, -0.7500000000000000000 ) ) ;
#10494 = LINE ( 'NONE', #24180, #28668 ) ;
#10495 = CARTESIAN_POINT ( 'NONE',  ( -20.00000000000004619, -105.0000000000000000, -162.9999999999999716 ) ) ;
#10497 = EDGE_CURVE ( 'NONE', #18208, #33010, #8836, .T. ) ;
#10496 = EDGE_LOOP ( 'NONE', ( #5054, #9058, #22688, #30759 ) ) ;
#10498 = LINE ( 'NONE', #32201, #5557 ) ;
#10499 = VECTOR ( 'NONE', #33303, 1000.000000000000000 ) ;
#10500 = CARTESIAN_POINT ( 'NONE',  ( 1.205771365940040196, 7.794228634059932048, -13.49999999999999822 ) ) ;
#10502 = CARTESIAN_POINT ( 'NONE',  ( 2.719010670160031395, -11.11630839801615167, 29.68118041677924168 ) ) ;
#10501 = PLANE ( 'NONE',  #4229 ) ;
#10503 = AXIS2_PLACEMENT_3D ( 'NONE', #3060, #16440, #33138 ) ;
#10504 = VERTEX_POINT ( 'NONE', #33382 ) ;
#10505 = VERTEX_POINT ( 'NONE', #295 ) ;
#10506 = VECTOR ( 'NONE', #12499, 1000.000000000000000 ) ;
#10507 = LINE ( 'NONE', #26864, #15176 ) ;
#10508 = VERTEX_POINT ( 'NONE', #11687 ) ;
#10509 = AXIS2_PLACEMENT_3D ( 'NONE', #20090, #30755, #1563 ) ;
#10510 = CARTESIAN_POINT ( 'NONE',  ( -355.0000000000000000, 118.9999999999999858, 128.0000000000000000 ) ) ;
#10511 = DIRECTION ( 'NONE',  ( 1.000000000000000000, 0.000000000000000000, 0.000000000000000000 ) ) ;
#10512 = EDGE_LOOP ( 'NONE', ( #13701, #2903, #2173, #6832 ) ) ;
#10513 = CARTESIAN_POINT ( 'NONE',  ( 2.789999999999999147, -22.61000311763331183, -20.38038735157106274 ) ) ;
#10514 = CARTESIAN_POINT ( 'NONE',  ( 10.17231796313409298, 6.310691531022070144, -77.50000000000000000 ) ) ;
#10515 = ORIENTED_EDGE ( 'NONE', *, *, #31143, .F. ) ;
#10516 = EDGE_CURVE ( 'NONE', #30837, #31738, #14181, .T. ) ;
#10517 = DIRECTION ( 'NONE',  ( 1.000000000000000000, 0.000000000000000000, -0.000000000000000000 ) ) ;
#10518 = DIRECTION ( 'NONE',  ( 1.000000000000000000, 0.000000000000000000, -1.232595164407831220E-32 ) ) ;
#10519 = LINE ( 'NONE', #24379, #20118 ) ;
#10521 = CARTESIAN_POINT ( 'NONE',  ( -30.58418286738120884, -22.31615353445078043, -36.68877005347593467 ) ) ;
#10520 = CARTESIAN_POINT ( 'NONE',  ( 1.999999999999999556, 0.000000000000000000, -0.7500000000000000000 ) ) ;
#10522 = VECTOR ( 'NONE', #6049, 1000.000000000000000 ) ;
#10523 = LINE ( 'NONE', #1796, #26780 ) ;
#10524 = CARTESIAN_POINT ( 'NONE',  ( 1.040000000000000924, 0.000000000000000000, 0.000000000000000000 ) ) ;
#10525 = LINE ( 'NONE', #7841, #24025 ) ;
#10526 = B_SPLINE_CURVE_WITH_KNOTS ( 'NONE', 3,
 ( #7658, #29212, #26707, #34724 ),
 .UNSPECIFIED., .F., .F.,
 ( 4, 4 ),
 ( 0.005298612564832130140, 0.005985477723952354126 ),
 .UNSPECIFIED. ) ;
#10527 = AXIS2_PLACEMENT_3D ( 'NONE', #26688, #2293, #13171 ) ;
#10528 = EDGE_CURVE ( 'NONE', #24474, #10186, #20428, .T. ) ;
#10529 = CARTESIAN_POINT ( 'NONE',  ( 0.000000000000000000, -14.75935258146395412, -26.65732927035534416 ) ) ;
#10530 = ADVANCED_FACE ( 'NONE', ( #998 ), #3911, .T. ) ;
#10531 = ADVANCED_FACE ( 'NONE', ( #28042 ), #6138, .F. ) ;
#10533 = ORIENTED_EDGE ( 'NONE', *, *, #34633, .F. ) ;
#10532 = AXIS2_PLACEMENT_3D ( 'NONE', #320, #29207, #23855 ) ;
#10535 = AXIS2_PLACEMENT_3D ( 'NONE', #5679, #27060, #30255 ) ;
#10534 = DIRECTION ( 'NONE',  ( -0.000000000000000000, -1.836970198721029688E-16, 1.000000000000000000 ) ) ;
#10536 = SHAPE_REPRESENTATION_RELATIONSHIP ( 'NONE' , 'NONE' ,  #8672, #15210 ) ;
#10537 = EDGE_LOOP ( 'NONE', ( #4655, #432, #13292, #24080 ) ) ;
#10538 = ORIENTED_EDGE ( 'NONE', *, *, #28939, .T. ) ;
#10539 = CARTESIAN_POINT ( 'NONE',  ( 109.2869635376109443, 3.831042253767035444, 6.454752727393734624 ) ) ;
#10540 =( NAMED_UNIT ( * ) SI_UNIT ( $, .STERADIAN. ) SOLID_ANGLE_UNIT ( ) );
#10541 = ORIENTED_EDGE ( 'NONE', *, *, #6753, .T. ) ;
#10542 = DIRECTION ( 'NONE',  ( 0.000000000000000000, -5.145227585319922065E-49, -1.000000000000000000 ) ) ;
#10543 =( NAMED_UNIT ( * ) PLANE_ANGLE_UNIT ( ) SI_UNIT ( $, .RADIAN. ) );
#10544 = AXIS2_PLACEMENT_3D ( 'NONE', #29501, #26818, #32498 ) ;
#10545 = CARTESIAN_POINT ( 'NONE',  ( 1.040000000000000924, 0.000000000000000000, 0.000000000000000000 ) ) ;
#10546 = B_SPLINE_CURVE_WITH_KNOTS ( 'NONE', 3,
 ( #21819, #32675, #4909, #7761 ),
 .UNSPECIFIED., .F., .F.,
 ( 4, 4 ),
 ( 0.005298361175080958108, 0.005985229640890899275 ),
 .UNSPECIFIED. ) ;
#10547 = ORIENTED_EDGE ( 'NONE', *, *, #8852, .T. ) ;
#10548 = ORIENTED_EDGE ( 'NONE', *, *, #23072, .T. ) ;
#10549 = LINE ( 'NONE', #15907, #12332 ) ;
#10550 = AXIS2_PLACEMENT_3D ( 'NONE', #28377, #18064, #12011 ) ;
#10551 = DIRECTION ( 'NONE',  ( -1.000000000000000000, -0.000000000000000000, -0.000000000000000000 ) ) ;
#10552 = VECTOR ( 'NONE', #22551, 1000.000000000000000 ) ;
#10553 = DIRECTION ( 'NONE',  ( 0.000000000000000000, 0.000000000000000000, 1.000000000000000000 ) ) ;
#10554 = DIRECTION ( 'NONE',  ( -1.000000000000000000, 0.000000000000000000, 0.000000000000000000 ) ) ;
#10555 = CARTESIAN_POINT ( 'NONE',  ( 145.0000000000000568, -78.33668825982573480, -63.00000000000000000 ) ) ;
#10556 = EDGE_LOOP ( 'NONE', ( #950, #7278, #10713, #28471 ) ) ;
#10557 = DIRECTION ( 'NONE',  ( 0.000000000000000000, 1.000000000000000000, 0.000000000000000000 ) ) ;
#10558 = DIRECTION ( 'NONE',  ( -1.000000000000000000, 0.000000000000000000, -1.300283923313630633E-47 ) ) ;
#10559 = CARTESIAN_POINT ( 'NONE',  ( 2.765921099433441999, -15.32140196853772984, 27.05343472112986092 ) ) ;
#10560 = CIRCLE ( 'NONE', #9425, 1.999999999999999112 ) ;
#10561 = CARTESIAN_POINT ( 'NONE',  ( 127.4999999999999147, 1.530808498934191521E-15, -12.50000000000000000 ) ) ;
#10562 = DIRECTION ( 'NONE',  ( -1.000000000000000000, 0.000000000000000000, -1.300283923313630633E-47 ) ) ;
#10563 = LINE ( 'NONE', #16265, #19509 ) ;
#10565 = CARTESIAN_POINT ( 'NONE',  ( -12.00000000000001066, -56.99999999999997868, 154.9999999999999716 ) ) ;
#10564 = CARTESIAN_POINT ( 'NONE',  ( 0.02407890056655695096, -23.70329957282599764, 20.11932597908820242 ) ) ;
#10566 = EDGE_CURVE ( 'NONE', #20271, #1001, #25366, .T. ) ;
#10567 = CARTESIAN_POINT ( 'NONE',  ( 11.99999999999999645, -124.9999999999999432, -154.9999999999999716 ) ) ;
#10568 = ORIENTED_EDGE ( 'NONE', *, *, #24560, .T. ) ;
#10569 = CARTESIAN_POINT ( 'NONE',  ( 106.8659954277186586, 5.439315735761661941, -11.25565174199232743 ) ) ;
#10571 = FACE_OUTER_BOUND ( 'NONE', #13045, .T. ) ;
#10570 = DIRECTION ( 'NONE',  ( 0.000000000000000000, 1.000000000000000000, 0.000000000000000000 ) ) ;
#10572 = EDGE_CURVE ( 'NONE', #10822, #10259, #22718, .T. ) ;
#10573 = CIRCLE ( 'NONE', #13442, 7.999999999999979572 ) ;
#10574 = EDGE_CURVE ( 'NONE', #28861, #11080, #24655, .T. ) ;
#10575 = ORIENTED_EDGE ( 'NONE', *, *, #19026, .T. ) ;
#10576 = DIRECTION ( 'NONE',  ( 0.000000000000000000, 1.836970198721029441E-16, -1.000000000000000000 ) ) ;
#10577 = EDGE_CURVE ( 'NONE', #31670, #17427, #11331, .T. ) ;
#10578 = VECTOR ( 'NONE', #2566, 1000.000000000000000 ) ;
#10579 = ORIENTED_EDGE ( 'NONE', *, *, #4085, .F. ) ;
#10580 =( REPRESENTATION_RELATIONSHIP ('NONE','NONE', #23037, #15767 ) REPRESENTATION_RELATIONSHIP_WITH_TRANSFORMATION ( #17964 )SHAPE_REPRESENTATION_RELATIONSHIP( ) );
#10581 = EDGE_LOOP ( 'NONE', ( #8589, #12296, #11638, #8240 ) ) ;
#10582 = DIRECTION ( 'NONE',  ( 0.000000000000000000, -1.000000000000000000, 2.309213040847544338E-50 ) ) ;
#10583 = ORIENTED_EDGE ( 'NONE', *, *, #4996, .F. ) ;
#10584 = EDGE_LOOP ( 'NONE', ( #28746, #13086, #14609, #19170 ) ) ;
#10585 = LINE ( 'NONE', #23572, #22995 ) ;
#10586 = AXIS2_PLACEMENT_3D ( 'NONE', #21893, #10702, #29385 ) ;
#10587 = EDGE_CURVE ( 'NONE', #26714, #28665, #30359, .T. ) ;
#10588 = CIRCLE ( 'NONE', #23098, 7.999999999999979572 ) ;
#10589 = LINE ( 'NONE', #18430, #30562 ) ;
#10590 = CARTESIAN_POINT ( 'NONE',  ( 1.749999999999999778, -30.02688531850381182, -16.81585001935615153 ) ) ;
#10591 = ORIENTED_EDGE ( 'NONE', *, *, #12397, .T. ) ;
#10592 = ORIENTED_EDGE ( 'NONE', *, *, #7525, .T. ) ;
#10593 = LINE ( 'NONE', #26772, #5441 ) ;
#10594 = CARTESIAN_POINT ( 'NONE',  ( -5.344999999999999751, 0.000000000000000000, -0.7520000000000001128 ) ) ;
#10595 = PLANE ( 'NONE',  #12471 ) ;
#10596 = DIRECTION ( 'NONE',  ( 0.000000000000000000, -1.000000000000000000, 0.000000000000000000 ) ) ;
#10597 = ORIENTED_EDGE ( 'NONE', *, *, #29830, .F. ) ;
#10598 = VECTOR ( 'NONE', #18912, 1000.000000000000000 ) ;
#10599 = CARTESIAN_POINT ( 'NONE',  ( -15.99999999999998579, -145.0000000000000000, 162.9999999999999716 ) ) ;
#10600 = LINE ( 'NONE', #11127, #10184 ) ;
#10601 = ORIENTED_EDGE ( 'NONE', *, *, #4788, .F. ) ;
#10602 = VECTOR ( 'NONE', #26655, 1000.000000000000000 ) ;
#10603 = DIRECTION ( 'NONE',  ( -0.000000000000000000, -0.000000000000000000, -1.000000000000000000 ) ) ;
#10604 = CARTESIAN_POINT ( 'NONE',  ( -365.0000000000000000, -131.0000000000000000, 111.9999999999999858 ) ) ;
#10605 = DIRECTION ( 'NONE',  ( 0.000000000000000000, -1.000000000000000000, 1.310824597558155437E-49 ) ) ;
#10606 = ORIENTED_EDGE ( 'NONE', *, *, #7697, .F. ) ;
#10607 = DIRECTION ( 'NONE',  ( 1.000000000000000000, 0.000000000000000000, 0.000000000000000000 ) ) ;
#10608 = ORIENTED_EDGE ( 'NONE', *, *, #24689, .T. ) ;
#10609 = DIRECTION ( 'NONE',  ( 0.000000000000000000, 0.000000000000000000, -1.000000000000000000 ) ) ;
#10610 = EDGE_LOOP ( 'NONE', ( #19690, #26799, #25086, #13853 ) ) ;
#10612 = DIRECTION ( 'NONE',  ( 0.000000000000000000, 1.000000000000000000, 1.836970198721029688E-16 ) ) ;
#10611 = CARTESIAN_POINT ( 'NONE',  ( 0.02407890056655521624, 28.29688452313399338, 12.88099432405614309 ) ) ;
#10613 = SURFACE_STYLE_FILL_AREA ( #13628 ) ;
#10614 = ADVANCED_FACE ( 'NONE', ( #4171 ), #31241, .F. ) ;
#10615 = ORIENTED_EDGE ( 'NONE', *, *, #20893, .F. ) ;
#10616 = DIRECTION ( 'NONE',  ( -1.000000000000000000, 0.000000000000000000, 0.000000000000000000 ) ) ;
#10617 = EDGE_CURVE ( 'NONE', #25524, #17023, #27805, .T. ) ;
#10618 = AXIS2_PLACEMENT_3D ( 'NONE', #16789, #33485, #22986 ) ;
#10619 = ADVANCED_FACE ( 'NONE', ( #30890 ), #10183, .T. ) ;
#10620 = VERTEX_POINT ( 'NONE', #1169 ) ;
#10621 = CIRCLE ( 'NONE', #26536, 7.999999999999979572 ) ;
#10622 = EDGE_CURVE ( 'NONE', #5027, #7621, #34929, .T. ) ;
#10623 = EDGE_CURVE ( 'NONE', #404, #3001, #12869, .T. ) ;
#10624 = CARTESIAN_POINT ( 'NONE',  ( 765.1790577462007832, 1363.554574543319177, 1753.598338701304328 ) ) ;
#10625 = ORIENTED_EDGE ( 'NONE', *, *, #22105, .F. ) ;
#10626 = CARTESIAN_POINT ( 'NONE',  ( -103.6327063011913623, 4.940661300061107042, 5.643441299694565316 ) ) ;
#10627 = ORIENTED_EDGE ( 'NONE', *, *, #18951, .T. ) ;
#10628 = DIRECTION ( 'NONE',  ( 0.000000000000000000, 0.000000000000000000, -1.000000000000000000 ) ) ;
#10629 = CARTESIAN_POINT ( 'NONE',  ( -104.6531427807880306, -5.115148824049938092, -5.485002510375801776 ) ) ;
#10630 = DIRECTION ( 'NONE',  ( -1.000000000000000000, 0.000000000000000000, 0.000000000000000000 ) ) ;
#10631 = ORIENTED_EDGE ( 'NONE', *, *, #33632, .T. ) ;
#10632 = ORIENTED_EDGE ( 'NONE', *, *, #8046, .T. ) ;
#10633 = EDGE_LOOP ( 'NONE', ( #7263, #28083, #29714, #12485 ) ) ;
#10634 = CARTESIAN_POINT ( 'NONE',  ( 28.23027531293552528, -10.15143121711728469, 0.000000000000000000 ) ) ;
#10635 = DIRECTION ( 'NONE',  ( -0.000000000000000000, -1.836970198721029688E-16, 1.000000000000000000 ) ) ;
#10636 = EDGE_CURVE ( 'NONE', #9815, #27727, #12219, .T. ) ;
#10637 = CARTESIAN_POINT ( 'NONE',  ( 18.19419936998244225, -33.21164777187627237, 49.43553178847298568 ) ) ;
#10638 = DIRECTION ( 'NONE',  ( 1.000000000000000000, -0.000000000000000000, -0.000000000000000000 ) ) ;
#10639 = DIRECTION ( 'NONE',  ( -1.000000000000000000, -0.000000000000000000, 0.000000000000000000 ) ) ;
#10640 = DIRECTION ( 'NONE',  ( 0.000000000000000000, -0.9961946980917453232, 0.08715574274766170471 ) ) ;
#10641 = DIRECTION ( 'NONE',  ( 0.000000000000000000, 0.000000000000000000, 1.000000000000000000 ) ) ;
#10642 = ORIENTED_EDGE ( 'NONE', *, *, #19538, .F. ) ;
#10643 = AXIS2_PLACEMENT_3D ( 'NONE', #30956, #33446, #535 ) ;
#10644 = CARTESIAN_POINT ( 'NONE',  ( 35.44043929807611448, -17.65143121711728469, 10.00000000000000000 ) ) ;
#10645 = CARTESIAN_POINT ( 'NONE',  ( -442.0000000000000000, 145.0000000000000000, -175.0000000000000000 ) ) ;
#10646 = DIRECTION ( 'NONE',  ( -1.000000000000000000, 0.000000000000000000, 0.000000000000000000 ) ) ;
#10647 = ORIENTED_EDGE ( 'NONE', *, *, #27607, .F. ) ;
#10648 = VECTOR ( 'NONE', #34582, 1000.000000000000000 ) ;
#10649 = AXIS2_PLACEMENT_3D ( 'NONE', #11429, #19632, #2708 ) ;
#10650 = EDGE_CURVE ( 'NONE', #980, #7256, #32909, .T. ) ;
#10651 = LINE ( 'NONE', #35038, #33130 ) ;
#10652 = ORIENTED_EDGE ( 'NONE', *, *, #8582, .F. ) ;
#10653 = CARTESIAN_POINT ( 'NONE',  ( -104.3222861221629358, 5.081071289440265204, -11.42094332255972766 ) ) ;
#10654 = DIRECTION ( 'NONE',  ( 1.000000000000000000, 0.000000000000000000, 0.000000000000000000 ) ) ;
#10655 = VECTOR ( 'NONE', #24845, 1000.000000000000000 ) ;
#10656 = ORIENTED_EDGE ( 'NONE', *, *, #15964, .F. ) ;
#10657 = CARTESIAN_POINT ( 'NONE',  ( -418.0000000000000000, 105.0000000000000000, 135.9999999999999716 ) ) ;
#10658 = CIRCLE ( 'NONE', #30554, 7.999999999999979572 ) ;
#10659 = CARTESIAN_POINT ( 'NONE',  ( 6.857172176539690689, 37.23415287044793587, 68.31122994652405112 ) ) ;
#10660 = DIRECTION ( 'NONE',  ( -1.000000000000000000, -0.000000000000000000, -0.000000000000000000 ) ) ;
#10661 = B_SPLINE_CURVE_WITH_KNOTS ( 'NONE', 3,
 ( #13323, #18670, #35036, #18837, #2267, #15994 ),
 .UNSPECIFIED., .F., .F.,
 ( 4, 2, 4 ),
 ( 4.404817005620078000E-07, 0.001874269608671721770, 0.003748098735642881301 ),
 .UNSPECIFIED. ) ;
#10662 = ORIENTED_EDGE ( 'NONE', *, *, #6080, .F. ) ;
#10663 = VERTEX_POINT ( 'NONE', #4822 ) ;
#10664 = TOROIDAL_SURFACE ( 'NONE', #23742, 30.47050528711512030, 8.000000000000000000 ) ;
#10665 = EDGE_CURVE ( 'NONE', #16556, #18985, #2222, .T. ) ;
#10666 = ADVANCED_FACE ( 'NONE', ( #12041, #6839 ), #22888, .T. ) ;
#10667 = DIRECTION ( 'NONE',  ( -7.893605728314050488E-14, 1.618803117314786135E-15, 0.9999999999999998890 ) ) ;
#10668 = VECTOR ( 'NONE', #7536, 1000.000000000000000 ) ;
#10669 = DIRECTION ( 'NONE',  ( 0.000000000000000000, 0.000000000000000000, 1.000000000000000000 ) ) ;
#10670 = ORIENTED_EDGE ( 'NONE', *, *, #26217, .T. ) ;
#10671 = DIRECTION ( 'NONE',  ( 0.000000000000000000, 0.000000000000000000, 1.000000000000000000 ) ) ;
#10672 = PLANE ( 'NONE',  #31709 ) ;
#10673 = AXIS2_PLACEMENT_3D ( 'NONE', #8486, #13652, #33030 ) ;
#10674 = CIRCLE ( 'NONE', #27144, 4.750000000000004441 ) ;
#10675 = CARTESIAN_POINT ( 'NONE',  ( 19.99999999999998224, 144.9999999999999147, 187.0000000000000000 ) ) ;
#10676 = CARTESIAN_POINT ( 'NONE',  ( -100.4263556498910646, -2.314419832420931744, 7.141071956987316227 ) ) ;
#10677 = ORIENTED_EDGE ( 'NONE', *, *, #9535, .F. ) ;
#10678 = DIRECTION ( 'NONE',  ( 0.000000000000000000, 0.000000000000000000, -1.000000000000000000 ) ) ;
#10679 = ADVANCED_FACE ( 'NONE', ( #18385 ), #21563, .T. ) ;
#10680 = AXIS2_PLACEMENT_3D ( 'NONE', #12181, #9498, #25506 ) ;
#10682 = CARTESIAN_POINT ( 'NONE',  ( 20.89386240318430410, 24.95297350523386726, 68.31122994652405112 ) ) ;
#10681 = LINE ( 'NONE', #16387, #7046 ) ;
#10683 = ORIENTED_EDGE ( 'NONE', *, *, #9414, .T. ) ;
#10684 = ORIENTED_EDGE ( 'NONE', *, *, #25499, .F. ) ;
#10685 = DIRECTION ( 'NONE',  ( 0.000000000000000000, 1.836970198721029441E-16, -1.000000000000000000 ) ) ;
#10686 = ORIENTED_EDGE ( 'NONE', *, *, #20034, .T. ) ;
#10687 = EDGE_CURVE ( 'NONE', #31399, #9316, #24509, .T. ) ;
#10688 = CARTESIAN_POINT ( 'NONE',  ( 2.790000000000081748, -3.624739946993785988, -30.44774159452265039 ) ) ;
#10689 = DIRECTION ( 'NONE',  ( 0.000000000000000000, 1.836970198721029441E-16, -1.000000000000000000 ) ) ;
#10690 = ORIENTED_EDGE ( 'NONE', *, *, #29486, .F. ) ;
#10691 = EDGE_CURVE ( 'NONE', #16381, #1315, #15322, .T. ) ;
#10693 = EDGE_CURVE ( 'NONE', #32960, #2754, #3991, .T. ) ;
#10692 = ORIENTED_EDGE ( 'NONE', *, *, #13140, .F. ) ;
#10694 = CYLINDRICAL_SURFACE ( 'NONE', #27170, 16.19999999999999574 ) ;
#10695 = CIRCLE ( 'NONE', #8983, 4.750000000000004441 ) ;
#10696 = DIRECTION ( 'NONE',  ( 0.000000000000000000, -0.000000000000000000, -1.000000000000000000 ) ) ;
#10697 = ORIENTED_EDGE ( 'NONE', *, *, #12806, .T. ) ;
#10698 = DIRECTION ( 'NONE',  ( 0.000000000000000000, 1.836970198721029688E-16, -1.000000000000000000 ) ) ;
#10699 = DIRECTION ( 'NONE',  ( 0.000000000000000000, 0.000000000000000000, -1.000000000000000000 ) ) ;
#10700 = EDGE_CURVE ( 'NONE', #7073, #24311, #14887, .T. ) ;
#10701 = LINE ( 'NONE', #5333, #11581 ) ;
#10702 = DIRECTION ( 'NONE',  ( -1.000000000000000000, -0.000000000000000000, -0.000000000000000000 ) ) ;
#10703 = AXIS2_PLACEMENT_3D ( 'NONE', #19103, #32596, #12885 ) ;
#10704 = AXIS2_PLACEMENT_3D ( 'NONE', #28296, #19935, #28112 ) ;
#10705 = LINE ( 'NONE', #27235, #13726 ) ;
#10706 = DIRECTION ( 'NONE',  ( -0.9868265225415261410, -0.1617819965527648174, 0.000000000000000000 ) ) ;
#10707 = LINE ( 'NONE', #18557, #19508 ) ;
#10708 = AXIS2_PLACEMENT_3D ( 'NONE', #23201, #1137, #34045 ) ;
#10709 = ORIENTED_EDGE ( 'NONE', *, *, #8350, .F. ) ;
#10710 = DIRECTION ( 'NONE',  ( 3.697785493223492838E-32, 1.934419779023891545E-16, -1.000000000000000000 ) ) ;
#10711 = UNCERTAINTY_MEASURE_WITH_UNIT (LENGTH_MEASURE( 1.000000000000000082E-05 ), #6790, 'distance_accuracy_value', 'NONE');
#10713 = ORIENTED_EDGE ( 'NONE', *, *, #33727, .T. ) ;
#10712 = MANIFOLD_SOLID_BREP ( 'Cut-Extrude1', #29869 ) ;
#10714 = ORIENTED_EDGE ( 'NONE', *, *, #11587, .F. ) ;
#10715 = VECTOR ( 'NONE', #6053, 1000.000000000000000 ) ;
#10716 = CARTESIAN_POINT ( 'NONE',  ( -7.700000000000000178, 1.959434878635765131E-15, 16.00000000000000000 ) ) ;
#10717 = APPLICATION_PROTOCOL_DEFINITION ( 'draft international standard', 'automotive_design', 1998, #18758 ) ;
#10718 = EDGE_LOOP ( 'NONE', ( #9822, #12513, #15546, #22496 ) ) ;
#10719 = DIRECTION ( 'NONE',  ( 0.000000000000000000, 1.000000000000000000, -3.374343856708137958E-53 ) ) ;
#10720 = DIRECTION ( 'NONE',  ( 1.000000000000000000, 3.469446951953834515E-18, 0.000000000000000000 ) ) ;
#10721 = VECTOR ( 'NONE', #728, 1000.000000000000000 ) ;
#10722 = CARTESIAN_POINT ( 'NONE',  ( 10.17231796313407344, -3.615060903476079890, -77.50000000000000000 ) ) ;
#10723 = ORIENTED_EDGE ( 'NONE', *, *, #34139, .T. ) ;
#10724 = ORIENTED_EDGE ( 'NONE', *, *, #21845, .F. ) ;
#10725 = AXIS2_PLACEMENT_3D ( 'NONE', #26330, #1604, #4958 ) ;
#10726 = FACE_OUTER_BOUND ( 'NONE', #31814, .T. ) ;
#10727 = DIRECTION ( 'NONE',  ( 0.000000000000000000, 0.000000000000000000, 1.000000000000000000 ) ) ;
#10728 = B_SPLINE_CURVE_WITH_KNOTS ( 'NONE', 3,
 ( #23945, #18982, #21806, #32310 ),
 .UNSPECIFIED., .F., .F.,
 ( 4, 4 ),
 ( 2.250995564674898728E-07, 0.0006879610227482087616 ),
 .UNSPECIFIED. ) ;
#10729 = CARTESIAN_POINT ( 'NONE',  ( -5.210000000000000853, 0.000000000000000000, 0.000000000000000000 ) ) ;
#10730 = CARTESIAN_POINT ( 'NONE',  ( -19.99999999999998934, 134.9999999999998863, 162.9999999999999716 ) ) ;
#10731 = DIRECTION ( 'NONE',  ( 0.000000000000000000, 1.000000000000000000, 0.000000000000000000 ) ) ;
#10732 = ORIENTED_EDGE ( 'NONE', *, *, #13663, .F. ) ;
#10733 = CIRCLE ( 'NONE', #1047, 7.999999999999979572 ) ;
#10734 = EDGE_CURVE ( 'NONE', #8663, #28119, #28576, .T. ) ;
#10735 = DIRECTION ( 'NONE',  ( 0.000000000000000000, 0.000000000000000000, 1.000000000000000000 ) ) ;
#10736 = CARTESIAN_POINT ( 'NONE',  ( 2.604019705000863993, -30.94574698966636106, 9.190792961030121333 ) ) ;
#10737 = EDGE_CURVE ( 'NONE', #10179, #23824, #31223, .T. ) ;
#10738 = LINE ( 'NONE', #219, #31686 ) ;
#10739 = CARTESIAN_POINT ( 'NONE',  ( 1.395000000000002238, -2.430610048905781806, -34.32897884578301984 ) ) ;
#10740 = CARTESIAN_POINT ( 'NONE',  ( -20.02113311122509032, -13.65249191622732816, -67.50000000000000000 ) ) ;
#10742 = DIRECTION ( 'NONE',  ( 1.000000000000000000, 0.000000000000000000, 0.000000000000000000 ) ) ;
#10741 = LINE ( 'NONE', #18588, #17333 ) ;
#10743 = CARTESIAN_POINT ( 'NONE',  ( 37.55078559520313775, -4.831299144296470338, 68.31122994652405112 ) ) ;
#10744 = ORIENTED_EDGE ( 'NONE', *, *, #23109, .F. ) ;
#10745 = PLANE ( 'NONE',  #4234 ) ;
#10747 = DIRECTION ( 'NONE',  ( 0.000000000000000000, 0.000000000000000000, -1.000000000000000000 ) ) ;
#10746 = CYLINDRICAL_SURFACE ( 'NONE', #29146, 11.80000000000000071 ) ;
#10748 = AXIS2_PLACEMENT_3D ( 'NONE', #10493, #21351, #22219 ) ;
#10749 = ORIENTED_EDGE ( 'NONE', *, *, #7985, .F. ) ;
#10750 = FACE_OUTER_BOUND ( 'NONE', #17032, .T. ) ;
#10751 = PRODUCT_DEFINITION_SHAPE ( 'NONE', 'NONE',  #35223 ) ;
#10752 = B_SPLINE_CURVE_WITH_KNOTS ( 'NONE', 3,
 ( #16729, #2824, #24522, #349 ),
 .UNSPECIFIED., .F., .F.,
 ( 4, 4 ),
 ( 2.042209043309391692E-07, 0.0006879399691688898233 ),
 .UNSPECIFIED. ) ;
#10753 = VERTEX_POINT ( 'NONE', #388 ) ;
#10754 = COLOUR_RGB ( '',0.7921568627450980005, 0.8196078431372548767, 0.9333333333333333481 ) ;
#10755 = ORIENTED_EDGE ( 'NONE', *, *, #34192, .T. ) ;
#10756 = FACE_BOUND ( 'NONE', #10969, .T. ) ;
#10757 = VERTEX_POINT ( 'NONE', #32582 ) ;
#10758 = ORIENTED_EDGE ( 'NONE', *, *, #4740, .F. ) ;
#10759 = CARTESIAN_POINT ( 'NONE',  ( 2.779215089232839109, 28.09152240582078974, -12.86217335695007868 ) ) ;
#10760 = AXIS2_PLACEMENT_3D ( 'NONE', #7150, #4478, #15370 ) ;
#10761 = LINE ( 'NONE', #10930, #9571 ) ;
#10762 = FACE_OUTER_BOUND ( 'NONE', #30248, .T. ) ;
#10763 = VERTEX_POINT ( 'NONE', #16243 ) ;
#10764 = ORIENTED_EDGE ( 'NONE', *, *, #22211, .T. ) ;
#10765 = CARTESIAN_POINT ( 'NONE',  ( -14.84098889165989377, 28.96462362251111244, 68.31122994652405112 ) ) ;
#10766 = CARTESIAN_POINT ( 'NONE',  ( -20.63749999999999574, 0.000000000000000000, -14.20000000000000107 ) ) ;
#10767 = MANIFOLD_SOLID_BREP ( 'Square tube 40 X 40 X 4(1)[13]', #18508 ) ;
#10768 = EDGE_CURVE ( 'NONE', #34323, #27344, #29930, .T. ) ;
#10769 = CARTESIAN_POINT ( 'NONE',  ( 11.99999999999995559, -145.0000000000000000, -186.9999999999999716 ) ) ;
#10770 = DIRECTION ( 'NONE',  ( 0.000000000000000000, 0.000000000000000000, 1.000000000000000000 ) ) ;
#10771 = ORIENTED_EDGE ( 'NONE', *, *, #33429, .T. ) ;
#10772 = VECTOR ( 'NONE', #35014, 1000.000000000000000 ) ;
#10773 = CARTESIAN_POINT ( 'NONE',  ( 212.5000000000000000, 9.184850993605147944E-16, -7.500000000000000000 ) ) ;
#10774 = EDGE_CURVE ( 'NONE', #26696, #12145, #24396, .T. ) ;
#10775 = CARTESIAN_POINT ( 'NONE',  ( 10.00000000000000000, -15.58845726811992627, 0.000000000000000000 ) ) ;
#10776 = VERTEX_POINT ( 'NONE', #5871 ) ;
#10777 = CARTESIAN_POINT ( 'NONE',  ( -499.9999999999999432, 140.9999999999999716, 187.0000000000000000 ) ) ;
#10778 = DIRECTION ( 'NONE',  ( -1.000000000000000000, -0.000000000000000000, 0.000000000000000000 ) ) ;
#10779 = DIRECTION ( 'NONE',  ( 0.000000000000000000, -2.465190328815661892E-32, -1.000000000000000000 ) ) ;
#10780 = DIRECTION ( 'NONE',  ( 0.000000000000000000, 0.000000000000000000, 1.000000000000000000 ) ) ;
#10781 = VERTEX_POINT ( 'NONE', #21733 ) ;
#10782 = CARTESIAN_POINT ( 'NONE',  ( -5.021133111224679091, 24.02303923978505296, -87.50000000000000000 ) ) ;
#10783 = ORIENTED_EDGE ( 'NONE', *, *, #14522, .T. ) ;
#10785 = DIRECTION ( 'NONE',  ( 0.000000000000000000, 1.836970198721029441E-16, -1.000000000000000000 ) ) ;
#10784 = DIRECTION ( 'NONE',  ( 1.232595164407831220E-32, -3.421138828918010427E-49, 1.000000000000000000 ) ) ;
#10786 = CARTESIAN_POINT ( 'NONE',  ( -12.00000000000001066, 112.9999999999999574, -175.0000000000000284 ) ) ;
#10787 = AXIS2_PLACEMENT_3D ( 'NONE', #27964, #28494, #1092 ) ;
#10788 = ORIENTED_EDGE ( 'NONE', *, *, #5002, .F. ) ;
#10789 =( REPRESENTATION_RELATIONSHIP ('NONE','NONE', #23037, #15767 ) REPRESENTATION_RELATIONSHIP_WITH_TRANSFORMATION ( #26328 )SHAPE_REPRESENTATION_RELATIONSHIP( ) );
#10790 = FACE_OUTER_BOUND ( 'NONE', #32864, .T. ) ;
#10791 = DIRECTION ( 'NONE',  ( 1.000000000000000000, 0.000000000000000000, 0.000000000000000000 ) ) ;
#10792 = EDGE_LOOP ( 'NONE', ( #29215, #838, #13837, #20229 ) ) ;
#10793 = ORIENTED_EDGE ( 'NONE', *, *, #1121, .F. ) ;
#10794 = CARTESIAN_POINT ( 'NONE',  ( -35.00000000000000000, 16.36947364650383818, 36.69637551990492597 ) ) ;
#10795 = CARTESIAN_POINT ( 'NONE',  ( -106.6861857794938544, 4.840548292904078842, 5.731216124222061836 ) ) ;
#10796 = ORIENTED_EDGE ( 'NONE', *, *, #2836, .F. ) ;
#10797 = EDGE_LOOP ( 'NONE', ( #5626, #14014, #22770, #21941 ) ) ;
#10798 = DIRECTION ( 'NONE',  ( -1.000000000000000000, -0.000000000000000000, -0.000000000000000000 ) ) ;
#10799 = AXIS2_PLACEMENT_3D ( 'NONE', #15200, #26044, #22857 ) ;
#10800 = DIRECTION ( 'NONE',  ( 1.000000000000000000, 0.000000000000000000, 1.300283923313630633E-47 ) ) ;
#10801 = DIRECTION ( 'NONE',  ( 0.000000000000000000, 1.000000000000000000, 0.000000000000000000 ) ) ;
#10802 = CARTESIAN_POINT ( 'NONE',  ( 110.7380848894539866, -2.712459438615764475E-14, -7.500000000000241585 ) ) ;
#10803 = VERTEX_POINT ( 'NONE', #27249 ) ;
#10804 = ORIENTED_EDGE ( 'NONE', *, *, #3696, .T. ) ;
#10805 = ORIENTED_EDGE ( 'NONE', *, *, #13468, .F. ) ;
#10806 = CARTESIAN_POINT ( 'NONE',  ( 1.749999999999999778, 0.000000000000000000, 0.000000000000000000 ) ) ;
#10807 = CARTESIAN_POINT ( 'NONE',  ( 145.0000000000000568, 85.49999999999998579, -63.00000000000000000 ) ) ;
#10808 = EDGE_CURVE ( 'NONE', #22671, #17531, #2858, .T. ) ;
#10809 = DIRECTION ( 'NONE',  ( -0.000000000000000000, 0.000000000000000000, 1.000000000000000000 ) ) ;
#10810 = CARTESIAN_POINT ( 'NONE',  ( -442.0000000000000000, -105.0000000000000142, -174.9999999999999716 ) ) ;
#10811 = CARTESIAN_POINT ( 'NONE',  ( -11.99999999999998224, -134.9999999999999716, 155.0000000000000000 ) ) ;
#10812 = DIRECTION ( 'NONE',  ( 0.000000000000000000, -0.08715574274766170471, -0.9961946980917453232 ) ) ;
#10813 = CARTESIAN_POINT ( 'NONE',  ( -35.00000000000000000, -7.062798427011537150, -17.20188834027723246 ) ) ;
#10814 = VERTEX_POINT ( 'NONE', #30101 ) ;
#10815 = EDGE_CURVE ( 'NONE', #2754, #7575, #24565, .T. ) ;
#10816 = LINE ( 'NONE', #21662, #27636 ) ;
#10817 = DIRECTION ( 'NONE',  ( -1.000000000000000000, 0.000000000000000000, 0.000000000000000000 ) ) ;
#10818 = CARTESIAN_POINT ( 'NONE',  ( 0.8418677244542628335, 6.533629441834533758, -13.49999999999999822 ) ) ;
#10819 = ORIENTED_EDGE ( 'NONE', *, *, #6018, .F. ) ;
#10820 = ADVANCED_FACE ( 'NONE', ( #3037 ), #24753, .T. ) ;
#10821 = DIRECTION ( 'NONE',  ( 0.000000000000000000, 0.000000000000000000, -1.000000000000000000 ) ) ;
#10822 = VERTEX_POINT ( 'NONE', #21569 ) ;
#10823 = MANIFOLD_SOLID_BREP ( 'Cut-Extrude1', #11122 ) ;
#10824 = CARTESIAN_POINT ( 'NONE',  ( 2.783107579261526965, 30.38148214875505104, 5.469007969453682172 ) ) ;
#10825 = ADVANCED_FACE ( 'NONE', ( #14974 ), #32408, .T. ) ;
#10826 = CARTESIAN_POINT ( 'NONE',  ( -4.875000000000000000, 2.702098422956710877, 0.000000000000000000 ) ) ;
#10827 = VECTOR ( 'NONE', #17484, 1000.000000000000000 ) ;
#10828 = VERTEX_POINT ( 'NONE', #17650 ) ;
#10829 = DIRECTION ( 'NONE',  ( 0.000000000000000000, 1.000000000000000000, 1.224646799147353207E-16 ) ) ;
#10830 = DIRECTION ( 'NONE',  ( 0.000000000000000000, 1.836970198721029441E-16, -1.000000000000000000 ) ) ;
#10831 = DIRECTION ( 'NONE',  ( -1.000000000000000000, 0.000000000000000000, -0.000000000000000000 ) ) ;
#10832 = EDGE_LOOP ( 'NONE', ( #19160, #23703, #14227, #23497, #14455, #3733, #14424, #30590 ) ) ;
#10833 = VERTEX_POINT ( 'NONE', #20311 ) ;
#10834 = VECTOR ( 'NONE', #8126, 1000.000000000000000 ) ;
#10835 = CARTESIAN_POINT ( 'NONE',  ( 757.3842652136373772, 1333.292759272352669, 1753.598338701303646 ) ) ;
#10836 = LINE ( 'NONE', #8333, #31473 ) ;
#10837 = ORIENTED_EDGE ( 'NONE', *, *, #15005, .T. ) ;
#10838 = DIRECTION ( 'NONE',  ( 0.000000000000000000, 1.836970198721029441E-16, -1.000000000000000000 ) ) ;
#10839 = CARTESIAN_POINT ( 'NONE',  ( -19.99999999999998934, 4.559999999999908127, -172.9900000000000091 ) ) ;
#10840 = LINE ( 'NONE', #15670, #22981 ) ;
#10841 = ORIENTED_EDGE ( 'NONE', *, *, #28427, .F. ) ;
#10842 = ORIENTED_EDGE ( 'NONE', *, *, #34927, .T. ) ;
#10843 = AXIS2_PLACEMENT_3D ( 'NONE', #18785, #29626, #5223 ) ;
#10844 = CARTESIAN_POINT ( 'NONE',  ( -20.00000000000004619, -137.0000000000000000, -162.9999999999999716 ) ) ;
#10845 = AXIS2_PLACEMENT_3D ( 'NONE', #33782, #6883, #9047 ) ;
#10847 = LINE ( 'NONE', #8831, #31751 ) ;
#10846 = CARTESIAN_POINT ( 'NONE',  ( 5.021133111224679091, 26.05646109878476580, -87.50000000000000000 ) ) ;
#10848 = VERTEX_POINT ( 'NONE', #17304 ) ;
#10849 = ORIENTED_EDGE ( 'NONE', *, *, #24691, .T. ) ;
#10850 = FACE_OUTER_BOUND ( 'NONE', #12874, .T. ) ;
#10851 = VERTEX_POINT ( 'NONE', #17121 ) ;
#10852 = DIRECTION ( 'NONE',  ( 1.000000000000000000, 0.000000000000000000, 5.546364386991661285E-52 ) ) ;
#10853 = EDGE_CURVE ( 'NONE', #9458, #10220, #29198, .T. ) ;
#10854 = LINE ( 'NONE', #32734, #1232 ) ;
#10855 = ORIENTED_EDGE ( 'NONE', *, *, #17346, .T. ) ;
#10856 = ORIENTED_EDGE ( 'NONE', *, *, #14589, .T. ) ;
#10857 = CYLINDRICAL_SURFACE ( 'NONE', #28869, 4.000000000000003553 ) ;
#10858 = VECTOR ( 'NONE', #21743, 1000.000000000000000 ) ;
#10859 = EDGE_CURVE ( 'NONE', #3630, #13120, #1945, .T. ) ;
#10860 = ADVANCED_FACE ( 'NONE', ( #17821 ), #23839, .T. ) ;
#10862 = CARTESIAN_POINT ( 'NONE',  ( 0.000000000000000000, 3.524919873834583163E-15, 68.31122994652405112 ) ) ;
#10861 = MECHANICAL_DESIGN_GEOMETRIC_PRESENTATION_REPRESENTATION (  '', ( #5727 ), #18268 ) ;
#10863 = ORIENTED_EDGE ( 'NONE', *, *, #11618, .T. ) ;
#10864 = DIRECTION ( 'NONE',  ( 0.000000000000000000, 1.000000000000000000, -3.374343856708137958E-53 ) ) ;
#10865 = CARTESIAN_POINT ( 'NONE',  ( 2.789999999999999147, 28.29688452313399338, 12.88099432405614309 ) ) ;
#10866 = CARTESIAN_POINT ( 'NONE',  ( -5.021133111225196011, -21.54630831098063481, -87.50000000000000000 ) ) ;
#10867 = DIRECTION ( 'NONE',  ( -1.000000000000000000, 0.000000000000000000, 0.000000000000000000 ) ) ;
#10868 = DIRECTION ( 'NONE',  ( 1.000000000000000000, -0.000000000000000000, 0.000000000000000000 ) ) ;
#10869 = CARTESIAN_POINT ( 'NONE',  ( -20.00000000000007461, 112.9999999999999574, 162.9999999999999716 ) ) ;
#10870 = AXIS2_PLACEMENT_3D ( 'NONE', #4834, #29051, #31551 ) ;
#10871 = EDGE_CURVE ( 'NONE', #9463, #18937, #14126, .T. ) ;
#10872 = AXIS2_PLACEMENT_3D ( 'NONE', #11289, #3607, #957 ) ;
#10873 = VERTEX_POINT ( 'NONE', #12829 ) ;
#10874 = CARTESIAN_POINT ( 'NONE',  ( -345.0000000000000000, 124.9999999999999432, 181.0000000000000000 ) ) ;
#10875 = ORIENTED_EDGE ( 'NONE', *, *, #28074, .T. ) ;
#10877 = VERTEX_POINT ( 'NONE', #4428 ) ;
#10876 = EDGE_CURVE ( 'NONE', #21448, #4640, #10311, .T. ) ;
#10878 = EDGE_CURVE ( 'NONE', #22891, #34395, #7862, .T. ) ;
#10879 = AXIS2_PLACEMENT_3D ( 'NONE', #23328, #1269, #1441 ) ;
#10880 = DIRECTION ( 'NONE',  ( 0.000000000000000000, 0.000000000000000000, 1.000000000000000000 ) ) ;
#10881 = ITEM_DEFINED_TRANSFORMATION ( 'NONE', 'NONE', #32560,  #28566 ) ;
#10882 = AXIS2_PLACEMENT_3D ( 'NONE', #18330, #20804, #20633 ) ;
#10883 = ORIENTED_EDGE ( 'NONE', *, *, #11670, .F. ) ;
#10884 = VECTOR ( 'NONE', #7569, 1000.000000000000000 ) ;
#10885 =( GEOMETRIC_REPRESENTATION_CONTEXT ( 3 ) GLOBAL_UNCERTAINTY_ASSIGNED_CONTEXT ( ( #25307 ) ) GLOBAL_UNIT_ASSIGNED_CONTEXT ( ( #22116, #221, #8406 ) ) REPRESENTATION_CONTEXT ( 'NONE', 'WORKASPACE' ) );
#10886 = CARTESIAN_POINT ( 'NONE',  ( -499.9999999999999432, 144.9999999999999716, 162.9999999999999716 ) ) ;
#10887 = DIRECTION ( 'NONE',  ( -0.000000000000000000, -0.000000000000000000, -1.000000000000000000 ) ) ;
#10888 = EDGE_CURVE ( 'NONE', #28564, #1870, #29393, .T. ) ;
#10889 = ITEM_DEFINED_TRANSFORMATION ( 'NONE', 'NONE', #23521,  #28566 ) ;
#10890 = CARTESIAN_POINT ( 'NONE',  ( -37.12776225901827587, -7.411627343331139706, -36.68877005347593467 ) ) ;
#10891 = VERTEX_POINT ( 'NONE', #1772 ) ;
#10892 = VERTEX_POINT ( 'NONE', #23665 ) ;
#10893 = CYLINDRICAL_SURFACE ( 'NONE', #27070, 16.19999999999999574 ) ;
#10894 = CARTESIAN_POINT ( 'NONE',  ( -442.0000000000000000, -105.0000000000000142, -155.0000000000000000 ) ) ;
#10895 = CARTESIAN_POINT ( 'NONE',  ( -20.02113311122488781, 4.168562732279004202, -67.50000000000000000 ) ) ;
#10896 = FACE_OUTER_BOUND ( 'NONE', #5930, .T. ) ;
#10897 = FACE_OUTER_BOUND ( 'NONE', #21948, .T. ) ;
#10898 = ORIENTED_EDGE ( 'NONE', *, *, #27509, .T. ) ;
#10899 = CIRCLE ( 'NONE', #2930, 30.47050528711511674 ) ;
#10900 = LINE ( 'NONE', #5015, #15197 ) ;
#10901 = CARTESIAN_POINT ( 'NONE',  ( -37.12776225901827587, -7.411627343331159246, 68.31122994652405112 ) ) ;
#10902 = CARTESIAN_POINT ( 'NONE',  ( -365.0000000000000000, -131.0000000000000000, 128.0000000000000000 ) ) ;
#10903 = EDGE_CURVE ( 'NONE', #12420, #19998, #31494, .T. ) ;
#10904 = EDGE_CURVE ( 'NONE', #32472, #6239, #21174, .T. ) ;
#10905 = CARTESIAN_POINT ( 'NONE',  ( -119.9999999999997726, 0.000000000000000000, 0.000000000000000000 ) ) ;
#10906 = CARTESIAN_POINT ( 'NONE',  ( 1.040000000000002922, 34.17636915695680244, -4.045051921974834208 ) ) ;
#10907 = CARTESIAN_POINT ( 'NONE',  ( 2.789999999999999147, 0.000000000000000000, 0.000000000000000000 ) ) ;
#10910 = LINE ( 'NONE', #21591, #348 ) ;
#10909 = LINE ( 'NONE', #32430, #32638 ) ;
#10908 = CIRCLE ( 'NONE', #16052, 0.3000000000000016542 ) ;
#10911 = AXIS2_PLACEMENT_3D ( 'NONE', #30002, #2242, #21994 ) ;
#10912 = LINE ( 'NONE', #10743, #8175 ) ;
#10914 = ORIENTED_EDGE ( 'NONE', *, *, #15451, .T. ) ;
#10913 = VECTOR ( 'NONE', #20101, 1000.000000000000000 ) ;
#10916 = CIRCLE ( 'NONE', #28548, 7.999999999999979572 ) ;
#10915 = DIRECTION ( 'NONE',  ( 0.000000000000000000, 0.000000000000000000, 1.000000000000000000 ) ) ;
#10918 = CARTESIAN_POINT ( 'NONE',  ( 2.765921099433443775, -31.05158812718220673, -1.559667679918931738 ) ) ;
#10917 = DIRECTION ( 'NONE',  ( 0.000000000000000000, 0.000000000000000000, -1.000000000000000000 ) ) ;
#10919 = ORIENTED_EDGE ( 'NONE', *, *, #17828, .F. ) ;
#10920 = LINE ( 'NONE', #32270, #4651 ) ;
#10921 = ORIENTED_EDGE ( 'NONE', *, *, #2101, .T. ) ;
#10922 = EDGE_CURVE ( 'NONE', #16922, #16320, #20996, .T. ) ;
#10923 = EDGE_CURVE ( 'NONE', #15056, #19998, #34010, .T. ) ;
#10924 = VERTEX_POINT ( 'NONE', #31832 ) ;
#10925 = DIRECTION ( 'NONE',  ( 0.000000000000000000, 0.000000000000000000, -1.000000000000000000 ) ) ;
#10926 = ORIENTED_EDGE ( 'NONE', *, *, #20454, .T. ) ;
#10927 = ORIENTED_EDGE ( 'NONE', *, *, #4080, .F. ) ;
#10928 = CARTESIAN_POINT ( 'NONE',  ( 2.765921099433442443, 20.99477179376825120, 22.93149026599753526 ) ) ;
#10929 =( GEOMETRIC_REPRESENTATION_CONTEXT ( 3 ) GLOBAL_UNCERTAINTY_ASSIGNED_CONTEXT ( ( #28468 ) ) GLOBAL_UNIT_ASSIGNED_CONTEXT ( ( #14663, #30490, #31015 ) ) REPRESENTATION_CONTEXT ( 'NONE', 'WORKASPACE' ) );
#10930 = CARTESIAN_POINT ( 'NONE',  ( 1.532562817202168137, 32.50931595846690669, 68.31122994652405112 ) ) ;
#10931 = CIRCLE ( 'NONE', #134, 1.649999999999999911 ) ;
#10932 = DIRECTION ( 'NONE',  ( -0.000000000000000000, 1.000000000000000000, -0.000000000000000000 ) ) ;
#10933 = ORIENTED_EDGE ( 'NONE', *, *, #19299, .T. ) ;
#10934 = VERTEX_POINT ( 'NONE', #23484 ) ;
#10935 = VECTOR ( 'NONE', #14169, 1000.000000000000114 ) ;
#10936 = DIRECTION ( 'NONE',  ( 0.7259954919231316195, 0.6876994588534225405, 1.263283411590315942E-16 ) ) ;
#10937 = EDGE_CURVE ( 'NONE', #29298, #7776, #18347, .T. ) ;
#10938 = CYLINDRICAL_SURFACE ( 'NONE', #15316, 1.999999999999999112 ) ;
#10939 = CARTESIAN_POINT ( 'NONE',  ( 0.000000000000000000, 0.000000000000000000, 0.000000000000000000 ) ) ;
#10940 = ORIENTED_EDGE ( 'NONE', *, *, #7525, .F. ) ;
#10941 = CARTESIAN_POINT ( 'NONE',  ( 15.99999999999998579, 75.55999999999990280, 168.2400000000000091 ) ) ;
#10942 = DIRECTION ( 'NONE',  ( 0.000000000000000000, 1.224646799147353207E-16, -1.000000000000000000 ) ) ;
#10943 = ORIENTED_EDGE ( 'NONE', *, *, #9337, .T. ) ;
#10944 = DIRECTION ( 'NONE',  ( -0.000000000000000000, -0.000000000000000000, 1.000000000000000000 ) ) ;
#10945 = PLANE ( 'NONE',  #5216 ) ;
#10946 = CARTESIAN_POINT ( 'NONE',  ( -2.791255079241054649, -37.75727539589166071, 68.31122994652405112 ) ) ;
#10947 = CARTESIAN_POINT ( 'NONE',  ( 2.789999999999999147, 17.11426446101236820, -26.96776559937708129 ) ) ;
#10948 = CARTESIAN_POINT ( 'NONE',  ( -418.0000000000000000, 113.0000000000000000, -155.0000000000000000 ) ) ;
#10949 = DIRECTION ( 'NONE',  ( 1.000000000000000000, 0.000000000000000000, 0.000000000000000000 ) ) ;
#10950 = VERTEX_POINT ( 'NONE', #9788 ) ;
#10951 = EDGE_CURVE ( 'NONE', #1165, #14972, #12476, .T. ) ;
#10952 = CARTESIAN_POINT ( 'NONE',  ( -8.000000000000000000, 0.000000000000000000, 0.000000000000000000 ) ) ;
#10953 = PRESENTATION_STYLE_ASSIGNMENT (( #21464 ) ) ;
#10954 =( GEOMETRIC_REPRESENTATION_CONTEXT ( 3 ) GLOBAL_UNCERTAINTY_ASSIGNED_CONTEXT ( ( #3895 ) ) GLOBAL_UNIT_ASSIGNED_CONTEXT ( ( #25844, #28859, #1630 ) ) REPRESENTATION_CONTEXT ( 'NONE', 'WORKASPACE' ) );
#10956 = ORIENTED_EDGE ( 'NONE', *, *, #34880, .T. ) ;
#10955 = CIRCLE ( 'NONE', #33689, 0.3000000000000016542 ) ;
#10957 = MECHANICAL_DESIGN_GEOMETRIC_PRESENTATION_REPRESENTATION (  '', ( #17237 ), #31955 ) ;
#10958 = VECTOR ( 'NONE', #2621, 1000.000000000000000 ) ;
#10959 = DIRECTION ( 'NONE',  ( -0.9766205557100866574, -0.2149704402110243218, -3.948942922735925786E-17 ) ) ;
#10960 = CARTESIAN_POINT ( 'NONE',  ( 2.604019721411119370, -31.54566302605122630, -6.854274004868179837 ) ) ;
#10961 = EDGE_CURVE ( 'NONE', #1683, #19066, #20651, .T. ) ;
#10962 = ORIENTED_EDGE ( 'NONE', *, *, #6299, .F. ) ;
#10963 = EDGE_CURVE ( 'NONE', #16672, #12010, #30029, .T. ) ;
#10964 = ADVANCED_FACE ( 'NONE', ( #25808 ), #15675, .T. ) ;
#10965 = VERTEX_POINT ( 'NONE', #31665 ) ;
#10966 = CARTESIAN_POINT ( 'NONE',  ( -365.0000000000000000, -131.0000000000000000, 126.0000000000000000 ) ) ;
#10967 = DIRECTION ( 'NONE',  ( 0.000000000000000000, -1.000000000000000000, 0.000000000000000000 ) ) ;
#10968 = VERTEX_POINT ( 'NONE', #7274 ) ;
#10969 = EDGE_LOOP ( 'NONE', ( #30011, #4591, #31824, #9345 ) ) ;
#10970 = PLANE ( 'NONE',  #13325 ) ;
#10971 = DIRECTION ( 'NONE',  ( -1.000000000000000000, 6.792721752314501023E-48, -3.697785493223492838E-32 ) ) ;
#10972 = CARTESIAN_POINT ( 'NONE',  ( -35.00000000000000000, -4.831299144296466785, 15.81122994652406355 ) ) ;
#10973 = ORIENTED_EDGE ( 'NONE', *, *, #26225, .F. ) ;
#10974 = VERTEX_POINT ( 'NONE', #33997 ) ;
#10975 = CARTESIAN_POINT ( 'NONE',  ( -37.58721499952019940, -4.609089608337739286, -15.81122994652406355 ) ) ;
#10976 = DIRECTION ( 'NONE',  ( -1.000000000000000000, 0.000000000000000000, 0.000000000000000000 ) ) ;
#10977 = CARTESIAN_POINT ( 'NONE',  ( 30.69344702212033127, -10.82204614554912681, 68.31122994652405112 ) ) ;
#10978 = CARTESIAN_POINT ( 'NONE',  ( 0.000000000000000000, 49.99999999999999289, 0.000000000000000000 ) ) ;
#10979 = AXIS2_PLACEMENT_3D ( 'NONE', #26711, #2159, #21386 ) ;
#10980 = DIRECTION ( 'NONE',  ( 1.000000000000000000, 0.000000000000000000, 0.000000000000000000 ) ) ;
#10981 = VECTOR ( 'NONE', #25386, 1000.000000000000000 ) ;
#10982 = CIRCLE ( 'NONE', #29732, 2.033421858999711951 ) ;
#10983 = PLANE ( 'NONE',  #10673 ) ;
#10984 = VECTOR ( 'NONE', #407, 1000.000000000000000 ) ;
#10985 = CARTESIAN_POINT ( 'NONE',  ( 32.81769769215652133, 18.87860345536237006, 68.31122994652405112 ) ) ;
#10986 = ORIENTED_EDGE ( 'NONE', *, *, #3081, .T. ) ;
#10987 = CARTESIAN_POINT ( 'NONE',  ( 1.039999999999999813, 21.72796464722045684, -26.68861566460872226 ) ) ;
#10988 = DIRECTION ( 'NONE',  ( 0.000000000000000000, 0.000000000000000000, 1.000000000000000000 ) ) ;
#10989 = FACE_OUTER_BOUND ( 'NONE', #1189, .T. ) ;
#10990 = EDGE_LOOP ( 'NONE', ( #33255, #32663, #14198, #11508 ) ) ;
#10991 = DIRECTION ( 'NONE',  ( 1.000000000000000000, 0.000000000000000000, 0.000000000000000000 ) ) ;
#10992 = ORIENTED_EDGE ( 'NONE', *, *, #6102, .F. ) ;
#10993 = CARTESIAN_POINT ( 'NONE',  ( 37.55078559520313775, -4.831299144296451686, 49.43553178847298568 ) ) ;
#10994 = DIRECTION ( 'NONE',  ( 1.000000000000000000, 3.469446951953834515E-18, 0.000000000000000000 ) ) ;
#10995 = VECTOR ( 'NONE', #42, 1000.000000000000000 ) ;
#10996 = ORIENTED_EDGE ( 'NONE', *, *, #1707, .F. ) ;
#10997 = EDGE_CURVE ( 'NONE', #13120, #30998, #18174, .T. ) ;
#10998 = DIRECTION ( 'NONE',  ( -0.000000000000000000, 1.000000000000000000, -0.000000000000000000 ) ) ;
#10999 = FACE_OUTER_BOUND ( 'NONE', #24591, .T. ) ;
#11000 = CARTESIAN_POINT ( 'NONE',  ( -355.0000000000000000, -133.0000000000000000, 113.9999999999999858 ) ) ;
#11001 = EDGE_CURVE ( 'NONE', #28629, #10047, #2126, .T. ) ;
#11002 = ORIENTED_EDGE ( 'NONE', *, *, #7283, .T. ) ;
#11003 = AXIS2_PLACEMENT_3D ( 'NONE', #5297, #21159, #7798 ) ;
#11005 = ORIENTED_EDGE ( 'NONE', *, *, #3471, .F. ) ;
#11004 = EDGE_CURVE ( 'NONE', #28476, #2088, #3869, .T. ) ;
#11006 = VECTOR ( 'NONE', #3452, 1000.000000000000000 ) ;
#11007 = CARTESIAN_POINT ( 'NONE',  ( 851.9590526956801568, 1022.204585483647634, 1753.598338701303419 ) ) ;
#11008 = CIRCLE ( 'NONE', #34877, 16.00000000000000000 ) ;
#11009 = DIRECTION ( 'NONE',  ( 0.000000000000000000, -0.5288966977476834419, 0.8486862100397269959 ) ) ;
#11010 = EDGE_CURVE ( 'NONE', #20439, #32701, #9506, .T. ) ;
#11011 = ORIENTED_EDGE ( 'NONE', *, *, #26867, .F. ) ;
#11012 = CARTESIAN_POINT ( 'NONE',  ( -414.0000000000000568, -105.0000000000000142, 132.0000000000000000 ) ) ;
#11013 = CARTESIAN_POINT ( 'NONE',  ( 0.000000000000000000, -45.49999999999999289, 0.000000000000000000 ) ) ;
#11014 = CARTESIAN_POINT ( 'NONE',  ( -20.00000000000001776, -113.0000000000000000, 190.9999999999999716 ) ) ;
#11015 = CARTESIAN_POINT ( 'NONE',  ( -100.0688062106723919, -1.369675690685149050, 7.375755714855094070 ) ) ;
#11016 = CONTEXT_DEPENDENT_SHAPE_REPRESENTATION ( #27617, #33912 ) ;
#11017 = ORIENTED_EDGE ( 'NONE', *, *, #17549, .F. ) ;
#11018 = EDGE_LOOP ( 'NONE', ( #10154, #34627, #2910, #29659 ) ) ;
#11019 = ORIENTED_EDGE ( 'NONE', *, *, #8704, .F. ) ;
#11020 = CARTESIAN_POINT ( 'NONE',  ( -20.00000000000007461, 136.9999999999999432, -155.0000000000000000 ) ) ;
#11021 = ADVANCED_FACE ( 'NONE', ( #21691 ), #16023, .T. ) ;
#11022 = CARTESIAN_POINT ( 'NONE',  ( -499.9999999999999432, 136.9999999999999432, -159.0000000000000000 ) ) ;
#11023 = CARTESIAN_POINT ( 'NONE',  ( -35.00000000000000000, 16.36947364650383818, -36.69637551990492597 ) ) ;
#11024 = ORIENTED_EDGE ( 'NONE', *, *, #2651, .T. ) ;
#11025 = ORIENTED_EDGE ( 'NONE', *, *, #3912, .F. ) ;
#11026 = DIRECTION ( 'NONE',  ( 1.000000000000000000, 0.000000000000000000, 0.000000000000000000 ) ) ;
#11027 = VERTEX_POINT ( 'NONE', #13868 ) ;
#11028 = B_SPLINE_CURVE_WITH_KNOTS ( 'NONE', 3,
 ( #9806, #4799, #2146, #20671 ),
 .UNSPECIFIED., .F., .F.,
 ( 4, 4 ),
 ( 0.005298484651059805900, 0.005985351487543621660 ),
 .UNSPECIFIED. ) ;
#11029 = DIRECTION ( 'NONE',  ( 0.000000000000000000, 0.000000000000000000, 1.000000000000000000 ) ) ;
#11030 = CARTESIAN_POINT ( 'NONE',  ( 9.630725478591894984, 36.62364762272931529, -36.68877005347593467 ) ) ;
#11031 = ORIENTED_EDGE ( 'NONE', *, *, #34846, .F. ) ;
#11032 = PRODUCT_DEFINITION_FORMATION_WITH_SPECIFIED_SOURCE ( 'ANY', '', #27382, .NOT_KNOWN. ) ;
#11033 = ORIENTED_EDGE ( 'NONE', *, *, #6126, .T. ) ;
#11034 = DIRECTION ( 'NONE',  ( 0.000000000000000000, 0.000000000000000000, -1.000000000000000000 ) ) ;
#11035 = AXIS2_PLACEMENT_3D ( 'NONE', #3413, #27800, #33853 ) ;
#11036 = AXIS2_PLACEMENT_3D ( 'NONE', #15833, #24332, #19025 ) ;
#11037 = CARTESIAN_POINT ( 'NONE',  ( -430.0000000000000000, -135.0000000000000000, 126.0000000000000000 ) ) ;
#11038 = ORIENTED_EDGE ( 'NONE', *, *, #30180, .T. ) ;
#11039 = DIRECTION ( 'NONE',  ( -1.000000000000000000, -0.000000000000000000, -0.000000000000000000 ) ) ;
#11041 = CIRCLE ( 'NONE', #12780, 34.41491905851385269 ) ;
#11040 = FACE_OUTER_BOUND ( 'NONE', #34896, .T. ) ;
#11042 = CARTESIAN_POINT ( 'NONE',  ( 0.000000000000000000, 3.524919873834583163E-15, 68.31122994652405112 ) ) ;
#11043 = DIRECTION ( 'NONE',  ( 0.000000000000000000, 1.000000000000000000, 0.000000000000000000 ) ) ;
#11044 =( REPRESENTATION_RELATIONSHIP ('NONE','NONE', #23037, #28231 ) REPRESENTATION_RELATIONSHIP_WITH_TRANSFORMATION ( #5003 )SHAPE_REPRESENTATION_RELATIONSHIP( ) );
#11045 = DIRECTION ( 'NONE',  ( 0.000000000000000000, 0.000000000000000000, 1.000000000000000000 ) ) ;
#11046 = DIRECTION ( 'NONE',  ( 0.6876994588534225405, -0.7259954919231316195, 0.000000000000000000 ) ) ;
#11047 = CARTESIAN_POINT ( 'NONE',  ( 15.99999999999997868, -137.0000000000000000, -155.0000000000000284 ) ) ;
#11048 = VECTOR ( 'NONE', #14538, 1000.000000000000114 ) ;
#11049 = ORIENTED_EDGE ( 'NONE', *, *, #14200, .T. ) ;
#11050 = B_SPLINE_CURVE_WITH_KNOTS ( 'NONE', 3,
 ( #4361, #1537, #31255, #33753 ),
 .UNSPECIFIED., .F., .F.,
 ( 4, 4 ),
 ( 0.005298346101779248009, 0.005985214792935097776 ),
 .UNSPECIFIED. ) ;
#11051 = B_SPLINE_CURVE_WITH_KNOTS ( 'NONE', 3,
 ( #4072, #34338, #18341, #28649 ),
 .UNSPECIFIED., .F., .F.,
 ( 4, 4 ),
 ( 0.005298437004852339476, 0.005985304466813749433 ),
 .UNSPECIFIED. ) ;
#11052 = DIRECTION ( 'NONE',  ( 0.000000000000000000, -1.000000000000000000, -5.145227585319922065E-49 ) ) ;
#11053 =( NAMED_UNIT ( * ) PLANE_ANGLE_UNIT ( ) SI_UNIT ( $, .RADIAN. ) );
#11054 = B_SPLINE_CURVE_WITH_KNOTS ( 'NONE', 3,
 ( #9889, #31598, #18107, #28931 ),
 .UNSPECIFIED., .F., .F.,
 ( 4, 4 ),
 ( 0.005298355823470672979, 0.005985224365431036052 ),
 .UNSPECIFIED. ) ;
#11055 = EDGE_CURVE ( 'NONE', #143, #28422, #11282, .T. ) ;
#11056 = ORIENTED_EDGE ( 'NONE', *, *, #12306, .F. ) ;
#11057 = VECTOR ( 'NONE', #10141, 1000.000000000000227 ) ;
#11058 = ORIENTED_EDGE ( 'NONE', *, *, #16162, .T. ) ;
#11059 = EDGE_CURVE ( 'NONE', #9649, #29470, #13170, .T. ) ;
#11060 = DIRECTION ( 'NONE',  ( 1.000000000000000000, -2.530127506375325948E-80, 1.848892746611746419E-32 ) ) ;
#11061 = VECTOR ( 'NONE', #18022, 1000.000000000000000 ) ;
#11062 = EDGE_CURVE ( 'NONE', #1917, #1130, #13688, .T. ) ;
#11063 = CARTESIAN_POINT ( 'NONE',  ( 102.0965294410245576, 4.962255517573300523, 5.629655879752474057 ) ) ;
#11064 = EDGE_CURVE ( 'NONE', #31361, #6257, #25471, .T. ) ;
#11065 = PRODUCT_CONTEXT ( 'NONE', #27351, 'mechanical' ) ;
#11066 = VERTEX_POINT ( 'NONE', #29711 ) ;
#11067 = LINE ( 'NONE', #32407, #7656 ) ;
#11068 =( NAMED_UNIT ( * ) SI_UNIT ( $, .STERADIAN. ) SOLID_ANGLE_UNIT ( ) );
#11069 = VECTOR ( 'NONE', #14757, 1000.000000000000000 ) ;
#11071 = CYLINDRICAL_SURFACE ( 'NONE', #24917, 16.19999999999999574 ) ;
#11070 = CARTESIAN_POINT ( 'NONE',  ( -23.78520691327551972, 22.21414650552148728, 68.31122994652405112 ) ) ;
#11072 = ORIENTED_EDGE ( 'NONE', *, *, #9911, .T. ) ;
#11073 = ORIENTED_EDGE ( 'NONE', *, *, #8352, .F. ) ;
#11074 = DIRECTION ( 'NONE',  ( -0.5155538571770231782, -0.8568571761675883858, 0.000000000000000000 ) ) ;
#11075 = LINE ( 'NONE', #25596, #6724 ) ;
#11076 = CARTESIAN_POINT ( 'NONE',  ( 6.078604839177343955, 33.69708579775584667, 49.43553178847298568 ) ) ;
#11078 = EDGE_CURVE ( 'NONE', #26400, #28097, #27679, .T. ) ;
#11077 = DIRECTION ( 'NONE',  ( 0.000000000000000000, 1.000000000000000000, 0.000000000000000000 ) ) ;
#11079 = DIRECTION ( 'NONE',  ( 1.000000000000000000, 0.000000000000000000, -0.000000000000000000 ) ) ;
#11080 = VERTEX_POINT ( 'NONE', #30228 ) ;
#11081 = DIRECTION ( 'NONE',  ( -0.4198891015602644883, -0.9075754196709571175, -0.000000000000000000 ) ) ;
#11082 = CARTESIAN_POINT ( 'NONE',  ( 1.749999999999999778, 21.72796464722046039, -26.68861566460872226 ) ) ;
#11083 = AXIS2_PLACEMENT_3D ( 'NONE', #7357, #21606, #18249 ) ;
#11084 = DIRECTION ( 'NONE',  ( 1.000000000000000000, -0.000000000000000000, -0.000000000000000000 ) ) ;
#11085 = VECTOR ( 'NONE', #7069, 1000.000000000000000 ) ;
#11086 = DIRECTION ( 'NONE',  ( 0.000000000000000000, 0.000000000000000000, -1.000000000000000000 ) ) ;
#11087 = ORIENTED_EDGE ( 'NONE', *, *, #16761, .T. ) ;
#11088 = DIRECTION ( 'NONE',  ( 1.000000000000000000, 0.000000000000000000, -0.000000000000000000 ) ) ;
#11090 = LINE ( 'NONE', #22655, #22500 ) ;
#11089 = DIRECTION ( 'NONE',  ( -1.000000000000000000, -0.000000000000000000, -0.000000000000000000 ) ) ;
#11091 = EDGE_CURVE ( 'NONE', #11327, #32902, #32898, .T. ) ;
#11092 = AXIS2_PLACEMENT_3D ( 'NONE', #15510, #4016, #28248 ) ;
#11093 = EDGE_CURVE ( 'NONE', #35009, #31908, #5657, .T. ) ;
#11094 = CARTESIAN_POINT ( 'NONE',  ( -449.9999999999999432, 105.0000000000000142, -175.0000000000000000 ) ) ;
#11095 = ORIENTED_EDGE ( 'NONE', *, *, #6083, .T. ) ;
#11096 = DIRECTION ( 'NONE',  ( 0.000000000000000000, 0.000000000000000000, 1.000000000000000000 ) ) ;
#11098 = CARTESIAN_POINT ( 'NONE',  ( -499.9999999999999432, 104.9999999999999858, -162.9999999999999716 ) ) ;
#11097 = CARTESIAN_POINT ( 'NONE',  ( -499.9999999999999432, 112.9999999999999574, 187.0000000000000000 ) ) ;
#11099 = CLOSED_SHELL ( 'NONE', ( #21470, #4356, #8444, #6650, #25183, #8188, #29310, #19441, #1403, #34762, #10825, #23574, #10119, #21762, #26582, #23268, #15805, #23565, #13258, #15277, #25660, #5812, #21609, #13668, #10166, #7618 ) ) ;
#11100 = ORIENTED_EDGE ( 'NONE', *, *, #33626, .T. ) ;
#11101 = VERTEX_POINT ( 'NONE', #29889 ) ;
#11102 = AXIS2_PLACEMENT_3D ( 'NONE', #13909, #24921, #8553 ) ;
#11103 = ADVANCED_FACE ( 'NONE', ( #24707 ), #16551, .T. ) ;
#11104 = EDGE_CURVE ( 'NONE', #11445, #24518, #10498, .T. ) ;
#11105 = ORIENTED_EDGE ( 'NONE', *, *, #17944, .T. ) ;
#11106 = CARTESIAN_POINT ( 'NONE',  ( -7.218132304338721994, -1.866624223957557893, 5.429999999999999716 ) ) ;
#11107 = B_SPLINE_CURVE_WITH_KNOTS ( 'NONE', 3,
 ( #3633, #26403, #21062, #18074 ),
 .UNSPECIFIED., .F., .F.,
 ( 4, 4 ),
 ( 1.992873153269126117E-07, 0.0006879349942371536155 ),
 .UNSPECIFIED. ) ;
#11108 = ORIENTED_EDGE ( 'NONE', *, *, #32781, .F. ) ;
#11109 = ORIENTED_EDGE ( 'NONE', *, *, #19560, .T. ) ;
#11110 = CARTESIAN_POINT ( 'NONE',  ( 0.000000000000000000, -29.00730259674833178, -9.328884633909240165 ) ) ;
#11111 = VECTOR ( 'NONE', #6150, 1000.000000000000000 ) ;
#11112 = EDGE_CURVE ( 'NONE', #1812, #22871, #19223, .T. ) ;
#11113 = ITEM_DEFINED_TRANSFORMATION ( 'NONE', 'NONE', #27463,  #28566 ) ;
#11114 = DIRECTION ( 'NONE',  ( 1.000000000000000000, 0.000000000000000000, 0.000000000000000000 ) ) ;
#11115 = DIRECTION ( 'NONE',  ( -0.000000000000000000, -5.145227585319922065E-49, -1.000000000000000000 ) ) ;
#11116 = VERTEX_POINT ( 'NONE', #30066 ) ;
#11117 = EDGE_LOOP ( 'NONE', ( #23188, #27557, #9800, #12438, #5691 ) ) ;
#11118 = VECTOR ( 'NONE', #29123, 1000.000000000000000 ) ;
#11119 = CARTESIAN_POINT ( 'NONE',  ( -418.0000000000000000, 105.0000000000000142, -175.0000000000000000 ) ) ;
#11120 = CIRCLE ( 'NONE', #4842, 2.525000000000000355 ) ;
#11121 = CARTESIAN_POINT ( 'NONE',  ( -99.88497961182919482, 6.264093345946821604E-16, 60.00000000000000000 ) ) ;
#11122 = CLOSED_SHELL ( 'NONE', ( #11469, #8223, #1162, #25891, #31386, #10242, #29405, #13232, #33340, #32574, #20577, #30934, #7744, #11329, #8265, #32213, #29610, #16701, #2907, #20856, #32836, #14670, #9606, #16742, #20637, #2766, #33187, #10016, #14324, #17218 ) ) ;
#11123 = CARTESIAN_POINT ( 'NONE',  ( 110.6995658519277725, -0.7644170489479740205, -12.48218521077886400 ) ) ;
#11124 = CARTESIAN_POINT ( 'NONE',  ( -414.0000000000000568, -125.0000000000000000, -101.9999999999999858 ) ) ;
#11125 = ORIENTED_EDGE ( 'NONE', *, *, #34428, .T. ) ;
#11126 = DIRECTION ( 'NONE',  ( 0.000000000000000000, 0.000000000000000000, -1.000000000000000000 ) ) ;
#11127 = CARTESIAN_POINT ( 'NONE',  ( 15.99999999999998579, 144.9999999999999716, -186.9999999999999432 ) ) ;
#11128 = EDGE_LOOP ( 'NONE', ( #29034, #16237, #26499, #28864 ) ) ;
#11129 = FACE_OUTER_BOUND ( 'NONE', #20695, .T. ) ;
#11131 = ADVANCED_FACE ( 'NONE', ( #27383 ), #7811, .F. ) ;
#11130 = LINE ( 'NONE', #21981, #10370 ) ;
#11132 = CARTESIAN_POINT ( 'NONE',  ( 2.265105725890352861, -32.12939361471795507, -9.050569439367922797 ) ) ;
#11133 = ADVANCED_FACE ( 'NONE', ( #15854 ), #26685, .F. ) ;
#11134 = DIRECTION ( 'NONE',  ( -0.000000000000000000, 0.000000000000000000, 1.000000000000000000 ) ) ;
#11135 = ORIENTED_EDGE ( 'NONE', *, *, #11218, .F. ) ;
#11136 = EDGE_CURVE ( 'NONE', #25489, #12065, #16989, .T. ) ;
#11137 = AXIS2_PLACEMENT_3D ( 'NONE', #24662, #300, #27866 ) ;
#11138 = CARTESIAN_POINT ( 'NONE',  ( -70.00000000000000000, 4.559999999999908127, -172.9900000000000091 ) ) ;
#11139 = ORIENTED_EDGE ( 'NONE', *, *, #20900, .F. ) ;
#11140 = LINE ( 'NONE', #33538, #650 ) ;
#11141 = VECTOR ( 'NONE', #8790, 1000.000000000000000 ) ;
#11142 = CARTESIAN_POINT ( 'NONE',  ( -445.9999999999999432, -124.9999999999999858, -77.99999999999997158 ) ) ;
#11143 = EDGE_CURVE ( 'NONE', #11027, #5171, #2469, .T. ) ;
#11144 = EDGE_CURVE ( 'NONE', #32910, #32630, #4934, .T. ) ;
#11145 = EDGE_LOOP ( 'NONE', ( #15185, #4090, #7147, #34207 ) ) ;
#11146 = PLANE ( 'NONE',  #10911 ) ;
#11147 = EDGE_CURVE ( 'NONE', #15752, #30776, #14587, .T. ) ;
#11148 = LINE ( 'NONE', #8809, #675 ) ;
#11149 = VECTOR ( 'NONE', #31685, 1000.000000000000000 ) ;
#11150 = EDGE_LOOP ( 'NONE', ( #34054, #16198, #7748, #18117, #33505, #5553, #23477, #12246 ) ) ;
#11151 = ORIENTED_EDGE ( 'NONE', *, *, #18219, .F. ) ;
#11152 = EDGE_LOOP ( 'NONE', ( #20593, #20199, #14494, #15189 ) ) ;
#11153 = DIRECTION ( 'NONE',  ( 1.000000000000000000, 0.000000000000000000, 0.000000000000000000 ) ) ;
#11154 = CARTESIAN_POINT ( 'NONE',  ( -100.9580106937146837, 3.151985035376890565, 6.811940677030119851 ) ) ;
#11155 = ORIENTED_EDGE ( 'NONE', *, *, #19808, .F. ) ;
#11156 = ORIENTED_EDGE ( 'NONE', *, *, #35061, .F. ) ;
#11157 = CARTESIAN_POINT ( 'NONE',  ( 0.000000000000000000, -3.728217946243090886, 30.24156218513556738 ) ) ;
#11158 = CARTESIAN_POINT ( 'NONE',  ( 1.394999999999999574, 34.10861917999616111, 4.581348211832198203 ) ) ;
#11159 = CIRCLE ( 'NONE', #8296, 32.54542015209057126 ) ;
#11160 = CARTESIAN_POINT ( 'NONE',  ( 2.765921099433442887, -21.56796757982795043, -22.39322359481629476 ) ) ;
#11161 = CARTESIAN_POINT ( 'NONE',  ( 12.00000000000004086, -60.99999999999996447, 155.0000000000000284 ) ) ;
#11162 = ORIENTED_EDGE ( 'NONE', *, *, #22794, .T. ) ;
#11163 = VERTEX_POINT ( 'NONE', #3871 ) ;
#11164 = CARTESIAN_POINT ( 'NONE',  ( 1.040000000000000924, 0.000000000000000000, 0.000000000000000000 ) ) ;
#11165 = LINE ( 'NONE', #29845, #34544 ) ;
#11166 = DIRECTION ( 'NONE',  ( -1.000000000000000000, -0.000000000000000000, -0.000000000000000000 ) ) ;
#11167 = VECTOR ( 'NONE', #34494, 1000.000000000000000 ) ;
#11168 = CYLINDRICAL_SURFACE ( 'NONE', #7982, 4.306175033202026547 ) ;
#11169 = CARTESIAN_POINT ( 'NONE',  ( 145.0000000000000568, -90.42893218813456713, 44.81798139211241505 ) ) ;
#11170 = DIRECTION ( 'NONE',  ( 1.000000000000000000, -0.000000000000000000, -0.000000000000000000 ) ) ;
#11171 = ORIENTED_EDGE ( 'NONE', *, *, #7093, .T. ) ;
#11172 = CARTESIAN_POINT ( 'NONE',  ( -1.307386931792819285, 32.51914993179678959, 68.31122994652405112 ) ) ;
#11173 = DIRECTION ( 'NONE',  ( 0.000000000000000000, 0.000000000000000000, 1.000000000000000000 ) ) ;
#11174 = EDGE_CURVE ( 'NONE', #30882, #30602, #19743, .T. ) ;
#11175 = LINE ( 'NONE', #16881, #20620 ) ;
#11176 = ORIENTED_EDGE ( 'NONE', *, *, #2678, .T. ) ;
#11177 = EDGE_CURVE ( 'NONE', #16061, #21875, #12988, .T. ) ;
#11178 = DIRECTION ( 'NONE',  ( 0.000000000000000000, 1.836970198721029441E-16, -1.000000000000000000 ) ) ;
#11179 = ORIENTED_EDGE ( 'NONE', *, *, #5807, .T. ) ;
#11180 = MANIFOLD_SOLID_BREP ( 'Trim/Extend7[1]', #14934 ) ;
#11181 = FACE_OUTER_BOUND ( 'NONE', #18906, .T. ) ;
#11182 = CARTESIAN_POINT ( 'NONE',  ( -103.6623624504978807, 4.939893293632465543, 11.48260997023825425 ) ) ;
#11183 = AXIS2_PLACEMENT_3D ( 'NONE', #3917, #14981, #9460 ) ;
#11184 = VERTEX_POINT ( 'NONE', #17081 ) ;
#11185 = SHAPE_REPRESENTATION ( 'bearing', ( #28566 ), #10929 ) ;
#11186 = DIRECTION ( 'NONE',  ( 0.000000000000000000, 1.000000000000000000, 1.224646799147353207E-16 ) ) ;
#11187 = CARTESIAN_POINT ( 'NONE',  ( 2.789999999999999147, -13.59935610937992401, 28.90010281771827039 ) ) ;
#11188 = LINE ( 'NONE', #3158, #24550 ) ;
#11189 = VECTOR ( 'NONE', #10241, 1000.000000000000000 ) ;
#11190 = VERTEX_POINT ( 'NONE', #6548 ) ;
#11191 = ORIENTED_EDGE ( 'NONE', *, *, #25667, .T. ) ;
#11192 = DIRECTION ( 'NONE',  ( 0.1063910735369155841, -0.9943243633099125844, -3.335902418025060287E-15 ) ) ;
#11193 = CARTESIAN_POINT ( 'NONE',  ( -9.978866888775527855, 6.201984591278717041, -67.50000000000000000 ) ) ;
#11194 = ORIENTED_EDGE ( 'NONE', *, *, #6463, .T. ) ;
#11195 = TOROIDAL_SURFACE ( 'NONE', #34485, 30.47050528711511674, 8.000000000000000000 ) ;
#11196 = DIRECTION ( 'NONE',  ( -1.000000000000000000, 0.000000000000000000, 0.000000000000000000 ) ) ;
#11197 = DIRECTION ( 'NONE',  ( 0.000000000000000000, 1.836970198721029441E-16, -1.000000000000000000 ) ) ;
#11198 = CARTESIAN_POINT ( 'NONE',  ( -103.6321150747602502, -4.940539628404772898, 5.643550520051347164 ) ) ;
#11199 = VERTEX_POINT ( 'NONE', #3702 ) ;
#11200 = ORIENTED_EDGE ( 'NONE', *, *, #33766, .T. ) ;
#11201 = VERTEX_POINT ( 'NONE', #19567 ) ;
#11202 = PRODUCT ( 'chainlinkage2', 'chainlinkage2', '', ( #13725 ) ) ;
#11203 = DIRECTION ( 'NONE',  ( -0.000000000000000000, -0.000000000000000000, -1.000000000000000000 ) ) ;
#11204 = CIRCLE ( 'NONE', #28801, 3.999999999999976019 ) ;
#11205 = CARTESIAN_POINT ( 'NONE',  ( 0.000000000000000000, 3.524919873834583163E-15, 68.31122994652405112 ) ) ;
#11206 = VECTOR ( 'NONE', #35070, 1000.000000000000114 ) ;
#11207 = CARTESIAN_POINT ( 'NONE',  ( 2.765921099433441110, -27.96208973699912548, 13.59246946040177129 ) ) ;
#11208 = EDGE_LOOP ( 'NONE', ( #24507, #14827, #22333, #28618, #9541, #24273, #13638, #8647 ) ) ;
#11209 = ORIENTED_EDGE ( 'NONE', *, *, #30579, .F. ) ;
#11210 = LINE ( 'NONE', #29716, #33353 ) ;
#11211 = ORIENTED_EDGE ( 'NONE', *, *, #31750, .T. ) ;
#11212 = EDGE_CURVE ( 'NONE', #3836, #12737, #27560, .T. ) ;
#11213 = DIRECTION ( 'NONE',  ( 0.000000000000000000, 0.000000000000000000, 1.000000000000000000 ) ) ;
#11214 = DIRECTION ( 'NONE',  ( -1.292961597001347186E-16, 0.000000000000000000, 1.000000000000000000 ) ) ;
#11215 = ORIENTED_EDGE ( 'NONE', *, *, #30006, .T. ) ;
#11216 = ORIENTED_EDGE ( 'NONE', *, *, #5181, .T. ) ;
#11217 = FACE_OUTER_BOUND ( 'NONE', #31655, .T. ) ;
#11218 = EDGE_CURVE ( 'NONE', #23413, #32949, #8144, .T. ) ;
#11219 = VECTOR ( 'NONE', #8822, 1000.000000000000000 ) ;
#11220 = DIRECTION ( 'NONE',  ( 0.000000000000000000, 1.000000000000000000, -3.374343856708137958E-53 ) ) ;
#11221 = VERTEX_POINT ( 'NONE', #3176 ) ;
#11222 = EDGE_CURVE ( 'NONE', #14883, #25692, #22584, .T. ) ;
#11223 = CARTESIAN_POINT ( 'NONE',  ( -365.0000000000000000, -125.0000000000000284, 168.9999999999999716 ) ) ;
#11224 = DIRECTION ( 'NONE',  ( -1.000000000000000000, 0.000000000000000000, 0.000000000000000000 ) ) ;
#11225 = CARTESIAN_POINT ( 'NONE',  ( 0.000000000000000000, 12.80000000000000071, 0.000000000000000000 ) ) ;
#11226 =( NAMED_UNIT ( * ) PLANE_ANGLE_UNIT ( ) SI_UNIT ( $, .RADIAN. ) );
#11227 = CARTESIAN_POINT ( 'NONE',  ( 2.261199742025449044, -2.866095775113887356, -33.26657006572086317 ) ) ;
#11228 = DIRECTION ( 'NONE',  ( 0.000000000000000000, 0.000000000000000000, 1.000000000000000000 ) ) ;
#11229 = VECTOR ( 'NONE', #32861, 1000.000000000000000 ) ;
#11230 = AXIS2_PLACEMENT_3D ( 'NONE', #24060, #12889, #10373 ) ;
#11231 = ORIENTED_EDGE ( 'NONE', *, *, #28216, .T. ) ;
#11232 = DIRECTION ( 'NONE',  ( 0.000000000000000000, 0.000000000000000000, -1.000000000000000000 ) ) ;
#11233 = DIRECTION ( 'NONE',  ( 0.1063910735368947813, -0.9943243633099144718, -3.335902418024520312E-15 ) ) ;
#11235 = ORIENTED_EDGE ( 'NONE', *, *, #13626, .F. ) ;
#11234 = MANIFOLD_SOLID_BREP ( 'Trim/Extend4[2]', #27017 ) ;
#11236 = VERTEX_POINT ( 'NONE', #1569 ) ;
#11237 = CARTESIAN_POINT ( 'NONE',  ( 100.4793743644694217, 3.553124229080486085, 6.613494096335986505 ) ) ;
#11238 = APPLICATION_PROTOCOL_DEFINITION ( 'draft international standard', 'automotive_design', 1998, #547 ) ;
#11239 = VERTEX_POINT ( 'NONE', #34126 ) ;
#11240 = DIRECTION ( 'NONE',  ( 0.000000000000000000, -1.000000000000000000, 6.123233995736766036E-17 ) ) ;
#11241 = CARTESIAN_POINT ( 'NONE',  ( 26.04754872656010178, -19.51229300245305964, 49.43553178847298568 ) ) ;
#11242 = ITEM_DEFINED_TRANSFORMATION ( 'NONE', 'NONE', #12166,  #28566 ) ;
#11244 = DIRECTION ( 'NONE',  ( 0.3203292411224474279, -0.8039657716618124894, -0.5010271602200255803 ) ) ;
#11243 = CARTESIAN_POINT ( 'NONE',  ( -414.0000000000000568, 137.0000000000000000, -175.0000000000000000 ) ) ;
#11245 = VECTOR ( 'NONE', #29834, 1000.000000000000000 ) ;
#11246 = VERTEX_POINT ( 'NONE', #31802 ) ;
#11247 = VERTEX_POINT ( 'NONE', #12442 ) ;
#11248 = DIRECTION ( 'NONE',  ( -1.000000000000000000, 0.000000000000000000, 0.000000000000000000 ) ) ;
#11249 = CARTESIAN_POINT ( 'NONE',  ( -20.72055270933793736, 25.09707290294328885, 68.31122994652405112 ) ) ;
#11250 = ADVANCED_FACE ( 'NONE', ( #25949 ), #14661, .T. ) ;
#11251 = DIRECTION ( 'NONE',  ( -0.000000000000000000, -0.000000000000000000, 1.000000000000000000 ) ) ;
#11252 = DIRECTION ( 'NONE',  ( 1.000000000000000000, 0.000000000000000000, 0.000000000000000000 ) ) ;
#11253 = CARTESIAN_POINT ( 'NONE',  ( 11.99999999999999645, 144.9999999999999716, 194.9999999999999716 ) ) ;
#11254 = ORIENTED_EDGE ( 'NONE', *, *, #23305, .F. ) ;
#11256 = DIRECTION ( 'NONE',  ( -1.000000000000000000, 6.792721752314501023E-48, -3.697785493223492838E-32 ) ) ;
#11255 = TOROIDAL_SURFACE ( 'NONE', #31151, 15.69999999999999929, 0.3000000000000007661 ) ;
#11258 = DIRECTION ( 'NONE',  ( 1.000000000000000000, 0.000000000000000000, 0.000000000000000000 ) ) ;
#11257 = AXIS2_PLACEMENT_3D ( 'NONE', #21014, #10698, #8365 ) ;
#11259 = CYLINDRICAL_SURFACE ( 'NONE', #4396, 4.750000000000004441 ) ;
#11260 =( REPRESENTATION_RELATIONSHIP ('NONE','NONE', #23037, #15767 ) REPRESENTATION_RELATIONSHIP_WITH_TRANSFORMATION ( #28268 )SHAPE_REPRESENTATION_RELATIONSHIP( ) );
#11261 = ORIENTED_EDGE ( 'NONE', *, *, #33237, .F. ) ;
#11262 = EDGE_CURVE ( 'NONE', #29040, #13030, #3822, .T. ) ;
#11263 = DIRECTION ( 'NONE',  ( 0.000000000000000000, 2.309213040847544338E-50, 1.000000000000000000 ) ) ;
#11264 = DIRECTION ( 'NONE',  ( -1.292961597001347186E-16, -0.000000000000000000, 1.000000000000000000 ) ) ;
#11265 = EDGE_CURVE ( 'NONE', #939, #30843, #27689, .T. ) ;
#11266 = CARTESIAN_POINT ( 'NONE',  ( -442.0000000000000000, -145.0000000000000000, 154.9999999999999716 ) ) ;
#11267 = AXIS2_PLACEMENT_3D ( 'NONE', #26950, #23918, #13265 ) ;
#11269 = CARTESIAN_POINT ( 'NONE',  ( 0.000000000000000000, 16.36473396058513075, -36.68877005347593467 ) ) ;
#11268 = CARTESIAN_POINT ( 'NONE',  ( 0.000000000000000000, -11.69134295108991672, -6.750000000000007105 ) ) ;
#11270 = EDGE_CURVE ( 'NONE', #7307, #29615, #18142, .T. ) ;
#11271 = EDGE_CURVE ( 'NONE', #14020, #25735, #11571, .T. ) ;
#11272 = DIRECTION ( 'NONE',  ( -1.000000000000000000, 0.000000000000000000, 0.000000000000000000 ) ) ;
#11273 = EDGE_LOOP ( 'NONE', ( #12967, #28642, #30383, #17086 ) ) ;
#11274 = DIRECTION ( 'NONE',  ( -0.2149704402110247936, -0.9766205557100865464, -1.794022856297800030E-16 ) ) ;
#11275 = CARTESIAN_POINT ( 'NONE',  ( 0.000000000000000000, 0.000000000000000000, 0.000000000000000000 ) ) ;
#11276 = ADVANCED_FACE ( 'NONE', ( #12788 ), #20611, .F. ) ;
#11277 = CIRCLE ( 'NONE', #25459, 34.41491905851385269 ) ;
#11278 = ORIENTED_EDGE ( 'NONE', *, *, #15682, .F. ) ;
#11279 =( NAMED_UNIT ( * ) PLANE_ANGLE_UNIT ( ) SI_UNIT ( $, .RADIAN. ) );
#11280 = ORIENTED_EDGE ( 'NONE', *, *, #11720, .T. ) ;
#11281 = VECTOR ( 'NONE', #30267, 1000.000000000000000 ) ;
#11282 = CIRCLE ( 'NONE', #24831, 7.999999999999979572 ) ;
#11283 = ORIENTED_EDGE ( 'NONE', *, *, #19340, .T. ) ;
#11284 = LINE ( 'NONE', #19469, #1958 ) ;
#11285 = ORIENTED_EDGE ( 'NONE', *, *, #9137, .T. ) ;
#11286 = ORIENTED_EDGE ( 'NONE', *, *, #31026, .F. ) ;
#11287 = LINE ( 'NONE', #3080, #9929 ) ;
#11288 = CARTESIAN_POINT ( 'NONE',  ( -145.0000000000000568, -167.8552739801376390, -46.75049602362128809 ) ) ;
#11289 = CARTESIAN_POINT ( 'NONE',  ( -19.99999999999998934, -124.9999999999999432, -162.9999999999999432 ) ) ;
#11290 = VERTEX_POINT ( 'NONE', #33961 ) ;
#11291 = ORIENTED_EDGE ( 'NONE', *, *, #32094, .F. ) ;
#11292 = CARTESIAN_POINT ( 'NONE',  ( -12.00000000000001243, 144.9999999999999147, 194.9999999999999716 ) ) ;
#11293 = CARTESIAN_POINT ( 'NONE',  ( -442.0000000000000000, 124.9999999999999574, -190.9999999999999716 ) ) ;
#11294 = CARTESIAN_POINT ( 'NONE',  ( 99.45139749831538722, -1.510413401456684790, -12.41397948795682993 ) ) ;
#11295 = AXIS2_PLACEMENT_3D ( 'NONE', #26868, #16736, #24892 ) ;
#11296 = CARTESIAN_POINT ( 'NONE',  ( 2.765921099433441999, 7.350529080603541487, 30.20932655202940254 ) ) ;
#11297 = EDGE_LOOP ( 'NONE', ( #5879, #31104, #21036, #8422 ) ) ;
#11298 = CARTESIAN_POINT ( 'NONE',  ( 28.23027531293552528, -17.65143121711728469, 20.00000000000000000 ) ) ;
#11299 = AXIS2_PLACEMENT_3D ( 'NONE', #7276, #34701, #1606 ) ;
#11300 = CARTESIAN_POINT ( 'NONE',  ( -441.9999999999999432, -141.0000000000000000, -155.0000000000000000 ) ) ;
#11301 = ORIENTED_EDGE ( 'NONE', *, *, #27716, .F. ) ;
#11302 = LINE ( 'NONE', #32643, #10035 ) ;
#11303 = FACE_BOUND ( 'NONE', #32281, .T. ) ;
#11304 = DIRECTION ( 'NONE',  ( -1.000000000000000000, 0.000000000000000000, 0.000000000000000000 ) ) ;
#11305 = EDGE_CURVE ( 'NONE', #34152, #20441, #7411, .T. ) ;
#11306 = FACE_OUTER_BOUND ( 'NONE', #21612, .T. ) ;
#11307 = ORIENTED_EDGE ( 'NONE', *, *, #30229, .F. ) ;
#11308 = PRESENTATION_LAYER_ASSIGNMENT (  '', '', ( #15869 ) ) ;
#11309 = EDGE_CURVE ( 'NONE', #34117, #30456, #28444, .T. ) ;
#11310 = EDGE_CURVE ( 'NONE', #27322, #32813, #29426, .T. ) ;
#11311 = DIRECTION ( 'NONE',  ( -0.000000000000000000, 1.836970198721029934E-16, -1.000000000000000000 ) ) ;
#11312 = ORIENTED_EDGE ( 'NONE', *, *, #11551, .F. ) ;
#11314 = DIRECTION ( 'NONE',  ( -0.9075754196709575616, 0.4198891015602634891, -0.000000000000000000 ) ) ;
#11313 = DIRECTION ( 'NONE',  ( -0.000000000000000000, 1.000000000000000000, -0.000000000000000000 ) ) ;
#11315 = VECTOR ( 'NONE', #485, 1000.000000000000000 ) ;
#11316 = ORIENTED_EDGE ( 'NONE', *, *, #28690, .T. ) ;
#11317 = CARTESIAN_POINT ( 'NONE',  ( -355.0000000000000000, 116.9999999999999858, 126.0000000000000000 ) ) ;
#11318 = DIRECTION ( 'NONE',  ( -0.000000000000000000, -0.000000000000000000, -1.000000000000000000 ) ) ;
#11319 = ORIENTED_EDGE ( 'NONE', *, *, #15727, .F. ) ;
#11320 = ADVANCED_FACE ( 'NONE', ( #23288 ), #23632, .T. ) ;
#11321 = ORIENTED_EDGE ( 'NONE', *, *, #3704, .T. ) ;
#11322 = VECTOR ( 'NONE', #28051, 1000.000000000000000 ) ;
#11323 = VERTEX_POINT ( 'NONE', #23449 ) ;
#11324 = DIRECTION ( 'NONE',  ( 0.000000000000000000, 0.000000000000000000, -1.000000000000000000 ) ) ;
#11325 = CARTESIAN_POINT ( 'NONE',  ( -442.0000000000000000, -105.0000000000000142, 155.0000000000000568 ) ) ;
#11326 = ORIENTED_EDGE ( 'NONE', *, *, #33540, .F. ) ;
#11327 = VERTEX_POINT ( 'NONE', #23119 ) ;
#11328 = CARTESIAN_POINT ( 'NONE',  ( -35.71762877834949990, -12.58147180936565235, -20.64109601603115607 ) ) ;
#11329 = ADVANCED_FACE ( 'NONE', ( #34306 ), #6888, .F. ) ;
#11330 = ADVANCED_FACE ( 'NONE', ( #10100 ), #18307, .F. ) ;
#11331 = LINE ( 'NONE', #33013, #24391 ) ;
#11332 =( GEOMETRIC_REPRESENTATION_CONTEXT ( 3 ) GLOBAL_UNCERTAINTY_ASSIGNED_CONTEXT ( ( #31933 ) ) GLOBAL_UNIT_ASSIGNED_CONTEXT ( ( #8204, #10543, #11068 ) ) REPRESENTATION_CONTEXT ( 'NONE', 'WORKASPACE' ) );
#11333 = EDGE_CURVE ( 'NONE', #24957, #29500, #12268, .T. ) ;
#11334 = LINE ( 'NONE', #19343, #16337 ) ;
#11335 = LINE ( 'NONE', #10972, #26742 ) ;
#11336 = VERTEX_POINT ( 'NONE', #17616 ) ;
#11337 = ORIENTED_EDGE ( 'NONE', *, *, #1099, .T. ) ;
#11338 = CARTESIAN_POINT ( 'NONE',  ( -418.0000000000000000, -125.0000000000000000, 162.9999999999999716 ) ) ;
#11339 = DIRECTION ( 'NONE',  ( 1.000000000000000000, 0.000000000000000000, 0.000000000000000000 ) ) ;
#11340 = CARTESIAN_POINT ( 'NONE',  ( -20.63749999999999574, 0.000000000000000000, 0.000000000000000000 ) ) ;
#11341 = EDGE_CURVE ( 'NONE', #18446, #29137, #4039, .T. ) ;
#11342 = FACE_OUTER_BOUND ( 'NONE', #28090, .T. ) ;
#11343 = AXIS2_PLACEMENT_3D ( 'NONE', #14197, #25020, #18266 ) ;
#11344 = CARTESIAN_POINT ( 'NONE',  ( 0.5288002580638561101, 14.91106968280097078, -29.87539438830504324 ) ) ;
#11345 = LINE ( 'NONE', #16517, #8938 ) ;
#11346 = FACE_OUTER_BOUND ( 'NONE', #22853, .T. ) ;
#11347 = ORIENTED_EDGE ( 'NONE', *, *, #14332, .T. ) ;
#11348 = CYLINDRICAL_SURFACE ( 'NONE', #4329, 16.19999999999999574 ) ;
#11349 = FACE_OUTER_BOUND ( 'NONE', #7305, .T. ) ;
#11350 = DIRECTION ( 'NONE',  ( 0.000000000000000000, 0.000000000000000000, 1.000000000000000000 ) ) ;
#11351 = ORIENTED_EDGE ( 'NONE', *, *, #8544, .T. ) ;
#11352 = AXIS2_PLACEMENT_3D ( 'NONE', #13439, #20914, #15771 ) ;
#11353 = ADVANCED_FACE ( 'NONE', ( #26820 ), #16159, .F. ) ;
#11354 = DIRECTION ( 'NONE',  ( 1.000000000000000000, 0.000000000000000000, 0.000000000000000000 ) ) ;
#11355 = ORIENTED_EDGE ( 'NONE', *, *, #21891, .T. ) ;
#11356 = DIRECTION ( 'NONE',  ( 1.000000000000000000, 0.000000000000000000, -1.848892746611746966E-32 ) ) ;
#11357 = FACE_OUTER_BOUND ( 'NONE', #5198, .T. ) ;
#11358 = ORIENTED_EDGE ( 'NONE', *, *, #7, .T. ) ;
#11359 = FACE_OUTER_BOUND ( 'NONE', #29395, .T. ) ;
#11360 = CARTESIAN_POINT ( 'NONE',  ( 18.19419936998243870, -33.21164777187627237, 68.31122994652405112 ) ) ;
#11361 = CARTESIAN_POINT ( 'NONE',  ( -445.9999999999999432, -125.0000000000000000, -101.9999999999999858 ) ) ;
#11362 = ORIENTED_EDGE ( 'NONE', *, *, #33677, .F. ) ;
#11363 = DIRECTION ( 'NONE',  ( 2.631201909438060585E-14, -5.396010391056496978E-16, 1.000000000000000000 ) ) ;
#11364 = CARTESIAN_POINT ( 'NONE',  ( 30.98406361983693103, 9.959526819984921175, 68.31122994652405112 ) ) ;
#11365 = VERTEX_POINT ( 'NONE', #27000 ) ;
#11366 = CARTESIAN_POINT ( 'NONE',  ( -12.00000000000001066, 144.9999999999999716, -158.9999999999999716 ) ) ;
#11367 = EDGE_CURVE ( 'NONE', #29615, #1937, #17515, .T. ) ;
#11368 = DIRECTION ( 'NONE',  ( 1.000000000000000000, 0.000000000000000000, 0.000000000000000000 ) ) ;
#11369 = EDGE_CURVE ( 'NONE', #30062, #27991, #21131, .T. ) ;
#11370 = CARTESIAN_POINT ( 'NONE',  ( 11.62236370382047745, -30.39942490923500884, 68.31122994652405112 ) ) ;
#11371 = CARTESIAN_POINT ( 'NONE',  ( -108.3720725006440659, -3.859727759966182781, 6.435874498883202399 ) ) ;
#11372 = EDGE_LOOP ( 'NONE', ( #19791, #18009, #10783, #30053 ) ) ;
#11373 = VERTEX_POINT ( 'NONE', #23963 ) ;
#11374 = VERTEX_POINT ( 'NONE', #29326 ) ;
#11375 = CARTESIAN_POINT ( 'NONE',  ( -418.0000000000000000, -125.0000000000000000, 104.0000000000000142 ) ) ;
#11376 = LINE ( 'NONE', #11739, #18496 ) ;
#11377 = VERTEX_POINT ( 'NONE', #29503 ) ;
#11378 = EDGE_LOOP ( 'NONE', ( #15436, #15630, #12576, #2468 ) ) ;
#11379 = CARTESIAN_POINT ( 'NONE',  ( 1.394999999999999574, -30.02688531850382958, -16.81585001935612667 ) ) ;
#11380 = ORIENTED_EDGE ( 'NONE', *, *, #11265, .F. ) ;
#11381 = CARTESIAN_POINT ( 'NONE',  ( 42.44043929807611448, -20.15143121711728469, 0.000000000000000000 ) ) ;
#11382 = DIRECTION ( 'NONE',  ( 1.000000000000000000, 0.000000000000000000, -1.232595164407831220E-32 ) ) ;
#11383 = ORIENTED_EDGE ( 'NONE', *, *, #19313, .F. ) ;
#11384 = AXIS2_PLACEMENT_3D ( 'NONE', #13558, #18, #10880 ) ;
#11385 = VERTEX_POINT ( 'NONE', #7588 ) ;
#11386 = FACE_OUTER_BOUND ( 'NONE', #5957, .T. ) ;
#11387 = CARTESIAN_POINT ( 'NONE',  ( 2.783107605771416804, 29.25821015115265311, -9.843862221887864195 ) ) ;
#11388 = ORIENTED_EDGE ( 'NONE', *, *, #23713, .T. ) ;
#11389 = CARTESIAN_POINT ( 'NONE',  ( 1.749999999999999778, 0.000000000000000000, 0.000000000000000000 ) ) ;
#11390 = CARTESIAN_POINT ( 'NONE',  ( 2.789999999999999147, -31.68806325674609781, 4.003133335385473224 ) ) ;
#11391 = FACE_BOUND ( 'NONE', #18102, .T. ) ;
#11392 = SURFACE_STYLE_FILL_AREA ( #34104 ) ;
#11393 = CARTESIAN_POINT ( 'NONE',  ( -35.71762877834949990, -12.58147180936565945, 20.64109601603116673 ) ) ;
#11394 = DIRECTION ( 'NONE',  ( 0.3193015301359797276, 0.9476531711828024562, -0.000000000000000000 ) ) ;
#11395 = EDGE_CURVE ( 'NONE', #3900, #18597, #5095, .T. ) ;
#11396 = EDGE_LOOP ( 'NONE', ( #24088, #21088, #29111, #15765 ) ) ;
#11397 = CARTESIAN_POINT ( 'NONE',  ( 840.2028454723844106, 1132.077367791697270, 1753.598338701302964 ) ) ;
#11398 = VECTOR ( 'NONE', #17747, 1000.000000000000000 ) ;
#11399 = VERTEX_POINT ( 'NONE', #27339 ) ;
#11400 = ORIENTED_EDGE ( 'NONE', *, *, #2678, .F. ) ;
#11401 = EDGE_CURVE ( 'NONE', #25432, #15904, #24664, .T. ) ;
#11402 = AXIS2_PLACEMENT_3D ( 'NONE', #9579, #3695, #22756 ) ;
#11403 = EDGE_CURVE ( 'NONE', #4890, #27831, #34845, .T. ) ;
#11404 = CARTESIAN_POINT ( 'NONE',  ( 110.7380848894536598, 7.027127293105233764E-16, 12.50000000000000000 ) ) ;
#11405 = EDGE_CURVE ( 'NONE', #1890, #12838, #10457, .T. ) ;
#11406 = CARTESIAN_POINT ( 'NONE',  ( 99.42172009583602232, 1.358924363732619600, 7.378408734721662476 ) ) ;
#11407 = CONTEXT_DEPENDENT_SHAPE_REPRESENTATION ( #23511, #28272 ) ;
#11408 = ORIENTED_EDGE ( 'NONE', *, *, #12367, .F. ) ;
#11409 = PRODUCT_RELATED_PRODUCT_CATEGORY ( 'part', '', ( #2933 ) ) ;
#11410 = LINE ( 'NONE', #732, #27553 ) ;
#11411 = CARTESIAN_POINT ( 'NONE',  ( -109.4312689855573097, -2.576157761670755164, -12.23490486094944707 ) ) ;
#11412 = CONTEXT_DEPENDENT_SHAPE_REPRESENTATION ( #27409, #17368 ) ;
#11414 = FACE_OUTER_BOUND ( 'NONE', #5731, .T. ) ;
#11413 = DIRECTION ( 'NONE',  ( 0.000000000000000000, 0.000000000000000000, 1.000000000000000000 ) ) ;
#11416 = EDGE_LOOP ( 'NONE', ( #10709, #10662, #6364, #24149 ) ) ;
#11415 = VECTOR ( 'NONE', #9319, 1000.000000000000000 ) ;
#11417 = VERTEX_POINT ( 'NONE', #19005 ) ;
#11418 = CARTESIAN_POINT ( 'NONE',  ( 5.021133111224679091, 28.08988295778447508, -87.50000000000000000 ) ) ;
#11419 = MECHANICAL_DESIGN_GEOMETRIC_PRESENTATION_REPRESENTATION (  '', ( #31848 ), #8002 ) ;
#11420 = CARTESIAN_POINT ( 'NONE',  ( -17.07420202168509604, 33.79163469797341435, 68.31122994652405112 ) ) ;
#11421 = DIRECTION ( 'NONE',  ( 0.000000000000000000, 0.000000000000000000, 1.000000000000000000 ) ) ;
#11422 = CARTESIAN_POINT ( 'NONE',  ( 0.000000000000000000, 0.000000000000000000, 0.000000000000000000 ) ) ;
#11423 = VERTEX_POINT ( 'NONE', #24479 ) ;
#11424 = CARTESIAN_POINT ( 'NONE',  ( -31.87924797510910935, -6.551177101682126747, 68.31122994652405112 ) ) ;
#11425 = DIRECTION ( 'NONE',  ( 0.000000000000000000, 1.836970198721029934E-16, -1.000000000000000000 ) ) ;
#11426 = CYLINDRICAL_SURFACE ( 'NONE', #20847, 2.000000000000001776 ) ;
#11427 = ORIENTED_EDGE ( 'NONE', *, *, #8583, .T. ) ;
#11428 = VECTOR ( 'NONE', #23411, 1000.000000000000114 ) ;
#11429 = CARTESIAN_POINT ( 'NONE',  ( 0.000000000000000000, 6.992329373473909019E-15, 49.43553178847298568 ) ) ;
#11430 = CARTESIAN_POINT ( 'NONE',  ( 2.789999999999999147, -15.32140196853734970, -27.05343472113007763 ) ) ;
#11431 = CIRCLE ( 'NONE', #31315, 2.525000000000003020 ) ;
#11432 = CARTESIAN_POINT ( 'NONE',  ( 29.63313772848249883, -13.45665341906702572, 68.31122994652405112 ) ) ;
#11434 = DIRECTION ( 'NONE',  ( 0.000000000000000000, -2.309213040847544338E-50, -1.000000000000000000 ) ) ;
#11433 = DIRECTION ( 'NONE',  ( -1.000000000000000000, -0.000000000000000000, -0.000000000000000000 ) ) ;
#11435 = CARTESIAN_POINT ( 'NONE',  ( 0.7181323043387224381, -1.866624223957557893, -0.7500000000000000000 ) ) ;
#11436 = ORIENTED_EDGE ( 'NONE', *, *, #5430, .F. ) ;
#11437 = LINE ( 'NONE', #16445, #15621 ) ;
#11438 = DIRECTION ( 'NONE',  ( 0.000000000000000000, 0.000000000000000000, 1.000000000000000000 ) ) ;
#11439 = ORIENTED_EDGE ( 'NONE', *, *, #31763, .F. ) ;
#11440 = AXIS2_PLACEMENT_3D ( 'NONE', #32377, #34709, #21182 ) ;
#11441 = VECTOR ( 'NONE', #21895, 1000.000000000000000 ) ;
#11442 = ADVANCED_FACE ( 'NONE', ( #24140 ), #13353, .F. ) ;
#11443 = CIRCLE ( 'NONE', #18826, 32.54542015209057126 ) ;
#11444 = AXIS2_PLACEMENT_3D ( 'NONE', #13890, #24727, #16041 ) ;
#11445 = VERTEX_POINT ( 'NONE', #302 ) ;
#11446 = ADVANCED_FACE ( 'NONE', ( #29847 ), #13649, .F. ) ;
#11447 = VERTEX_POINT ( 'NONE', #15816 ) ;
#11448 = DIRECTION ( 'NONE',  ( 0.000000000000000000, -0.8486862100397269959, 0.5288966977476833309 ) ) ;
#11449 = VERTEX_POINT ( 'NONE', #26647 ) ;
#11450 = ORIENTED_EDGE ( 'NONE', *, *, #28068, .T. ) ;
#11451 = AXIS2_PLACEMENT_3D ( 'NONE', #27261, #32069, #2701 ) ;
#11452 = ADVANCED_FACE ( 'NONE', ( #32160 ), #2783, .T. ) ;
#11453 = CARTESIAN_POINT ( 'NONE',  ( -5.344999999999999751, 0.000000000000000000, 4.679999999999999716 ) ) ;
#11454 = AXIS2_PLACEMENT_3D ( 'NONE', #31541, #7145, #25676 ) ;
#11455 = ORIENTED_EDGE ( 'NONE', *, *, #25628, .T. ) ;
#11456 = CARTESIAN_POINT ( 'NONE',  ( 35.63428259149704758, -12.79065496477508823, 68.31122994652405112 ) ) ;
#11457 = CARTESIAN_POINT ( 'NONE',  ( -12.00000000000001066, 124.9999999999999716, 155.0000000000000000 ) ) ;
#11458 = ORIENTED_EDGE ( 'NONE', *, *, #18020, .F. ) ;
#11459 = EDGE_CURVE ( 'NONE', #11377, #25387, #7770, .T. ) ;
#11460 = EDGE_LOOP ( 'NONE', ( #33162, #34261, #8467, #31279, #117, #1515 ) ) ;
#11461 = APPLICATION_CONTEXT ( 'automotive_design' ) ;
#11462 = DIRECTION ( 'NONE',  ( -1.000000000000000000, -0.000000000000000000, -0.000000000000000000 ) ) ;
#11463 = CARTESIAN_POINT ( 'NONE',  ( 2.765921099433441555, -0.3931553186911057041, -31.08824725498900676 ) ) ;
#11464 = EDGE_CURVE ( 'NONE', #25758, #26019, #13313, .T. ) ;
#11465 = CARTESIAN_POINT ( 'NONE',  ( -449.9999999999999432, -125.0000000000000000, 162.9999999999999716 ) ) ;
#11466 = DIRECTION ( 'NONE',  ( 1.000000000000000000, 0.000000000000000000, 0.000000000000000000 ) ) ;
#11467 = CARTESIAN_POINT ( 'NONE',  ( 145.0000000000000568, -187.5436536988701732, -180.0000000000000284 ) ) ;
#11468 = ORIENTED_EDGE ( 'NONE', *, *, #11271, .F. ) ;
#11469 = ADVANCED_FACE ( 'NONE', ( #8304 ), #5265, .F. ) ;
#11470 = LINE ( 'NONE', #5409, #19682 ) ;
#11471 = VECTOR ( 'NONE', #25923, 1000.000000000000000 ) ;
#11472 = CARTESIAN_POINT ( 'NONE',  ( 0.02407890056655825201, -3.506335382740311868, -30.89238256715869468 ) ) ;
#11473 = VERTEX_POINT ( 'NONE', #16338 ) ;
#11474 = AXIS2_PLACEMENT_3D ( 'NONE', #33239, #25216, #14393 ) ;
#11475 = VECTOR ( 'NONE', #31958, 1000.000000000000000 ) ;
#11476 = VECTOR ( 'NONE', #16886, 1000.000000000000000 ) ;
#11477 = B_SPLINE_CURVE_WITH_KNOTS ( 'NONE', 3,
 ( #6116, #19852, #30698, #25342, #17018, #14695, #27841, #3447, #14864, #33533, #9149, #6472, #6647, #25698, #12197, #14341, #25519, #17373, #1151, #31561, #28892, #4491, #34763, #32078, #15381, #10026, #12891, #31729, #20537, #18066, #29059, #7337, #10377, #2015, #20882, #7696, #29247, #23375, #1835, #26212, #6995, #23890, #18403, #21232, #9848 ),
 .UNSPECIFIED., .F., .F.,
 ( 4, 2, 2, 2, 2, 2, 2, 2, 2, 2, 1, 2, 2, 2, 2, 2, 2, 2, 2, 2, 2, 2, 4 ),
 ( 3.984693255910324139E-19, 0.001177949164446570477, 0.002355898328893140520, 0.003533847493339711213, 0.004711796657786281907, 0.005889745822232853034, 0.007067694986679424161, 0.007656669568902727506, 0.008245644151126031718, 0.008834618733349335062, 0.009423593315572640142, 0.01001256789779594349, 0.01060154248001924683, 0.01119051706224255191, 0.01177949164446585525, 0.01295744080891246194, 0.01413538997335907210, 0.01531333913780567879, 0.01590231372002897173, 0.01649128830225226466, 0.01708026288447555760, 0.01766923746669885054, 0.01884718663114543988 ),
 .UNSPECIFIED. ) ;
#11478 = DIRECTION ( 'NONE',  ( -1.000000000000000000, 0.000000000000000000, 0.000000000000000000 ) ) ;
#11479 = CARTESIAN_POINT ( 'NONE',  ( -2.791255079241054649, -37.75727539589163939, -36.68877005347593467 ) ) ;
#11480 = DIRECTION ( 'NONE',  ( 1.000000000000000000, 0.000000000000000000, 0.000000000000000000 ) ) ;
#11481 = CARTESIAN_POINT ( 'NONE',  ( 0.7181323043387224381, -1.866624223957557893, 5.429999999999999716 ) ) ;
#11482 = DIRECTION ( 'NONE',  ( 0.2675283385292215321, 0.9635499925192227977, 0.000000000000000000 ) ) ;
#11483 = CARTESIAN_POINT ( 'NONE',  ( 11.99999999999999645, -109.0000000000000142, -155.0000000000000284 ) ) ;
#11484 = VERTEX_POINT ( 'NONE', #27168 ) ;
#11486 = DIRECTION ( 'NONE',  ( 0.000000000000000000, 0.000000000000000000, 1.000000000000000000 ) ) ;
#11485 = FACE_OUTER_BOUND ( 'NONE', #2603, .T. ) ;
#11487 = AXIS2_PLACEMENT_3D ( 'NONE', #3832, #14550, #9374 ) ;
#11488 = ORIENTED_EDGE ( 'NONE', *, *, #14919, .F. ) ;
#11489 = CYLINDRICAL_SURFACE ( 'NONE', #4656, 1.999999999999999112 ) ;
#11490 = PRODUCT_DEFINITION_SHAPE ( 'NONE', 'NONE',  #27721 ) ;
#11491 = LINE ( 'NONE', #24994, #23382 ) ;
#11492 = ORIENTED_EDGE ( 'NONE', *, *, #33441, .T. ) ;
#11493 = ORIENTED_EDGE ( 'NONE', *, *, #13517, .T. ) ;
#11494 = AXIS2_PLACEMENT_3D ( 'NONE', #11361, #14032, #14213 ) ;
#11495 = AXIS2_PLACEMENT_3D ( 'NONE', #30693, #24981, #1148 ) ;
#11496 = VECTOR ( 'NONE', #7600, 1000.000000000000000 ) ;
#11497 = ORIENTED_EDGE ( 'NONE', *, *, #22105, .T. ) ;
#11498 = CARTESIAN_POINT ( 'NONE',  ( 28.11866956577617316, 16.38733641342590985, 68.31122994652405112 ) ) ;
#11499 = DIRECTION ( 'NONE',  ( 0.000000000000000000, 0.000000000000000000, 1.000000000000000000 ) ) ;
#11500 = ORIENTED_EDGE ( 'NONE', *, *, #26670, .F. ) ;
#11501 = ORIENTED_EDGE ( 'NONE', *, *, #2504, .F. ) ;
#11502 = CARTESIAN_POINT ( 'NONE',  ( 30.45781707305797426, -22.50252913745434569, 49.43553178847298568 ) ) ;
#11503 = EDGE_CURVE ( 'NONE', #34660, #16525, #28234, .T. ) ;
#11504 = DIRECTION ( 'NONE',  ( -1.000000000000000000, 0.000000000000000000, -5.546364386991661285E-52 ) ) ;
#11505 = CARTESIAN_POINT ( 'NONE',  ( 0.02407890056655868569, -17.95514392185398833, -25.38201125280375692 ) ) ;
#11506 = FACE_OUTER_BOUND ( 'NONE', #12908, .T. ) ;
#11507 = EDGE_CURVE ( 'NONE', #7193, #14739, #32814, .T. ) ;
#11508 = ORIENTED_EDGE ( 'NONE', *, *, #1691, .T. ) ;
#11509 = EDGE_CURVE ( 'NONE', #19421, #32336, #22600, .T. ) ;
#11510 = ORIENTED_EDGE ( 'NONE', *, *, #15120, .F. ) ;
#11511 = CARTESIAN_POINT ( 'NONE',  ( -6.927285360088501365E-16, 29.09243261715493034, 9.683176917503475423 ) ) ;
#11512 = DIRECTION ( 'NONE',  ( 1.000000000000000000, 3.040835319149746528E-31, 1.232595164407830946E-32 ) ) ;
#11513 = CARTESIAN_POINT ( 'NONE',  ( -345.0000000000000000, -125.0000000000000284, 113.9999999999999858 ) ) ;
#11514 = DIRECTION ( 'NONE',  ( 0.000000000000000000, -1.000000000000000000, -2.132064625830773463E-16 ) ) ;
#11515 = CYLINDRICAL_SURFACE ( 'NONE', #9694, 1.999999999999999112 ) ;
#11516 = CARTESIAN_POINT ( 'NONE',  ( 23.93847777447631131, 22.04889236939138186, 68.31122994652405112 ) ) ;
#11517 =( REPRESENTATION_RELATIONSHIP ('NONE','NONE', #23037, #28231 ) REPRESENTATION_RELATIONSHIP_WITH_TRANSFORMATION ( #6799 )SHAPE_REPRESENTATION_RELATIONSHIP( ) );
#11518 = CARTESIAN_POINT ( 'NONE',  ( -20.00000000000007461, 112.9999999999999574, 190.9999999999999716 ) ) ;
#11519 = EDGE_LOOP ( 'NONE', ( #3533, #25494, #21180, #17939, #31296 ) ) ;
#11520 = DIRECTION ( 'NONE',  ( -1.000000000000000000, 0.000000000000000000, -0.000000000000000000 ) ) ;
#11521 = CARTESIAN_POINT ( 'NONE',  ( 0.02407890056655651728, -3.506335382740735529, 30.89238256715863784 ) ) ;
#11522 = ADVANCED_FACE ( 'NONE', ( #14189 ), #14726, .F. ) ;
#11523 = CIRCLE ( 'NONE', #8100, 1.155000000000000027 ) ;
#11524 = CARTESIAN_POINT ( 'NONE',  ( 0.3923936511923831194, 30.27116788629744804, 13.00174666746672969 ) ) ;
#11525 = ORIENTED_EDGE ( 'NONE', *, *, #3680, .T. ) ;
#11526 = AXIS2_PLACEMENT_3D ( 'NONE', #8533, #14426, #33448 ) ;
#11527 = CIRCLE ( 'NONE', #34824, 16.00000000000000000 ) ;
#11528 = VECTOR ( 'NONE', #22197, 1000.000000000000000 ) ;
#11529 = FACE_OUTER_BOUND ( 'NONE', #19312, .T. ) ;
#11530 = ORIENTED_EDGE ( 'NONE', *, *, #17909, .T. ) ;
#11531 = CARTESIAN_POINT ( 'NONE',  ( -430.0000000000000000, 130.9999999999999716, 109.9999999999999858 ) ) ;
#11532 = CARTESIAN_POINT ( 'NONE',  ( -430.0000000000000000, 118.9999999999999858, 128.0000000000000000 ) ) ;
#11533 = EDGE_CURVE ( 'NONE', #12217, #3404, #16870, .T. ) ;
#11534 = EDGE_CURVE ( 'NONE', #30543, #32722, #19706, .T. ) ;
#11535 = EDGE_CURVE ( 'NONE', #7282, #9737, #8380, .T. ) ;
#11536 = ORIENTED_EDGE ( 'NONE', *, *, #35061, .T. ) ;
#11537 = DIRECTION ( 'NONE',  ( 1.000000000000000000, 0.000000000000000000, 0.000000000000000000 ) ) ;
#11538 = PLANE ( 'NONE',  #17387 ) ;
#11539 = PLANE ( 'NONE',  #16636 ) ;
#11540 = VERTEX_POINT ( 'NONE', #3312 ) ;
#11541 = DIRECTION ( 'NONE',  ( 2.631201909438060585E-14, -5.396010391056496978E-16, 1.000000000000000000 ) ) ;
#11542 = CARTESIAN_POINT ( 'NONE',  ( 19.99999999999998934, 136.9999999999999716, -175.0000000000000284 ) ) ;
#11543 = ORIENTED_EDGE ( 'NONE', *, *, #34671, .T. ) ;
#11544 = DIRECTION ( 'NONE',  ( 0.000000000000000000, 0.000000000000000000, 1.000000000000000000 ) ) ;
#11545 = AXIS2_PLACEMENT_3D ( 'NONE', #19946, #3026, #24913 ) ;
#11546 = VECTOR ( 'NONE', #15603, 1000.000000000000000 ) ;
#11547 = CARTESIAN_POINT ( 'NONE',  ( 2.765921099433441555, 11.80989368511502846, -28.76039115933972923 ) ) ;
#11548 = DIRECTION ( 'NONE',  ( 0.000000000000000000, 0.000000000000000000, 1.000000000000000000 ) ) ;
#11550 = COLOUR_RGB ( '',0.7921568627450980005, 0.8196078431372548767, 0.9333333333333333481 ) ;
#11549 = ITEM_DEFINED_TRANSFORMATION ( 'NONE', 'NONE', #29171,  #28566 ) ;
#11551 = EDGE_CURVE ( 'NONE', #23608, #16235, #652, .T. ) ;
#11552 = ORIENTED_EDGE ( 'NONE', *, *, #20176, .F. ) ;
#11553 = ADVANCED_FACE ( 'NONE', ( #30191 ), #25551, .F. ) ;
#11554 = VERTEX_POINT ( 'NONE', #22364 ) ;
#11555 = VECTOR ( 'NONE', #19111, 1000.000000000000000 ) ;
#11556 = ORIENTED_EDGE ( 'NONE', *, *, #18335, .F. ) ;
#11557 = DIRECTION ( 'NONE',  ( 1.000000000000000000, -0.000000000000000000, -0.000000000000000000 ) ) ;
#11558 = ADVANCED_FACE ( 'NONE', ( #33213 ), #8480, .T. ) ;
#11559 = DIRECTION ( 'NONE',  ( -1.000000000000000000, -0.000000000000000000, -0.000000000000000000 ) ) ;
#11560 = FACE_OUTER_BOUND ( 'NONE', #29571, .T. ) ;
#11561 = ORIENTED_EDGE ( 'NONE', *, *, #34127, .F. ) ;
#11562 = EDGE_LOOP ( 'NONE', ( #18081, #26384, #19547 ) ) ;
#11563 = CARTESIAN_POINT ( 'NONE',  ( 2.789999999999999147, -17.83604598421647935, -24.70480026434183429 ) ) ;
#11564 = ORIENTED_EDGE ( 'NONE', *, *, #29447, .T. ) ;
#11565 = CARTESIAN_POINT ( 'NONE',  ( -37.69926482250235722, 3.578808500140874926, -16.17202516343390428 ) ) ;
#11566 = CARTESIAN_POINT ( 'NONE',  ( 22.10765473302597073, -16.64466345897532307, -87.50000000000000000 ) ) ;
#11567 = ORIENTED_EDGE ( 'NONE', *, *, #14621, .F. ) ;
#11568 = VERTEX_POINT ( 'NONE', #27522 ) ;
#11569 = DIRECTION ( 'NONE',  ( -0.000000000000000000, 1.836970198721029934E-16, -1.000000000000000000 ) ) ;
#11570 = AXIS2_PLACEMENT_3D ( 'NONE', #12013, #17710, #28020 ) ;
#11571 = B_SPLINE_CURVE_WITH_KNOTS ( 'NONE', 3,
 ( #28621, #1395, #15454, #26291 ),
 .UNSPECIFIED., .F., .F.,
 ( 4, 4 ),
 ( 2.122664452422479579E-07, 0.0006879480821238842655 ),
 .UNSPECIFIED. ) ;
#11572 = CARTESIAN_POINT ( 'NONE',  ( 0.000000000000000000, -33.69708579775584667, 49.43553178847298568 ) ) ;
#11573 = ORIENTED_EDGE ( 'NONE', *, *, #28499, .F. ) ;
#11574 = LINE ( 'NONE', #22425, #8959 ) ;
#11575 = LINE ( 'NONE', #19589, #16624 ) ;
#11576 = LINE ( 'NONE', #19591, #26345 ) ;
#11577 = EDGE_CURVE ( 'NONE', #3035, #30605, #19528, .T. ) ;
#11579 = LINE ( 'NONE', #19767, #8871 ) ;
#11578 = AXIS2_PLACEMENT_3D ( 'NONE', #34156, #4069, #20124 ) ;
#11580 = EDGE_CURVE ( 'NONE', #10924, #3997, #1006, .T. ) ;
#11581 = VECTOR ( 'NONE', #32222, 1000.000000000000000 ) ;
#11582 = CARTESIAN_POINT ( 'NONE',  ( -107.2764268663271281, -4.592708079286354383, 11.62653478258734907 ) ) ;
#11583 = DIRECTION ( 'NONE',  ( -0.000000000000000000, 1.000000000000000000, -0.000000000000000000 ) ) ;
#11584 = FACE_OUTER_BOUND ( 'NONE', #32371, .T. ) ;
#11585 = ADVANCED_FACE ( 'NONE', ( #22187 ), #17046, .F. ) ;
#11586 = ORIENTED_EDGE ( 'NONE', *, *, #24252, .T. ) ;
#11587 = EDGE_CURVE ( 'NONE', #17023, #16061, #3484, .T. ) ;
#11588 = ORIENTED_EDGE ( 'NONE', *, *, #19019, .F. ) ;
#11589 = DIRECTION ( 'NONE',  ( 0.1063910735368947813, -0.9943243633099144718, -3.335902418024520312E-15 ) ) ;
#11590 = EDGE_CURVE ( 'NONE', #31738, #1594, #20057, .T. ) ;
#11591 = ORIENTED_EDGE ( 'NONE', *, *, #1064, .F. ) ;
#11592 = ORIENTED_EDGE ( 'NONE', *, *, #26478, .F. ) ;
#11593 = FACE_OUTER_BOUND ( 'NONE', #1749, .T. ) ;
#11594 = AXIS2_PLACEMENT_3D ( 'NONE', #28145, #17134, #6414 ) ;
#11595 = CARTESIAN_POINT ( 'NONE',  ( 101.5015052779749425, 4.562308164568303681, 5.958384794357583836 ) ) ;
#11596 = APPLICATION_PROTOCOL_DEFINITION ( 'draft international standard', 'automotive_design', 1998, #6666 ) ;
#11597 = VERTEX_POINT ( 'NONE', #19883 ) ;
#11598 = CARTESIAN_POINT ( 'NONE',  ( -9.410814080250917257, 36.67205378194064735, 68.31122994652405112 ) ) ;
#11599 =( NAMED_UNIT ( * ) PLANE_ANGLE_UNIT ( ) SI_UNIT ( $, .RADIAN. ) );
#11600 = AXIS2_PLACEMENT_3D ( 'NONE', #20857, #26367, #15711 ) ;
#11602 = DIRECTION ( 'NONE',  ( 0.000000000000000000, 0.000000000000000000, 1.000000000000000000 ) ) ;
#11601 = CARTESIAN_POINT ( 'NONE',  ( 2.789999999999999147, 0.000000000000000000, 0.000000000000000000 ) ) ;
#11603 = VECTOR ( 'NONE', #20674, 1000.000000000000114 ) ;
#11604 = ORIENTED_EDGE ( 'NONE', *, *, #6962, .T. ) ;
#11605 = ORIENTED_EDGE ( 'NONE', *, *, #3030, .T. ) ;
#11606 = AXIS2_PLACEMENT_3D ( 'NONE', #1416, #7084, #33978 ) ;
#11607 = DIRECTION ( 'NONE',  ( -1.000000000000000000, 6.792721752314501023E-48, -3.697785493223492838E-32 ) ) ;
#11608 = EDGE_CURVE ( 'NONE', #904, #28532, #19760, .T. ) ;
#11609 = CYLINDRICAL_SURFACE ( 'NONE', #4503, 16.19999999999999574 ) ;
#11610 = DIRECTION ( 'NONE',  ( 1.000000000000000000, 3.469446951953834515E-18, 0.000000000000000000 ) ) ;
#11611 = CARTESIAN_POINT ( 'NONE',  ( 0.02407890056655608360, -31.05158812718222450, 1.559667679918499417 ) ) ;
#11612 = VERTEX_POINT ( 'NONE', #22726 ) ;
#11613 = DIRECTION ( 'NONE',  ( 3.697785493223492838E-32, 1.934419779023891545E-16, -1.000000000000000000 ) ) ;
#11614 = CARTESIAN_POINT ( 'NONE',  ( 11.99999999999999645, 134.9999999999999432, -162.9999999999999432 ) ) ;
#11615 = CARTESIAN_POINT ( 'NONE',  ( -19.99999999999996092, -137.0000000000000284, 155.0000000000000000 ) ) ;
#11616 = ORIENTED_EDGE ( 'NONE', *, *, #18537, .F. ) ;
#11617 = CARTESIAN_POINT ( 'NONE',  ( -418.0000000000000000, 104.9999999999999858, -187.0000000000000000 ) ) ;
#11618 = EDGE_CURVE ( 'NONE', #9444, #10934, #33561, .T. ) ;
#11619 = FACE_OUTER_BOUND ( 'NONE', #144, .T. ) ;
#11620 = CARTESIAN_POINT ( 'NONE',  ( 1.040000000000000924, 0.000000000000000000, 0.000000000000000000 ) ) ;
#11621 = EDGE_CURVE ( 'NONE', #3870, #14310, #28828, .T. ) ;
#11623 = DIRECTION ( 'NONE',  ( -1.000000000000000000, 0.000000000000000000, 0.000000000000000000 ) ) ;
#11622 = CARTESIAN_POINT ( 'NONE',  ( -345.0000000000000000, 124.9999999999999432, 181.0000000000000000 ) ) ;
#11624 = ADVANCED_FACE ( 'NONE', ( #34264 ), #26078, .T. ) ;
#11625 = LINE ( 'NONE', #6077, #28663 ) ;
#11626 = ORIENTED_EDGE ( 'NONE', *, *, #29825, .F. ) ;
#11627 = CARTESIAN_POINT ( 'NONE',  ( -418.0000000000000000, -104.9999999999999858, -194.9999999999999716 ) ) ;
#11628 = CARTESIAN_POINT ( 'NONE',  ( -365.0000000000000000, 130.9999999999999716, 110.0000000000000000 ) ) ;
#11629 = VECTOR ( 'NONE', #1263, 1000.000000000000000 ) ;
#11630 = PLANE ( 'NONE',  #22110 ) ;
#11632 = ORIENTED_EDGE ( 'NONE', *, *, #6856, .F. ) ;
#11631 = VECTOR ( 'NONE', #6999, 1000.000000000000000 ) ;
#11633 = AXIS2_PLACEMENT_3D ( 'NONE', #13067, #23895, #21238 ) ;
#11634 = VECTOR ( 'NONE', #7628, 1000.000000000000000 ) ;
#11635 = VERTEX_POINT ( 'NONE', #20233 ) ;
#11636 = EDGE_LOOP ( 'NONE', ( #29071, #13902, #19431, #7057 ) ) ;
#11637 = DIRECTION ( 'NONE',  ( -0.000000000000000000, 5.145227585319922065E-49, 1.000000000000000000 ) ) ;
#11638 = ORIENTED_EDGE ( 'NONE', *, *, #18730, .T. ) ;
#11639 = VERTEX_POINT ( 'NONE', #12052 ) ;
#11640 = CARTESIAN_POINT ( 'NONE',  ( -11.83261234297099662, -30.31820670846265742, -36.68877005347593467 ) ) ;
#11641 = ITEM_DEFINED_TRANSFORMATION ( 'NONE', 'NONE', #4156,  #28566 ) ;
#11642 = AXIS2_PLACEMENT_3D ( 'NONE', #20049, #34967, #2376 ) ;
#11643 = EDGE_LOOP ( 'NONE', ( #11455, #31372, #32326, #6304 ) ) ;
#11644 = DIRECTION ( 'NONE',  ( 0.000000000000000000, 1.836970198721029441E-16, -1.000000000000000000 ) ) ;
#11645 = CARTESIAN_POINT ( 'NONE',  ( 22.89764159710611224, 15.60017778382161246, -77.50000000000000000 ) ) ;
#11646 = ORIENTED_EDGE ( 'NONE', *, *, #15353, .F. ) ;
#11647 = VERTEX_POINT ( 'NONE', #9546 ) ;
#11648 = PLANE ( 'NONE',  #31053 ) ;
#11649 = LINE ( 'NONE', #11121, #4987 ) ;
#11650 = CIRCLE ( 'NONE', #15059, 2.033421858999710619 ) ;
#11651 = CARTESIAN_POINT ( 'NONE',  ( 0.000000000000000000, 49.99999999999999289, 0.000000000000000000 ) ) ;
#11652 = DIRECTION ( 'NONE',  ( 0.000000000000000000, 0.000000000000000000, 1.000000000000000000 ) ) ;
#11653 = CARTESIAN_POINT ( 'NONE',  ( -12.00000000000001066, 144.9999999999999716, 190.9999999999999716 ) ) ;
#11654 = ORIENTED_EDGE ( 'NONE', *, *, #21535, .T. ) ;
#11655 = CARTESIAN_POINT ( 'NONE',  ( 19.99999999999998224, 144.9999999999999716, -162.9999999999999432 ) ) ;
#11656 = FACE_OUTER_BOUND ( 'NONE', #26220, .T. ) ;
#11657 = CIRCLE ( 'NONE', #31500, 7.999999999999992895 ) ;
#11658 = CARTESIAN_POINT ( 'NONE',  ( -45.05956070192387841, -32.65143121711728469, 0.000000000000000000 ) ) ;
#11659 = EDGE_LOOP ( 'NONE', ( #20607, #24920, #12100, #29352 ) ) ;
#11660 = AXIS2_PLACEMENT_3D ( 'NONE', #2815, #155, #22579 ) ;
#11661 = LINE ( 'NONE', #8978, #19649 ) ;
#11662 = LINE ( 'NONE', #19674, #24552 ) ;
#11663 = ADVANCED_FACE ( 'NONE', ( #29096 ), #12562, .T. ) ;
#11664 = CARTESIAN_POINT ( 'NONE',  ( -5.038454199367317976, -32.15304576796694391, -36.68877005347593467 ) ) ;
#11665 = CARTESIAN_POINT ( 'NONE',  ( 0.000000000000000000, -23.41952779159748843, -19.49300927180572529 ) ) ;
#11666 = CARTESIAN_POINT ( 'NONE',  ( -36.80830595996284416, 8.862931941313773265, 68.31122994652405112 ) ) ;
#11667 = ADVANCED_FACE ( 'NONE', ( #31248 ), #15069, .F. ) ;
#11668 = CARTESIAN_POINT ( 'NONE',  ( 2.789999999999999147, 5.092684668492570843, 30.01061466292829394 ) ) ;
#11669 = ORIENTED_EDGE ( 'NONE', *, *, #30169, .T. ) ;
#11670 = EDGE_CURVE ( 'NONE', #33546, #21129, #12396, .T. ) ;
#11671 = LINE ( 'NONE', #22521, #33775 ) ;
#11673 = CARTESIAN_POINT ( 'NONE',  ( 0.07094833952453778736, -3.385765165811753352, 31.51266256086713469 ) ) ;
#11672 = CARTESIAN_POINT ( 'NONE',  ( 26.97014235612466493, -26.57093094961043889, 68.31122994652405112 ) ) ;
#11674 = AXIS2_PLACEMENT_3D ( 'NONE', #23192, #6970, #17688 ) ;
#11675 = VERTEX_POINT ( 'NONE', #28409 ) ;
#11676 = DIRECTION ( 'NONE',  ( 3.697785493223492838E-32, 1.934419779023891545E-16, -1.000000000000000000 ) ) ;
#11677 = DIRECTION ( 'NONE',  ( 0.000000000000000000, -1.224646799147353207E-16, 1.000000000000000000 ) ) ;
#11678 = AXIS2_PLACEMENT_3D ( 'NONE', #32332, #18829, #29672 ) ;
#11679 = ADVANCED_FACE ( 'NONE', ( #15410 ), #33408, .T. ) ;
#11680 = ORIENTED_EDGE ( 'NONE', *, *, #19938, .T. ) ;
#11681 = VECTOR ( 'NONE', #28254, 1000.000000000000000 ) ;
#11682 = ORIENTED_EDGE ( 'NONE', *, *, #4109, .T. ) ;
#11683 = PLANE ( 'NONE',  #15674 ) ;
#11684 = ORIENTED_EDGE ( 'NONE', *, *, #28330, .T. ) ;
#11685 = ORIENTED_EDGE ( 'NONE', *, *, #31018, .F. ) ;
#11686 = CARTESIAN_POINT ( 'NONE',  ( 2.789999999999999147, -3.728217946242703196, -30.24156218513559935 ) ) ;
#11687 = CARTESIAN_POINT ( 'NONE',  ( 0.000000000000000000, -27.53147453683434520, 13.05640081644832939 ) ) ;
#11688 = DIRECTION ( 'NONE',  ( -3.469446951953832974E-18, -1.000000000000000000, -7.888609052210116302E-31 ) ) ;
#11689 = CARTESIAN_POINT ( 'NONE',  ( -40.71667869272602758, -14.57327534360751109, 21.88237730393305469 ) ) ;
#11690 = ORIENTED_EDGE ( 'NONE', *, *, #15800, .F. ) ;
#11691 = VERTEX_POINT ( 'NONE', #23409 ) ;
#11692 = CARTESIAN_POINT ( 'NONE',  ( 1.039999999999999147, -33.39989884085096605, 8.296590337300141726 ) ) ;
#11693 = DIRECTION ( 'NONE',  ( -1.000000000000000000, -0.000000000000000000, -0.000000000000000000 ) ) ;
#11694 = CARTESIAN_POINT ( 'NONE',  ( -414.0000000000000568, -137.0000000000000000, -175.0000000000000000 ) ) ;
#11695 = CARTESIAN_POINT ( 'NONE',  ( 2.265105726929532270, -11.05013152551644851, 31.49770363594203104 ) ) ;
#11696 = CYLINDRICAL_SURFACE ( 'NONE', #9719, 16.19999999999999574 ) ;
#11697 = CIRCLE ( 'NONE', #30438, 2.033421858999711951 ) ;
#11698 = CARTESIAN_POINT ( 'NONE',  ( 9.199999999999999289, 7.794228634059932048, -13.49999999999999822 ) ) ;
#11699 = DIRECTION ( 'NONE',  ( 0.000000000000000000, 0.000000000000000000, 1.000000000000000000 ) ) ;
#11700 = ORIENTED_EDGE ( 'NONE', *, *, #16988, .F. ) ;
#11701 = AXIS2_PLACEMENT_3D ( 'NONE', #15026, #25870, #970 ) ;
#11702 = CARTESIAN_POINT ( 'NONE',  ( 2.789999999999999147, 28.52477022197315648, -10.62590764890695283 ) ) ;
#11703 = LINE ( 'NONE', #25382, #31353 ) ;
#11704 = EDGE_CURVE ( 'NONE', #1937, #33546, #18256, .T. ) ;
#11705 = DIRECTION ( 'NONE',  ( 0.000000000000000000, 0.000000000000000000, 1.000000000000000000 ) ) ;
#11706 = VERTEX_POINT ( 'NONE', #17745 ) ;
#11707 = DIRECTION ( 'NONE',  ( 0.000000000000000000, -1.000000000000000000, 0.000000000000000000 ) ) ;
#11708 = ORIENTED_EDGE ( 'NONE', *, *, #10961, .T. ) ;
#11709 = ADVANCED_FACE ( 'NONE', ( #26249 ), #20747, .T. ) ;
#11710 = FILL_AREA_STYLE ('',( #9202 ) ) ;
#11712 = AXIS2_PLACEMENT_3D ( 'NONE', #7298, #28678, #22994 ) ;
#11711 = CARTESIAN_POINT ( 'NONE',  ( -101.8751819073018225, 4.063332493481115471, 11.82279441766105954 ) ) ;
#11713 = EDGE_CURVE ( 'NONE', #31774, #29370, #1598, .T. ) ;
#11714 = ORIENTED_EDGE ( 'NONE', *, *, #10434, .F. ) ;
#11715 = EDGE_CURVE ( 'NONE', #21769, #15766, #12740, .T. ) ;
#11716 = ADVANCED_FACE ( 'NONE', ( #22895 ), #7023, .F. ) ;
#11717 = DIRECTION ( 'NONE',  ( 0.000000000000000000, -5.053935297177146739E-49, -1.000000000000000000 ) ) ;
#11718 = DIRECTION ( 'NONE',  ( -1.000000000000000000, 0.000000000000000000, 0.000000000000000000 ) ) ;
#11719 = CARTESIAN_POINT ( 'NONE',  ( 1.749999999999999778, -18.21166265554766994, -29.20140402659760070 ) ) ;
#11720 = EDGE_CURVE ( 'NONE', #7256, #34152, #33741, .T. ) ;
#11721 = ORIENTED_EDGE ( 'NONE', *, *, #11104, .T. ) ;
#11722 = CARTESIAN_POINT ( 'NONE',  ( 843.6605534792362278, 1099.761843583447671, 1753.598338701303192 ) ) ;
#11723 = CARTESIAN_POINT ( 'NONE',  ( 2.789999999999999147, -9.994970281559535152, 28.75192165143414869 ) ) ;
#11724 = EDGE_LOOP ( 'NONE', ( #27088, #23566, #33815, #8143 ) ) ;
#11725 = AXIS2_PLACEMENT_3D ( 'NONE', #9280, #6417, #31811 ) ;
#11726 = CARTESIAN_POINT ( 'NONE',  ( 1.749999999999999778, 6.183021911002332338, -33.85493898757056286 ) ) ;
#11727 = EDGE_CURVE ( 'NONE', #5950, #28571, #6699, .T. ) ;
#11728 = CARTESIAN_POINT ( 'NONE',  ( 1.749999999999999778, -34.41385771548413430, 0.2702793785568976537 ) ) ;
#11729 = DIRECTION ( 'NONE',  ( 0.000000000000000000, 0.000000000000000000, 1.000000000000000000 ) ) ;
#11730 = CARTESIAN_POINT ( 'NONE',  ( 1.205771365940041528, 7.794228634059941818, 13.49999999999999645 ) ) ;
#11731 = ITEM_DEFINED_TRANSFORMATION ( 'NONE', 'NONE', #22367,  #28566 ) ;
#11732 = ORIENTED_EDGE ( 'NONE', *, *, #16910, .T. ) ;
#11734 = ORIENTED_EDGE ( 'NONE', *, *, #21101, .F. ) ;
#11733 =( REPRESENTATION_RELATIONSHIP ('NONE','NONE', #23037, #28231 ) REPRESENTATION_RELATIONSHIP_WITH_TRANSFORMATION ( #8029 )SHAPE_REPRESENTATION_RELATIONSHIP( ) );
#11735 = EDGE_LOOP ( 'NONE', ( #10099, #24259, #20698, #4583 ) ) ;
#11736 = DIRECTION ( 'NONE',  ( -1.232595164407830946E-32, 0.000000000000000000, -1.000000000000000000 ) ) ;
#11737 = CIRCLE ( 'NONE', #31610, 32.54542015209056416 ) ;
#11738 = DIRECTION ( 'NONE',  ( -1.000000000000000000, -0.000000000000000000, 0.000000000000000000 ) ) ;
#11739 = CARTESIAN_POINT ( 'NONE',  ( -12.00000000000001066, 134.9999999999998863, 155.0000000000000000 ) ) ;
#11740 = CARTESIAN_POINT ( 'NONE',  ( -7.218132304338721994, -1.866624223957557893, -0.7500000000000000000 ) ) ;
#11741 = ORIENTED_EDGE ( 'NONE', *, *, #22707, .T. ) ;
#11742 = CIRCLE ( 'NONE', #935, 7.999999999999979572 ) ;
#11743 = VERTEX_POINT ( 'NONE', #14897 ) ;
#11744 = DIRECTION ( 'NONE',  ( 0.000000000000000000, 1.000000000000000000, 0.000000000000000000 ) ) ;
#11745 = ORIENTED_EDGE ( 'NONE', *, *, #21079, .T. ) ;
#11746 = PRODUCT_DEFINITION_SHAPE ( 'NONE', 'NONE',  #35141 ) ;
#11747 = DIRECTION ( 'NONE',  ( 0.000000000000000000, 1.000000000000000000, 5.053935297177146739E-49 ) ) ;
#11748 = CARTESIAN_POINT ( 'NONE',  ( 104.2406003994089616, 5.690832488206158501, 11.12946004024182933 ) ) ;
#11749 = ORIENTED_EDGE ( 'NONE', *, *, #6943, .T. ) ;
#11750 = ORIENTED_EDGE ( 'NONE', *, *, #25952, .T. ) ;
#11751 = VECTOR ( 'NONE', #25462, 1000.000000000000000 ) ;
#11752 = CARTESIAN_POINT ( 'NONE',  ( 1.040000000000002922, -34.41385771548413430, 0.2702793785568980978 ) ) ;
#11753 = B_SPLINE_CURVE_WITH_KNOTS ( 'NONE', 3,
 ( #12567, #34270, #30905, #20752 ),
 .UNSPECIFIED., .F., .F.,
 ( 4, 4 ),
 ( 1.992873153269112882E-07, 0.0006879349942371712880 ),
 .UNSPECIFIED. ) ;
#11754 = DIRECTION ( 'NONE',  ( 0.000000000000000000, -1.000000000000000000, 0.000000000000000000 ) ) ;
#11755 = ORIENTED_EDGE ( 'NONE', *, *, #3119, .T. ) ;
#11756 = VECTOR ( 'NONE', #23770, 1000.000000000000000 ) ;
#11757 = CYLINDRICAL_SURFACE ( 'NONE', #30000, 5.115020388170798959 ) ;
#11758 = CARTESIAN_POINT ( 'NONE',  ( 0.000000000000000000, -25.77598557799263901, 16.24962337825793313 ) ) ;
#11759 = DIRECTION ( 'NONE',  ( 1.848892746611746419E-32, 6.842277657836020854E-49, -1.000000000000000000 ) ) ;
#11760 = DIRECTION ( 'NONE',  ( -0.9289767198167909745, 0.3701381553399156199, 0.000000000000000000 ) ) ;
#11761 = EDGE_CURVE ( 'NONE', #20902, #22067, #25730, .T. ) ;
#11762 = EDGE_CURVE ( 'NONE', #27942, #14836, #23078, .T. ) ;
#11763 = CARTESIAN_POINT ( 'NONE',  ( -104.3285450821986018, -5.082150419746904291, 11.42046709103397895 ) ) ;
#11764 = DIRECTION ( 'NONE',  ( 1.000000000000000000, 0.000000000000000000, 0.000000000000000000 ) ) ;
#11765 = CARTESIAN_POINT ( 'NONE',  ( 2.765921099433442443, 30.61125888652961891, 5.439165181699118889 ) ) ;
#11766 = VECTOR ( 'NONE', #11314, 1000.000000000000114 ) ;
#11767 = ORIENTED_EDGE ( 'NONE', *, *, #26142, .T. ) ;
#11768 = ORIENTED_EDGE ( 'NONE', *, *, #13434, .T. ) ;
#11769 = CARTESIAN_POINT ( 'NONE',  ( 855.2960651265181014, 989.8772847433134530, 1753.598338701303419 ) ) ;
#11770 = ORIENTED_EDGE ( 'NONE', *, *, #29202, .F. ) ;
#11771 = ORIENTED_EDGE ( 'NONE', *, *, #24983, .T. ) ;
#11772 = CIRCLE ( 'NONE', #31708, 34.41491905851385269 ) ;
#11773 = EDGE_CURVE ( 'NONE', #27137, #33378, #18091, .T. ) ;
#11774 = CARTESIAN_POINT ( 'NONE',  ( -35.00000000000000000, -38.34433698000722046, 36.69637551990492597 ) ) ;
#11775 = CIRCLE ( 'NONE', #2654, 32.54542015209056416 ) ;
#11776 = CARTESIAN_POINT ( 'NONE',  ( 15.99999999999998579, 136.9999999999999716, 155.0000000000000000 ) ) ;
#11777 = ITEM_DEFINED_TRANSFORMATION ( 'NONE', 'NONE', #28591,  #28566 ) ;
#11778 = ORIENTED_EDGE ( 'NONE', *, *, #114, .F. ) ;
#11779 = CARTESIAN_POINT ( 'NONE',  ( -6.500000000000000000, 0.000000000000000000, 0.000000000000000000 ) ) ;
#11780 = CARTESIAN_POINT ( 'NONE',  ( -102.4258224158205763, -4.432411119407283273, -11.68939833797860395 ) ) ;
#11781 = EDGE_CURVE ( 'NONE', #30234, #18803, #34799, .T. ) ;
#11782 = EDGE_CURVE ( 'NONE', #2439, #4511, #31157, .T. ) ;
#11783 = EDGE_CURVE ( 'NONE', #5077, #26849, #29457, .T. ) ;
#11785 = DIRECTION ( 'NONE',  ( -1.232595164407830946E-32, -7.496237820289040735E-63, 1.000000000000000000 ) ) ;
#11784 = CARTESIAN_POINT ( 'NONE',  ( 0.000000000000000000, 0.000000000000000000, -13.49999999999999822 ) ) ;
#11786 = ORIENTED_EDGE ( 'NONE', *, *, #6338, .F. ) ;
#11787 = VERTEX_POINT ( 'NONE', #16114 ) ;
#11788 = DIRECTION ( 'NONE',  ( 0.000000000000000000, 1.000000000000000000, 5.053935297177146739E-49 ) ) ;
#11789 = EDGE_CURVE ( 'NONE', #2476, #769, #32284, .T. ) ;
#11790 = CARTESIAN_POINT ( 'NONE',  ( 2.789999999999999147, 0.000000000000000000, 0.000000000000000000 ) ) ;
#11791 = DIRECTION ( 'NONE',  ( 0.000000000000000000, 1.000000000000000000, -3.374343856708137958E-53 ) ) ;
#11792 = FACE_OUTER_BOUND ( 'NONE', #16310, .T. ) ;
#11793 = VERTEX_POINT ( 'NONE', #21265 ) ;
#11794 = CARTESIAN_POINT ( 'NONE',  ( 145.0000000000000568, -177.8172209610550851, -45.87893859614474223 ) ) ;
#11795 = DIRECTION ( 'NONE',  ( 1.000000000000000000, 0.000000000000000000, 0.000000000000000000 ) ) ;
#11796 = PRODUCT_DEFINITION_SHAPE ( 'NONE', 'NONE',  #13389 ) ;
#11797 = VERTEX_POINT ( 'NONE', #5051 ) ;
#11798 = B_SPLINE_CURVE_WITH_KNOTS ( 'NONE', 3,
 ( #34021, #7475, #18198, #31523, #23514, #29022 ),
 .UNSPECIFIED., .F., .F.,
 ( 4, 2, 4 ),
 ( 2.343813143900254662E-07, 0.001873432713173583302, 0.003746631045032785060 ),
 .UNSPECIFIED. ) ;
#11799 = PLANE ( 'NONE',  #27709 ) ;
#11800 = AXIS2_PLACEMENT_3D ( 'NONE', #13099, #10605, #33801 ) ;
#11801 = DIRECTION ( 'NONE',  ( -1.848892746611746966E-32, 6.842277657836020854E-49, -1.000000000000000000 ) ) ;
#11802 = FACE_OUTER_BOUND ( 'NONE', #14029, .T. ) ;
#11804 = CARTESIAN_POINT ( 'NONE',  ( -418.0000000000000000, -137.0000000000000000, -155.0000000000000000 ) ) ;
#11803 = CARTESIAN_POINT ( 'NONE',  ( -9.410814080250917257, 36.67205378194064735, 68.31122994652405112 ) ) ;
#11805 = CIRCLE ( 'NONE', #7217, 13.50000000000000000 ) ;
#11806 = AXIS2_PLACEMENT_3D ( 'NONE', #20669, #18360, #21187 ) ;
#11807 = EDGE_CURVE ( 'NONE', #27734, #34696, #13608, .T. ) ;
#11808 = UNCERTAINTY_MEASURE_WITH_UNIT (LENGTH_MEASURE( 1.000000000000000082E-05 ), #9432, 'distance_accuracy_value', 'NONE');
#11809 = DIRECTION ( 'NONE',  ( 0.000000000000000000, 2.309213040847544338E-50, 1.000000000000000000 ) ) ;
#11810 = CARTESIAN_POINT ( 'NONE',  ( 0.000000000000000000, 0.000000000000000000, 3.930000000000000160 ) ) ;
#11811 = VERTEX_POINT ( 'NONE', #32113 ) ;
#11812 = DIRECTION ( 'NONE',  ( -0.1617819965527650672, 0.9868265225415261410, 1.812770913216289798E-16 ) ) ;
#11813 = LINE ( 'NONE', #28164, #32483 ) ;
#11814 = VECTOR ( 'NONE', #8122, 1000.000000000000000 ) ;
#11815 = EDGE_LOOP ( 'NONE', ( #13504, #27421, #15013, #10180 ) ) ;
#11816 =( NAMED_UNIT ( * ) SI_UNIT ( $, .STERADIAN. ) SOLID_ANGLE_UNIT ( ) );
#11817 = VECTOR ( 'NONE', #16507, 1000.000000000000000 ) ;
#11818 = ORIENTED_EDGE ( 'NONE', *, *, #34181, .F. ) ;
#11819 = VECTOR ( 'NONE', #26597, 1000.000000000000000 ) ;
#11820 = EDGE_LOOP ( 'NONE', ( #30355, #25087, #21618, #19228 ) ) ;
#11821 = LINE ( 'NONE', #22669, #4764 ) ;
#11822 = ORIENTED_EDGE ( 'NONE', *, *, #17297, .F. ) ;
#11823 = ORIENTED_EDGE ( 'NONE', *, *, #34508, .F. ) ;
#11824 = DIRECTION ( 'NONE',  ( 0.000000000000000000, 0.000000000000000000, -1.000000000000000000 ) ) ;
#11825 = ADVANCED_FACE ( 'NONE', ( #18612 ), #18436, .T. ) ;
#11826 = VECTOR ( 'NONE', #22363, 1000.000000000000000 ) ;
#11827 = ADVANCED_FACE ( 'NONE', ( #21085 ), #29279, .F. ) ;
#11828 = ORIENTED_EDGE ( 'NONE', *, *, #31016, .F. ) ;
#11829 = CARTESIAN_POINT ( 'NONE',  ( -361.0000000000000000, 124.9999999999999432, 181.0000000000000000 ) ) ;
#11830 = DIRECTION ( 'NONE',  ( -0.05413890858541763051, -0.9985334138511239299, -1.834276123671687319E-16 ) ) ;
#11831 = VERTEX_POINT ( 'NONE', #27124 ) ;
#11832 = ORIENTED_EDGE ( 'NONE', *, *, #1100, .F. ) ;
#11833 = LINE ( 'NONE', #16643, #8858 ) ;
#11834 = PLANE ( 'NONE',  #26013 ) ;
#11835 = MANIFOLD_SOLID_BREP ( 'Square tube 40 X 40 X 4(1)[14]', #17781 ) ;
#11836 = DIRECTION ( 'NONE',  ( 1.000000000000000000, 0.000000000000000000, 0.000000000000000000 ) ) ;
#11837 = CARTESIAN_POINT ( 'NONE',  ( -41.91891556802573859, 16.36473396058513785, -36.68877005347594178 ) ) ;
#11838 = LINE ( 'NONE', #11467, #660 ) ;
#11839 = VERTEX_POINT ( 'NONE', #31929 ) ;
#11840 = VECTOR ( 'NONE', #4515, 1000.000000000000000 ) ;
#11841 = DIRECTION ( 'NONE',  ( -0.000000000000000000, 0.5000000000000012212, 0.8660254037844380415 ) ) ;
#11842 = FACE_OUTER_BOUND ( 'NONE', #15543, .T. ) ;
#11843 = ORIENTED_EDGE ( 'NONE', *, *, #21898, .T. ) ;
#11844 = CARTESIAN_POINT ( 'NONE',  ( 15.00000000000000000, 1.836970198721029589E-15, 20.00000000000000000 ) ) ;
#11845 = DIRECTION ( 'NONE',  ( 0.8568571761675904952, -0.5155538571770196254, -0.000000000000000000 ) ) ;
#11846 = DIRECTION ( 'NONE',  ( 0.000000000000000000, 1.836970198721029688E-16, -1.000000000000000000 ) ) ;
#11847 = CARTESIAN_POINT ( 'NONE',  ( -363.0000000000000000, -125.0000000000000284, 168.9999999999999716 ) ) ;
#11848 = CARTESIAN_POINT ( 'NONE',  ( -349.0000000000000000, -125.0000000000000284, 168.9999999999999716 ) ) ;
#11849 = AXIS2_PLACEMENT_3D ( 'NONE', #19659, #18952, #8250 ) ;
#11850 = LINE ( 'NONE', #33535, #3042 ) ;
#11851 = ORIENTED_EDGE ( 'NONE', *, *, #20531, .F. ) ;
#11852 = CARTESIAN_POINT ( 'NONE',  ( 0.000000000000000000, -32.54542015209057126, 87.50000000000000000 ) ) ;
#11854 = CARTESIAN_POINT ( 'NONE',  ( -19.99999999999998934, 134.9999999999999432, -186.9999999999999716 ) ) ;
#11853 = CARTESIAN_POINT ( 'NONE',  ( 2.765921099433441555, 4.286445725888036407, 30.79383171238946204 ) ) ;
#11855 = AXIS2_PLACEMENT_3D ( 'NONE', #7625, #5346, #27032 ) ;
#11856 = ORIENTED_EDGE ( 'NONE', *, *, #8791, .T. ) ;
#11857 = CARTESIAN_POINT ( 'NONE',  ( 11.99999999999999645, -137.0000000000000000, 174.9999999999999432 ) ) ;
#11858 = ORIENTED_EDGE ( 'NONE', *, *, #27755, .T. ) ;
#11859 = ORIENTED_EDGE ( 'NONE', *, *, #28498, .F. ) ;
#11860 = CIRCLE ( 'NONE', #30596, 32.54542015209057126 ) ;
#11861 = EDGE_LOOP ( 'NONE', ( #33079, #26442, #12615, #23525, #32896, #31533 ) ) ;
#11862 = CARTESIAN_POINT ( 'NONE',  ( 106.5437455398453466, -5.539877390153430170, -5.057044031126181061 ) ) ;
#11863 = VERTEX_POINT ( 'NONE', #5404 ) ;
#11864 = ORIENTED_EDGE ( 'NONE', *, *, #32930, .F. ) ;
#11865 = DIRECTION ( 'NONE',  ( -0.000000000000000000, -0.000000000000000000, -1.000000000000000000 ) ) ;
#11866 = EDGE_CURVE ( 'NONE', #23276, #2234, #12970, .T. ) ;
#11867 = AXIS2_PLACEMENT_3D ( 'NONE', #11790, #33654, #31334 ) ;
#11868 = CARTESIAN_POINT ( 'NONE',  ( 2.789999999999999147, 19.87737664170521867, -23.05346671160885563 ) ) ;
#11869 = EDGE_CURVE ( 'NONE', #30622, #18057, #2738, .T. ) ;
#11870 = AXIS2_PLACEMENT_3D ( 'NONE', #16597, #16778, #3219 ) ;
#11871 = DIRECTION ( 'NONE',  ( -1.000000000000000000, -0.000000000000000000, -0.000000000000000000 ) ) ;
#11872 = PLANE ( 'NONE',  #34728 ) ;
#11873 = ORIENTED_EDGE ( 'NONE', *, *, #34265, .F. ) ;
#11874 = ORIENTED_EDGE ( 'NONE', *, *, #23785, .F. ) ;
#11875 = LINE ( 'NONE', #30367, #332 ) ;
#11876 = CARTESIAN_POINT ( 'NONE',  ( -430.0000000000000000, 116.9999999999999716, 113.9999999999999858 ) ) ;
#11877 = ADVANCED_FACE ( 'NONE', ( #75 ), #21441, .F. ) ;
#11878 = DIRECTION ( 'NONE',  ( 0.000000000000000000, 0.000000000000000000, -1.000000000000000000 ) ) ;
#11879 = DIRECTION ( 'NONE',  ( 0.000000000000000000, 1.000000000000000000, 0.000000000000000000 ) ) ;
#11880 = CARTESIAN_POINT ( 'NONE',  ( 0.000000000000000000, -49.99999999999999289, -9.999999999999998224 ) ) ;
#11881 = CARTESIAN_POINT ( 'NONE',  ( 2.789999999999999147, -20.35927063852789232, -22.08513060777193004 ) ) ;
#11882 = FACE_OUTER_BOUND ( 'NONE', #25927, .T. ) ;
#11883 = ORIENTED_EDGE ( 'NONE', *, *, #8772, .F. ) ;
#11884 = DIRECTION ( 'NONE',  ( 0.000000000000000000, 0.000000000000000000, 1.000000000000000000 ) ) ;
#11885 = DIRECTION ( 'NONE',  ( 0.000000000000000000, -1.224646799147353207E-16, 1.000000000000000000 ) ) ;
#11886 = VECTOR ( 'NONE', #28059, 1000.000000000000000 ) ;
#11887 = CARTESIAN_POINT ( 'NONE',  ( -349.0000000000000000, -135.0000000000000000, 109.9999999999999858 ) ) ;
#11888 = ORIENTED_EDGE ( 'NONE', *, *, #31740, .T. ) ;
#11889 = CARTESIAN_POINT ( 'NONE',  ( -365.0000000000000000, 118.9999999999999858, 128.0000000000000000 ) ) ;
#11890 = ORIENTED_EDGE ( 'NONE', *, *, #27850, .T. ) ;
#11891 = LINE ( 'NONE', #14208, #24713 ) ;
#11892 = CARTESIAN_POINT ( 'NONE',  ( -101.6189403138812821, 3.852356953585670318, 11.89405885704113786 ) ) ;
#11893 = AXIS2_PLACEMENT_3D ( 'NONE', #31249, #34090, #14898 ) ;
#11894 = ORIENTED_EDGE ( 'NONE', *, *, #11093, .F. ) ;
#11895 = DIRECTION ( 'NONE',  ( -1.232595164407830946E-32, 0.000000000000000000, -1.000000000000000000 ) ) ;
#11896 = DIRECTION ( 'NONE',  ( 0.000000000000000000, 1.310824597558155437E-49, 1.000000000000000000 ) ) ;
#11897 = CARTESIAN_POINT ( 'NONE',  ( -29.34345171400087793, 14.07715221144536777, -36.68877005347593467 ) ) ;
#11898 = ORIENTED_EDGE ( 'NONE', *, *, #27850, .F. ) ;
#11899 = AXIS2_PLACEMENT_3D ( 'NONE', #27425, #24225, #8554 ) ;
#11900 = DIRECTION ( 'NONE',  ( -0.1063910735369225230, 0.9943243633099118073, -1.000770725407345128E-14 ) ) ;
#11901 = EDGE_CURVE ( 'NONE', #9458, #3870, #11649, .T. ) ;
#11902 = CARTESIAN_POINT ( 'NONE',  ( 1.040000000000000924, 0.000000000000000000, 0.000000000000000000 ) ) ;
#11903 = ORIENTED_EDGE ( 'NONE', *, *, #2611, .F. ) ;
#11904 = PLANE ( 'NONE',  #1918 ) ;
#11905 = EDGE_CURVE ( 'NONE', #20048, #3630, #22684, .T. ) ;
#11906 = AXIS2_PLACEMENT_3D ( 'NONE', #29629, #5226, #34804 ) ;
#11907 = DIRECTION ( 'NONE',  ( 0.000000000000000000, 1.836970198721029441E-16, -1.000000000000000000 ) ) ;
#11908 = DIRECTION ( 'NONE',  ( -1.000000000000000000, -0.000000000000000000, -0.000000000000000000 ) ) ;
#11909 = CARTESIAN_POINT ( 'NONE',  ( 99.26191511054632599, -6.978196330887525654E-16, -12.50000000000000000 ) ) ;
#11910 = ORIENTED_EDGE ( 'NONE', *, *, #10808, .F. ) ;
#11911 = ORIENTED_EDGE ( 'NONE', *, *, #25136, .F. ) ;
#11912 = ORIENTED_EDGE ( 'NONE', *, *, #16108, .T. ) ;
#11913 = EDGE_CURVE ( 'NONE', #13600, #8194, #22623, .T. ) ;
#11914 = DIRECTION ( 'NONE',  ( 1.000000000000000000, 3.469446951953834515E-18, 0.000000000000000000 ) ) ;
#11915 = DIRECTION ( 'NONE',  ( 1.000000000000000000, 0.000000000000000000, 0.000000000000000000 ) ) ;
#11916 = CIRCLE ( 'NONE', #33493, 1.649999999999999911 ) ;
#11917 = FACE_OUTER_BOUND ( 'NONE', #11117, .T. ) ;
#11918 = ORIENTED_EDGE ( 'NONE', *, *, #2677, .T. ) ;
#11919 = ADVANCED_FACE ( 'NONE', ( #8969 ), #3434, .T. ) ;
#11920 = LINE ( 'NONE', #33969, #5489 ) ;
#11921 = DIRECTION ( 'NONE',  ( -1.000000000000000000, 0.000000000000000000, 0.000000000000000000 ) ) ;
#11922 = VERTEX_POINT ( 'NONE', #24801 ) ;
#11923 = CARTESIAN_POINT ( 'NONE',  ( 2.790000000000000924, 1.224646799147353256E-15, -10.00000000000000000 ) ) ;
#11924 = EDGE_CURVE ( 'NONE', #11597, #24095, #601, .T. ) ;
#11925 = CARTESIAN_POINT ( 'NONE',  ( -12.00000000000003908, -134.9999999999999716, -154.9999999999999716 ) ) ;
#11926 = ORIENTED_EDGE ( 'NONE', *, *, #32742, .F. ) ;
#11927 = EDGE_CURVE ( 'NONE', #33325, #31534, #32978, .T. ) ;
#11928 = PRESENTATION_LAYER_ASSIGNMENT (  '', '', ( #30077 ) ) ;
#11929 = ORIENTED_EDGE ( 'NONE', *, *, #28520, .T. ) ;
#11930 = PLANE ( 'NONE',  #25975 ) ;
#11931 = CYLINDRICAL_SURFACE ( 'NONE', #12671, 10.00000000000000000 ) ;
#11932 = VERTEX_POINT ( 'NONE', #30682 ) ;
#11933 = CARTESIAN_POINT ( 'NONE',  ( -20.00000000000004619, 112.9999999999999574, -194.9999999999999432 ) ) ;
#11934 = DIRECTION ( 'NONE',  ( 0.000000000000000000, -1.000000000000000000, 0.000000000000000000 ) ) ;
#11935 = CARTESIAN_POINT ( 'NONE',  ( 31.83311414508813897, -6.771795677801495827, 68.31122994652405112 ) ) ;
#11936 = AXIS2_PLACEMENT_3D ( 'NONE', #8638, #3123, #34033 ) ;
#11937 = CARTESIAN_POINT ( 'NONE',  ( -108.1231672730592095, -4.064293880962485339, 11.82242856119474261 ) ) ;
#11938 = DIRECTION ( 'NONE',  ( 0.000000000000000000, 0.000000000000000000, -1.000000000000000000 ) ) ;
#11939 =( LENGTH_UNIT ( ) NAMED_UNIT ( * ) SI_UNIT ( .MILLI., .METRE. ) );
#11940 = EDGE_LOOP ( 'NONE', ( #7146, #9504, #4754, #13427 ) ) ;
#11941 = AXIS2_PLACEMENT_3D ( 'NONE', #10729, #8396, #21578 ) ;
#11942 = ORIENTED_EDGE ( 'NONE', *, *, #9797, .F. ) ;
#11943 = CARTESIAN_POINT ( 'NONE',  ( 821.1317321780975362, 959.1034997990071815, 1753.598338701302964 ) ) ;
#11944 =( REPRESENTATION_RELATIONSHIP ('NONE','NONE', #23037, #28231 ) REPRESENTATION_RELATIONSHIP_WITH_TRANSFORMATION ( #28963 )SHAPE_REPRESENTATION_RELATIONSHIP( ) );
#11945 = ORIENTED_EDGE ( 'NONE', *, *, #6915, .T. ) ;
#11946 = CARTESIAN_POINT ( 'NONE',  ( 2.765921099433441110, 11.80989368511462523, 28.76039115933989976 ) ) ;
#11947 = LINE ( 'NONE', #20307, #584 ) ;
#11948 = ITEM_DEFINED_TRANSFORMATION ( 'NONE', 'NONE', #31978,  #28566 ) ;
#11949 = ORIENTED_EDGE ( 'NONE', *, *, #2823, .F. ) ;
#11950 = B_SPLINE_CURVE_WITH_KNOTS ( 'NONE', 3,
 ( #11472, #33172, #8976, #3441, #22326, #612 ),
 .UNSPECIFIED., .F., .F.,
 ( 4, 2, 4 ),
 ( 2.011514595355519563E-07, 0.001873399447076926029, 0.003746597742694316585 ),
 .UNSPECIFIED. ) ;
#11951 = PRODUCT_DEFINITION_SHAPE ( 'NONE', 'NONE',  #35243 ) ;
#11952 = FACE_OUTER_BOUND ( 'NONE', #5913, .T. ) ;
#11953 = SURFACE_SIDE_STYLE ('',( #14632 ) ) ;
#11954 = EDGE_CURVE ( 'NONE', #27889, #28881, #25329, .T. ) ;
#11955 = VECTOR ( 'NONE', #32052, 1000.000000000000000 ) ;
#11957 = CARTESIAN_POINT ( 'NONE',  ( -5.210000000000000853, 0.000000000000000000, 0.000000000000000000 ) ) ;
#11956 = CARTESIAN_POINT ( 'NONE',  ( 2.265105755614663874, -18.53613167721979949, 27.76008932203575696 ) ) ;
#11958 = EDGE_LOOP ( 'NONE', ( #1786, #32913 ) ) ;
#11959 = ORIENTED_EDGE ( 'NONE', *, *, #458, .T. ) ;
#11960 = EDGE_CURVE ( 'NONE', #6373, #18937, #1026, .T. ) ;
#11961 = ADVANCED_FACE ( 'NONE', ( #5925 ), #19840, .F. ) ;
#11962 = DIRECTION ( 'NONE',  ( 0.5155538571770216238, -0.8568571761675893850, 0.000000000000000000 ) ) ;
#11963 = PLANE ( 'NONE',  #4430 ) ;
#11964 = CARTESIAN_POINT ( 'NONE',  ( 2.033589655681871111, 33.57753319639237333, -4.776354065834818030 ) ) ;
#11965 = FACE_OUTER_BOUND ( 'NONE', #29026, .T. ) ;
#11966 = ORIENTED_EDGE ( 'NONE', *, *, #33174, .T. ) ;
#11967 = CYLINDRICAL_SURFACE ( 'NONE', #11725, 2.033421858999711507 ) ;
#11968 = CARTESIAN_POINT ( 'NONE',  ( 3.235562306570555532E-30, -11.61907005722761177, -87.50000000000000000 ) ) ;
#11969 = ORIENTED_EDGE ( 'NONE', *, *, #13503, .F. ) ;
#11970 = CARTESIAN_POINT ( 'NONE',  ( -6.500000000000000000, 0.000000000000000000, -0.7500000000000000000 ) ) ;
#11971 = CARTESIAN_POINT ( 'NONE',  ( 0.000000000000000000, 0.000000000000000000, -0.7500000000000000000 ) ) ;
#11972 = EDGE_CURVE ( 'NONE', #33055, #29254, #30854, .T. ) ;
#11973 = DIRECTION ( 'NONE',  ( 1.000000000000000000, 0.000000000000000000, 0.000000000000000000 ) ) ;
#11975 = DIRECTION ( 'NONE',  ( -0.3193015301359803382, -0.9476531711828023452, 0.000000000000000000 ) ) ;
#11974 = DIRECTION ( 'NONE',  ( 0.000000000000000000, -7.888609052210118054E-31, -1.000000000000000000 ) ) ;
#11976 = DIRECTION ( 'NONE',  ( -0.000000000000000000, -0.000000000000000000, -1.000000000000000000 ) ) ;
#11977 = CARTESIAN_POINT ( 'NONE',  ( 1.224646799147352862E-15, 49.99999999999999289, 9.999999999999998224 ) ) ;
#11978 = ORIENTED_EDGE ( 'NONE', *, *, #16537, .F. ) ;
#11979 = DIRECTION ( 'NONE',  ( -0.9868265225415260300, -0.1617819965527650394, 0.000000000000000000 ) ) ;
#11980 = ADVANCED_FACE ( 'NONE', ( #2906 ), #27653, .T. ) ;
#11981 = EDGE_CURVE ( 'NONE', #18461, #32452, #16468, .T. ) ;
#11982 = ORIENTED_EDGE ( 'NONE', *, *, #5654, .T. ) ;
#11983 = EDGE_CURVE ( 'NONE', #32630, #32910, #3850, .T. ) ;
#11984 = EDGE_CURVE ( 'NONE', #509, #34660, #27247, .T. ) ;
#11985 = ORIENTED_EDGE ( 'NONE', *, *, #24378, .T. ) ;
#11986 = VECTOR ( 'NONE', #9591, 1000.000000000000000 ) ;
#11987 = AXIS2_PLACEMENT_3D ( 'NONE', #6866, #31437, #23266 ) ;
#11988 = VERTEX_POINT ( 'NONE', #30143 ) ;
#11989 = DIRECTION ( 'NONE',  ( 0.000000000000000000, 0.000000000000000000, -1.000000000000000000 ) ) ;
#11990 = ORIENTED_EDGE ( 'NONE', *, *, #28529, .F. ) ;
#11991 = ORIENTED_EDGE ( 'NONE', *, *, #10170, .F. ) ;
#11992 = DIRECTION ( 'NONE',  ( 0.000000000000000000, 1.000000000000000000, 1.836970198721029688E-16 ) ) ;
#11993 = ORIENTED_EDGE ( 'NONE', *, *, #30244, .F. ) ;
#11994 = CARTESIAN_POINT ( 'NONE',  ( 11.99999999999995559, -134.9999999999999716, -162.9999999999999432 ) ) ;
#11995 = DIRECTION ( 'NONE',  ( 0.000000000000000000, 0.000000000000000000, 1.000000000000000000 ) ) ;
#11996 = ORIENTED_EDGE ( 'NONE', *, *, #30431, .F. ) ;
#11997 = ORIENTED_EDGE ( 'NONE', *, *, #24859, .F. ) ;
#11998 = EDGE_CURVE ( 'NONE', #8062, #13770, #24972, .T. ) ;
#11999 = ADVANCED_FACE ( 'NONE', ( #8781, #19664 ), #11834, .F. ) ;
#12000 = DIRECTION ( 'NONE',  ( 0.000000000000000000, 0.000000000000000000, 1.000000000000000000 ) ) ;
#12001 = CARTESIAN_POINT ( 'NONE',  ( 0.7564103345238918363, -29.97226545381531082, 15.87222719455781750 ) ) ;
#12002 = CARTESIAN_POINT ( 'NONE',  ( -1.307386931792819285, 32.51914993179681090, -36.68877005347593467 ) ) ;
#12003 = CARTESIAN_POINT ( 'NONE',  ( -6.500000000000000000, 0.000000000000000000, 3.930000000000000160 ) ) ;
#12004 = CYLINDRICAL_SURFACE ( 'NONE', #22813, 14.20000000000000107 ) ;
#12005 = ORIENTED_EDGE ( 'NONE', *, *, #22191, .T. ) ;
#12006 = CIRCLE ( 'NONE', #17143, 4.309328216469825001 ) ;
#12007 = DIRECTION ( 'NONE',  ( 1.232595164407830946E-32, 0.000000000000000000, 1.000000000000000000 ) ) ;
#12008 = CARTESIAN_POINT ( 'NONE',  ( -361.0000000000000000, -125.0000000000000284, 110.0000000000000000 ) ) ;
#12009 = CARTESIAN_POINT ( 'NONE',  ( 2.789999999999999147, 4.286445725888036407, 30.79383171238946204 ) ) ;
#12010 = VERTEX_POINT ( 'NONE', #13968 ) ;
#12011 = DIRECTION ( 'NONE',  ( 1.000000000000000000, 0.000000000000000000, 0.000000000000000000 ) ) ;
#12012 = CARTESIAN_POINT ( 'NONE',  ( 0.008463494849040043358, -26.25524549613186309, -16.27432041257312179 ) ) ;
#12013 = CARTESIAN_POINT ( 'NONE',  ( 11.99999999999999645, 144.9999999999999716, -162.9999999999999432 ) ) ;
#12014 = DIRECTION ( 'NONE',  ( 1.000000000000000000, 0.000000000000000000, 0.000000000000000000 ) ) ;
#12016 = DIRECTION ( 'NONE',  ( -0.000000000000000000, -0.000000000000000000, -1.000000000000000000 ) ) ;
#12015 = CARTESIAN_POINT ( 'NONE',  ( -12.00000000000003908, -134.9999999999999716, -194.9999999999999432 ) ) ;
#12017 = VECTOR ( 'NONE', #32943, 1000.000000000000000 ) ;
#12018 = CIRCLE ( 'NONE', #31331, 10.00000000000000000 ) ;
#12019 = LINE ( 'NONE', #17551, #18416 ) ;
#12021 = ORIENTED_EDGE ( 'NONE', *, *, #15033, .T. ) ;
#12020 = CIRCLE ( 'NONE', #31870, 5.115020388170798959 ) ;
#12022 = B_SPLINE_CURVE_WITH_KNOTS ( 'NONE', 3,
 ( #34401, #5702, #14099, #19272, #16782, #27610 ),
 .UNSPECIFIED., .F., .F.,
 ( 4, 2, 4 ),
 ( 4.404817168184892227E-07, 0.001874269729529006020, 0.003748098977341193273 ),
 .UNSPECIFIED. ) ;
#12023 = DIRECTION ( 'NONE',  ( -0.000000000000000000, -0.000000000000000000, -1.000000000000000000 ) ) ;
#12025 = CARTESIAN_POINT ( 'NONE',  ( -445.9999999999999432, 104.9999999999999858, -162.9999999999999716 ) ) ;
#12024 = CARTESIAN_POINT ( 'NONE',  ( 2.719010729300724627, 26.43944202223378426, -17.47857661787091743 ) ) ;
#12026 = ADVANCED_FACE ( 'NONE', ( #3958 ), #31547, .F. ) ;
#12027 = ADVANCED_FACE ( 'NONE', ( #14850 ), #26040, .T. ) ;
#12028 = ORIENTED_EDGE ( 'NONE', *, *, #7545, .F. ) ;
#12029 = CARTESIAN_POINT ( 'NONE',  ( 0.000000000000000000, 3.524919873834583163E-15, 68.31122994652405112 ) ) ;
#12030 = VECTOR ( 'NONE', #19843, 1000.000000000000000 ) ;
#12031 = EDGE_CURVE ( 'NONE', #29779, #15405, #4306, .T. ) ;
#12032 = ORIENTED_EDGE ( 'NONE', *, *, #26717, .T. ) ;
#12033 = AXIS2_PLACEMENT_3D ( 'NONE', #12873, #1476, #21038 ) ;
#12034 = ADVANCED_FACE ( 'NONE', ( #25862 ), #33695, .F. ) ;
#12035 = VERTEX_POINT ( 'NONE', #7149 ) ;
#12036 = CARTESIAN_POINT ( 'NONE',  ( 99.30430670822994443, -0.7984011589207654636, -7.467432841349395112 ) ) ;
#12037 = ORIENTED_EDGE ( 'NONE', *, *, #34636, .F. ) ;
#12038 = VERTEX_POINT ( 'NONE', #6454 ) ;
#12039 = CYLINDRICAL_SURFACE ( 'NONE', #3671, 2.000000000000001776 ) ;
#12040 = PRODUCT_DEFINITION_SHAPE ( 'NONE', 'NONE',  #35180 ) ;
#12041 = FACE_BOUND ( 'NONE', #4556, .T. ) ;
#12042 = DIRECTION ( 'NONE',  ( 0.000000000000000000, 0.000000000000000000, 1.000000000000000000 ) ) ;
#12043 = AXIS2_PLACEMENT_3D ( 'NONE', #3754, #28495, #33655 ) ;
#12044 = FACE_OUTER_BOUND ( 'NONE', #23646, .T. ) ;
#12045 = VERTEX_POINT ( 'NONE', #6983 ) ;
#12046 = ORIENTED_EDGE ( 'NONE', *, *, #32844, .F. ) ;
#12047 = AXIS2_PLACEMENT_3D ( 'NONE', #15517, #10163, #23857 ) ;
#12048 = CARTESIAN_POINT ( 'NONE',  ( 0.7564103444830446721, 6.875279775961484319, -33.21136585175263178 ) ) ;
#12049 = CARTESIAN_POINT ( 'NONE',  ( -499.9999999999999432, 112.9999999999999574, -155.0000000000000000 ) ) ;
#12050 = AXIS2_PLACEMENT_3D ( 'NONE', #3460, #8462, #13990 ) ;
#12051 = AXIS2_PLACEMENT_3D ( 'NONE', #26702, #13538, #366 ) ;
#12052 = CARTESIAN_POINT ( 'NONE',  ( 19.99999999999998934, 144.9999999999999716, -162.9999999999999432 ) ) ;
#12053 = FACE_OUTER_BOUND ( 'NONE', #34006, .T. ) ;
#12054 = DIRECTION ( 'NONE',  ( 1.000000000000000000, -0.000000000000000000, -0.000000000000000000 ) ) ;
#12055 = FACE_OUTER_BOUND ( 'NONE', #31079, .T. ) ;
#12056 = CARTESIAN_POINT ( 'NONE',  ( -12.00000000000001066, 134.9999999999998863, 187.0000000000000000 ) ) ;
#12057 = ORIENTED_EDGE ( 'NONE', *, *, #27974, .F. ) ;
#12058 = ADVANCED_FACE ( 'NONE', ( #1650 ), #4476, .F. ) ;
#12059 = DIRECTION ( 'NONE',  ( -0.000000000000000000, -0.000000000000000000, 1.000000000000000000 ) ) ;
#12060 = LINE ( 'NONE', #9379, #21146 ) ;
#12061 = VECTOR ( 'NONE', #16160, 1000.000000000000000 ) ;
#12062 = DIRECTION ( 'NONE',  ( 0.000000000000000000, -1.000000000000000000, 5.053935297177146739E-49 ) ) ;
#12063 = ORIENTED_EDGE ( 'NONE', *, *, #1841, .T. ) ;
#12064 = LINE ( 'NONE', #7037, #28030 ) ;
#12065 = VERTEX_POINT ( 'NONE', #23537 ) ;
#12066 = CARTESIAN_POINT ( 'NONE',  ( -109.8491107295462683, 1.661471846880725911, 12.39299840842996225 ) ) ;
#12067 = EDGE_CURVE ( 'NONE', #34039, #23769, #1481, .T. ) ;
#12068 = EDGE_CURVE ( 'NONE', #14410, #594, #15368, .T. ) ;
#12069 = VECTOR ( 'NONE', #23987, 1000.000000000000000 ) ;
#12070 = EDGE_CURVE ( 'NONE', #13149, #15074, #4422, .T. ) ;
#12072 = ORIENTED_EDGE ( 'NONE', *, *, #25302, .T. ) ;
#12071 = VECTOR ( 'NONE', #1017, 1000.000000000000000 ) ;
#12073 = CIRCLE ( 'NONE', #31925, 2.524999999999999467 ) ;
#12074 = CARTESIAN_POINT ( 'NONE',  ( 212.5000000000000000, 0.000000000000000000, 0.000000000000000000 ) ) ;
#12075 = CARTESIAN_POINT ( 'NONE',  ( 11.99999999999999645, -141.0000000000000000, 155.0000000000000000 ) ) ;
#12076 = DIRECTION ( 'NONE',  ( -0.000000000000000000, -0.000000000000000000, 1.000000000000000000 ) ) ;
#12077 = CIRCLE ( 'NONE', #31357, 34.41491905851385269 ) ;
#12078 = ORIENTED_EDGE ( 'NONE', *, *, #6797, .T. ) ;
#12079 = DIRECTION ( 'NONE',  ( -7.893605728314051750E-14, 1.618803117314786530E-15, 1.000000000000000000 ) ) ;
#12080 = DIRECTION ( 'NONE',  ( 0.000000000000000000, 0.000000000000000000, 1.000000000000000000 ) ) ;
#12081 = EDGE_LOOP ( 'NONE', ( #26547, #25326, #14108, #25082, #10575, #27217, #20655, #1845 ) ) ;
#12082 = DIRECTION ( 'NONE',  ( -1.000000000000000000, 0.000000000000000000, 0.000000000000000000 ) ) ;
#12083 = DIRECTION ( 'NONE',  ( 0.000000000000000000, 0.000000000000000000, -1.000000000000000000 ) ) ;
#12084 = CARTESIAN_POINT ( 'NONE',  ( 0.7561992243675458303, -29.46088656861464017, 16.80164552011240531 ) ) ;
#12085 = PLANE ( 'NONE',  #43 ) ;
#12086 = ITEM_DEFINED_TRANSFORMATION ( 'NONE', 'NONE', #9279,  #28566 ) ;
#12087 = ORIENTED_EDGE ( 'NONE', *, *, #28719, .T. ) ;
#12088 = EDGE_LOOP ( 'NONE', ( #18071, #19683, #34676, #9459 ) ) ;
#12089 = ORIENTED_EDGE ( 'NONE', *, *, #10011, .T. ) ;
#12090 = PRODUCT_DEFINITION_SHAPE ( 'NONE', 'NONE',  #35095 ) ;
#12091 =( NAMED_UNIT ( * ) PLANE_ANGLE_UNIT ( ) SI_UNIT ( $, .RADIAN. ) );
#12092 = CARTESIAN_POINT ( 'NONE',  ( 0.7181323043387224381, -1.866624223957557671, 4.679999999999999716 ) ) ;
#12093 = DIRECTION ( 'NONE',  ( -1.000000000000000000, -0.000000000000000000, -0.000000000000000000 ) ) ;
#12094 = CARTESIAN_POINT ( 'NONE',  ( 11.99999999999999645, 136.9999999999999716, -175.0000000000000284 ) ) ;
#12095 = AXIS2_PLACEMENT_3D ( 'NONE', #13366, #26047, #18714 ) ;
#12096 = VECTOR ( 'NONE', #17718, 1000.000000000000000 ) ;
#12097 = CARTESIAN_POINT ( 'NONE',  ( 2.265105810640112072, -32.51534716424843907, 7.547378828040344878 ) ) ;
#12098 = MECHANICAL_DESIGN_GEOMETRIC_PRESENTATION_REPRESENTATION (  '', ( #22882 ), #7511 ) ;
#12099 = LINE ( 'NONE', #22938, #7871 ) ;
#12100 = ORIENTED_EDGE ( 'NONE', *, *, #1025, .F. ) ;
#12101 = DIRECTION ( 'NONE',  ( 0.000000000000000000, 1.000000000000000000, 0.000000000000000000 ) ) ;
#12102 = CARTESIAN_POINT ( 'NONE',  ( 104.6215662523440386, 5.728791326347600688, 11.10996872791848844 ) ) ;
#12103 = ORIENTED_EDGE ( 'NONE', *, *, #7289, .T. ) ;
#12104 = PLANE ( 'NONE',  #11800 ) ;
#12105 = EDGE_CURVE ( 'NONE', #7140, #12748, #12348, .T. ) ;
#12106 = LINE ( 'NONE', #1582, #9809 ) ;
#12107 = ORIENTED_EDGE ( 'NONE', *, *, #27407, .T. ) ;
#12108 = PLANE ( 'NONE',  #10704 ) ;
#12109 = CARTESIAN_POINT ( 'NONE',  ( -12.00000000000001066, 144.9999999999999716, 155.0000000000000000 ) ) ;
#12110 = ADVANCED_FACE ( 'NONE', ( #28705 ), #4133, .T. ) ;
#12111 = CARTESIAN_POINT ( 'NONE',  ( 1.039999999999999369, -18.21166265554768060, -29.20140402659759360 ) ) ;
#12112 = ADVANCED_FACE ( 'NONE', ( #3790 ), #34220, .T. ) ;
#12113 = DIRECTION ( 'NONE',  ( -0.000000000000000000, 1.000000000000000000, -0.000000000000000000 ) ) ;
#12114 = UNCERTAINTY_MEASURE_WITH_UNIT (LENGTH_MEASURE( 1.000000000000000082E-05 ), #20850, 'distance_accuracy_value', 'NONE');
#12115 = CARTESIAN_POINT ( 'NONE',  ( -45.00000000000000000, 16.36947364650383818, -36.69637551990492597 ) ) ;
#12117 = EDGE_CURVE ( 'NONE', #29230, #25215, #7268, .T. ) ;
#12116 = FACE_OUTER_BOUND ( 'NONE', #18041, .T. ) ;
#12118 = ORIENTED_EDGE ( 'NONE', *, *, #18806, .F. ) ;
#12119 = AXIS2_PLACEMENT_3D ( 'NONE', #5342, #32047, #29216 ) ;
#12120 = ORIENTED_EDGE ( 'NONE', *, *, #11218, .T. ) ;
#12121 = AXIS2_PLACEMENT_3D ( 'NONE', #34499, #2625, #7426 ) ;
#12122 = DIRECTION ( 'NONE',  ( 8.116886477248912167E-15, -3.927377025192767386E-14, 0.9999999999999998890 ) ) ;
#12123 = AXIS2_PLACEMENT_3D ( 'NONE', #15601, #26788, #7208 ) ;
#12124 = VERTEX_POINT ( 'NONE', #6806 ) ;
#12125 = EDGE_CURVE ( 'NONE', #14959, #16209, #31112, .T. ) ;
#12126 = LINE ( 'NONE', #3558, #481 ) ;
#12127 = CARTESIAN_POINT ( 'NONE',  ( -1.155000000000000027, 0.000000000000000000, 0.000000000000000000 ) ) ;
#12128 = EDGE_LOOP ( 'NONE', ( #27441, #5758, #9864, #8964 ) ) ;
#12129 = CARTESIAN_POINT ( 'NONE',  ( 1.532562817202168137, 37.83772838912469894, 68.31122994652405112 ) ) ;
#12130 = CARTESIAN_POINT ( 'NONE',  ( -109.5893175474791690, -2.283823867687211795, -12.29365298152801778 ) ) ;
#12131 = AXIS2_PLACEMENT_3D ( 'NONE', #29245, #26392, #15918 ) ;
#12133 = LINE ( 'NONE', #33831, #21508 ) ;
#12132 = DIRECTION ( 'NONE',  ( -0.000000000000000000, -0.000000000000000000, -1.000000000000000000 ) ) ;
#12134 = EDGE_LOOP ( 'NONE', ( #19018, #22723, #14662, #17485 ) ) ;
#12135 = VERTEX_POINT ( 'NONE', #6633 ) ;
#12136 = DIRECTION ( 'NONE',  ( -1.000000000000000000, -0.000000000000000000, -0.000000000000000000 ) ) ;
#12137 = CARTESIAN_POINT ( 'NONE',  ( -499.9999999999999432, 136.9999999999999432, 190.9999999999999716 ) ) ;
#12138 = FACE_OUTER_BOUND ( 'NONE', #22003, .T. ) ;
#12139 = ORIENTED_EDGE ( 'NONE', *, *, #26867, .T. ) ;
#12140 = AXIS2_PLACEMENT_3D ( 'NONE', #11722, #19556, #22574 ) ;
#12141 = CARTESIAN_POINT ( 'NONE',  ( -12.00000000000001066, -145.0000000000000000, 159.0000000000000000 ) ) ;
#12142 = CIRCLE ( 'NONE', #24602, 32.54542015209057126 ) ;
#12143 = LINE ( 'NONE', #34496, #34234 ) ;
#12144 = CIRCLE ( 'NONE', #6421, 34.41491905851385269 ) ;
#12145 = VERTEX_POINT ( 'NONE', #15019 ) ;
#12146 = DIRECTION ( 'NONE',  ( -1.000000000000000000, -0.000000000000000000, -0.000000000000000000 ) ) ;
#12147 = DIRECTION ( 'NONE',  ( 0.000000000000000000, -7.888609052210118054E-31, -1.000000000000000000 ) ) ;
#12148 = ADVANCED_FACE ( 'NONE', ( #18052 ), #28877, .F. ) ;
#12149 = DIRECTION ( 'NONE',  ( 0.000000000000000000, 0.000000000000000000, -1.000000000000000000 ) ) ;
#12151 = DIRECTION ( 'NONE',  ( -0.000000000000000000, 1.836970198721029934E-16, -1.000000000000000000 ) ) ;
#12150 = CARTESIAN_POINT ( 'NONE',  ( -349.0000000000000000, -125.0000000000000284, 128.0000000000000000 ) ) ;
#12152 = APPLICATION_CONTEXT ( 'automotive_design' ) ;
#12153 = CARTESIAN_POINT ( 'NONE',  ( -445.9999999999999432, 137.0000000000000000, -175.0000000000000000 ) ) ;
#12154 = DIRECTION ( 'NONE',  ( -0.000000000000000000, -0.000000000000000000, -1.000000000000000000 ) ) ;
#12155 = ORIENTED_EDGE ( 'NONE', *, *, #27360, .T. ) ;
#12156 = DIRECTION ( 'NONE',  ( 1.000000000000000000, 0.000000000000000000, 0.000000000000000000 ) ) ;
#12158 = EDGE_CURVE ( 'NONE', #20178, #13790, #1621, .T. ) ;
#12157 = LINE ( 'NONE', #4455, #12697 ) ;
#12159 = EDGE_CURVE ( 'NONE', #33898, #11399, #19646, .T. ) ;
#12160 = VECTOR ( 'NONE', #24344, 1000.000000000000227 ) ;
#12161 = EDGE_LOOP ( 'NONE', ( #9956, #17862, #20973, #33833, #9612 ) ) ;
#12162 = EDGE_CURVE ( 'NONE', #35069, #2443, #15908, .T. ) ;
#12163 = EDGE_CURVE ( 'NONE', #1041, #24110, #25476, .T. ) ;
#12164 = ORIENTED_EDGE ( 'NONE', *, *, #31257, .T. ) ;
#12165 = ORIENTED_EDGE ( 'NONE', *, *, #20382, .F. ) ;
#12166 = AXIS2_PLACEMENT_3D ( 'NONE', #21566, #1809, #16064 ) ;
#12167 = DIRECTION ( 'NONE',  ( -1.000000000000000000, 0.000000000000000000, 0.000000000000000000 ) ) ;
#12168 = AXIS2_PLACEMENT_3D ( 'NONE', #12667, #1967, #21016 ) ;
#12169 = ORIENTED_EDGE ( 'NONE', *, *, #14532, .F. ) ;
#12170 = EDGE_LOOP ( 'NONE', ( #19156, #8729, #9162, #5091, #14056, #1544 ) ) ;
#12171 = EDGE_LOOP ( 'NONE', ( #5048, #9130, #19712, #14712 ) ) ;
#12172 = DIRECTION ( 'NONE',  ( -1.000000000000000000, 0.000000000000000000, 0.000000000000000000 ) ) ;
#12173 = EDGE_CURVE ( 'NONE', #34333, #13531, #2519, .T. ) ;
#12174 = CONTEXT_DEPENDENT_SHAPE_REPRESENTATION ( #7861, #7891 ) ;
#12175 = ORIENTED_EDGE ( 'NONE', *, *, #5822, .F. ) ;
#12176 = CARTESIAN_POINT ( 'NONE',  ( 0.000000000000000000, 2.281310696040539424E-14, -36.68877005347592757 ) ) ;
#12177 = DIRECTION ( 'NONE',  ( 0.000000000000000000, 1.000000000000000000, 0.000000000000000000 ) ) ;
#12178 = ORIENTED_EDGE ( 'NONE', *, *, #13235, .F. ) ;
#12179 = EDGE_LOOP ( 'NONE', ( #24309, #27182, #1244, #3827 ) ) ;
#12180 = DIRECTION ( 'NONE',  ( -0.000000000000000000, -0.000000000000000000, -1.000000000000000000 ) ) ;
#12181 = CARTESIAN_POINT ( 'NONE',  ( -410.0000000000000568, -124.9999999999999716, 132.0000000000000000 ) ) ;
#12182 = CARTESIAN_POINT ( 'NONE',  ( -6.500000000000000000, 0.000000000000000000, 5.429999999999999716 ) ) ;
#12183 = DIRECTION ( 'NONE',  ( 0.000000000000000000, -1.000000000000000000, -1.836970198721029934E-16 ) ) ;
#12184 = LINE ( 'NONE', #20190, #12030 ) ;
#12185 = ORIENTED_EDGE ( 'NONE', *, *, #1570, .T. ) ;
#12186 = EDGE_CURVE ( 'NONE', #7199, #29588, #15848, .T. ) ;
#12187 = DIRECTION ( 'NONE',  ( 0.000000000000000000, -0.000000000000000000, -1.000000000000000000 ) ) ;
#12188 = CARTESIAN_POINT ( 'NONE',  ( 12.00000000000001066, -134.9999999999999716, 187.0000000000000000 ) ) ;
#12189 = AXIS2_PLACEMENT_3D ( 'NONE', #17037, #9005, #3303 ) ;
#12190 = EDGE_CURVE ( 'NONE', #527, #9865, #23716, .T. ) ;
#12191 = DIRECTION ( 'NONE',  ( -0.9289767198167914186, -0.3701381553399144542, 0.000000000000000000 ) ) ;
#12192 = ORIENTED_EDGE ( 'NONE', *, *, #34837, .T. ) ;
#12193 = LINE ( 'NONE', #11844, #13398 ) ;
#12194 = LINE ( 'NONE', #25696, #14356 ) ;
#12195 = CARTESIAN_POINT ( 'NONE',  ( -349.0000000000000000, -125.0000000000000284, 183.0000000000000000 ) ) ;
#12196 = PRODUCT_DEFINITION_FORMATION_WITH_SPECIFIED_SOURCE ( 'ANY', '', #695, .NOT_KNOWN. ) ;
#12197 = CARTESIAN_POINT ( 'NONE',  ( 103.0997794884429197, 5.417593104495392886, -5.187149597110491506 ) ) ;
#12198 = CARTESIAN_POINT ( 'NONE',  ( 0.02407890056655825201, 14.63235270440936731, 27.43224275967444470 ) ) ;
#12199 = VECTOR ( 'NONE', #12327, 1000.000000000000000 ) ;
#12200 = AXIS2_PLACEMENT_3D ( 'NONE', #17717, #1155, #19857 ) ;
#12201 = CARTESIAN_POINT ( 'NONE',  ( -349.0000000000000000, -135.0000000000000000, 126.0000000000000000 ) ) ;
#12202 = VERTEX_POINT ( 'NONE', #32104 ) ;
#12203 = DIRECTION ( 'NONE',  ( -0.000000000000000000, -0.000000000000000000, -1.000000000000000000 ) ) ;
#12205 = DIRECTION ( 'NONE',  ( -0.000000000000000000, -0.000000000000000000, -1.000000000000000000 ) ) ;
#12204 = DIRECTION ( 'NONE',  ( 0.000000000000000000, 3.374343856708137958E-53, -1.000000000000000000 ) ) ;
#12206 = AXIS2_PLACEMENT_3D ( 'NONE', #17999, #6441, #1123 ) ;
#12207 = VERTEX_POINT ( 'NONE', #31717 ) ;
#12208 = EDGE_CURVE ( 'NONE', #23769, #13768, #8587, .T. ) ;
#12209 = EDGE_CURVE ( 'NONE', #32759, #13324, #28337, .T. ) ;
#12210 =( REPRESENTATION_RELATIONSHIP ('NONE','NONE', #23037, #28231 ) REPRESENTATION_RELATIONSHIP_WITH_TRANSFORMATION ( #23018 )SHAPE_REPRESENTATION_RELATIONSHIP( ) );
#12211 = FACE_OUTER_BOUND ( 'NONE', #33984, .T. ) ;
#12212 = ORIENTED_EDGE ( 'NONE', *, *, #21973, .T. ) ;
#12213 = VECTOR ( 'NONE', #29446, 1000.000000000000000 ) ;
#12214 = ORIENTED_EDGE ( 'NONE', *, *, #5194, .F. ) ;
#12215 = CARTESIAN_POINT ( 'NONE',  ( 100.1711952389851348, -3.105058450138034498, -6.829076936735990699 ) ) ;
#12216 = VERTEX_POINT ( 'NONE', #7502 ) ;
#12217 = VERTEX_POINT ( 'NONE', #30 ) ;
#12218 = LINE ( 'NONE', #20559, #5898 ) ;
#12219 = B_SPLINE_CURVE_WITH_KNOTS ( 'NONE', 3,
 ( #28225, #21034, #1519, #17397, #14718, #1348 ),
 .UNSPECIFIED., .F., .F.,
 ( 4, 2, 4 ),
 ( 4.404817002564675576E-07, 0.001874269606309967098, 0.003748098730919677702 ),
 .UNSPECIFIED. ) ;
#12220 = CARTESIAN_POINT ( 'NONE',  ( -5.469264258321805627, 1.713938105891546382, -0.7500000000000000000 ) ) ;
#12221 = AXIS2_PLACEMENT_3D ( 'NONE', #5896, #11089, #33322 ) ;
#12222 = DIRECTION ( 'NONE',  ( 0.000000000000000000, 0.000000000000000000, -1.000000000000000000 ) ) ;
#12223 = DIRECTION ( 'NONE',  ( -1.000000000000000000, -0.000000000000000000, -0.000000000000000000 ) ) ;
#12224 = ORIENTED_EDGE ( 'NONE', *, *, #924, .T. ) ;
#12225 = ORIENTED_EDGE ( 'NONE', *, *, #13585, .T. ) ;
#12226 = TOROIDAL_SURFACE ( 'NONE', #8793, 30.47050528711512030, 8.000000000000000000 ) ;
#12227 = CARTESIAN_POINT ( 'NONE',  ( 2.765921099433441999, -15.32140196853772984, 27.05343472112986092 ) ) ;
#12228 = LINE ( 'NONE', #9702, #34536 ) ;
#12229 = DIRECTION ( 'NONE',  ( 0.000000000000000000, 1.836970198721029441E-16, -1.000000000000000000 ) ) ;
#12230 = EDGE_CURVE ( 'NONE', #17921, #33397, #26556, .T. ) ;
#12231 = DIRECTION ( 'NONE',  ( -0.000000000000000000, -0.000000000000000000, 1.000000000000000000 ) ) ;
#12232 = DIRECTION ( 'NONE',  ( -1.000000000000000000, 0.000000000000000000, 0.000000000000000000 ) ) ;
#12233 = EDGE_CURVE ( 'NONE', #3012, #11540, #5564, .T. ) ;
#12234 = ADVANCED_FACE ( 'NONE', ( #21576 ), #4646, .F. ) ;
#12235 = CARTESIAN_POINT ( 'NONE',  ( -20.00000000000007461, 104.9999999999999858, 187.0000000000000000 ) ) ;
#12236 = CARTESIAN_POINT ( 'NONE',  ( -2.988332237913170807E-15, -11.36060796471277357, 7.322849800245833762 ) ) ;
#12237 = ORIENTED_EDGE ( 'NONE', *, *, #30869, .F. ) ;
#12238 = PLANE ( 'NONE',  #6547 ) ;
#12239 = EDGE_CURVE ( 'NONE', #19542, #26155, #31882, .T. ) ;
#12240 = LINE ( 'NONE', #19715, #6344 ) ;
#12241 = LINE ( 'NONE', #1368, #18924 ) ;
#12242 = ORIENTED_EDGE ( 'NONE', *, *, #687, .F. ) ;
#12243 = VECTOR ( 'NONE', #3388, 1000.000000000000000 ) ;
#12244 = EDGE_CURVE ( 'NONE', #736, #6259, #11860, .T. ) ;
#12245 = DIRECTION ( 'NONE',  ( 0.000000000000000000, 0.000000000000000000, 1.000000000000000000 ) ) ;
#12246 = ORIENTED_EDGE ( 'NONE', *, *, #33580, .F. ) ;
#12247 = VECTOR ( 'NONE', #23635, 1000.000000000000000 ) ;
#12248 = PLANE ( 'NONE',  #9153 ) ;
#12249 = CIRCLE ( 'NONE', #32105, 30.47050528711511674 ) ;
#12250 = ORIENTED_EDGE ( 'NONE', *, *, #11913, .T. ) ;
#12251 = VECTOR ( 'NONE', #26884, 1000.000000000000000 ) ;
#12252 = CARTESIAN_POINT ( 'NONE',  ( -42.55956070192386420, -17.65143121711728469, 20.00000000000000000 ) ) ;
#12253 = CIRCLE ( 'NONE', #32114, 6.898500000000000298 ) ;
#12254 = ORIENTED_EDGE ( 'NONE', *, *, #26324, .T. ) ;
#12255 = DIRECTION ( 'NONE',  ( -7.893605728314051750E-14, 1.618803117314786530E-15, 1.000000000000000000 ) ) ;
#12256 = CARTESIAN_POINT ( 'NONE',  ( -6.500000000000000000, 0.000000000000000000, 3.180000000000000160 ) ) ;
#12257 = ORIENTED_EDGE ( 'NONE', *, *, #29248, .F. ) ;
#12258 = LINE ( 'NONE', #9402, #5339 ) ;
#12259 = FACE_OUTER_BOUND ( 'NONE', #9003, .T. ) ;
#12260 = CIRCLE ( 'NONE', #8274, 7.999999999999979572 ) ;
#12261 = CYLINDRICAL_SURFACE ( 'NONE', #17369, 4.000000000000003553 ) ;
#12262 = CYLINDRICAL_SURFACE ( 'NONE', #11402, 34.41491905851385269 ) ;
#12263 = CONTEXT_DEPENDENT_SHAPE_REPRESENTATION ( #20357, #22825 ) ;
#12264 = VERTEX_POINT ( 'NONE', #13221 ) ;
#12265 = EDGE_LOOP ( 'NONE', ( #18382, #900, #21636, #4815, #7043, #20019, #16103, #251, #11049, #26645, #22308, #8853 ) ) ;
#12266 = ORIENTED_EDGE ( 'NONE', *, *, #21763, .T. ) ;
#12267 = B_SPLINE_CURVE_WITH_KNOTS ( 'NONE', 3,
 ( #3346, #19914, #14223, #25582 ),
 .UNSPECIFIED., .F., .F.,
 ( 4, 4 ),
 ( 0.005298404680630649545, 0.005985272568144306589 ),
 .UNSPECIFIED. ) ;
#12268 = LINE ( 'NONE', #31124, #24864 ) ;
#12269 = VECTOR ( 'NONE', #26084, 1000.000000000000000 ) ;
#12270 = CARTESIAN_POINT ( 'NONE',  ( 9.199999999999999289, 13.50000000000000178, 0.000000000000000000 ) ) ;
#12271 = EDGE_CURVE ( 'NONE', #15134, #8335, #491, .T. ) ;
#12272 = EDGE_CURVE ( 'NONE', #22594, #23988, #10362, .T. ) ;
#12273 = DIRECTION ( 'NONE',  ( 0.000000000000000000, 1.000000000000000000, 1.934419779023891545E-16 ) ) ;
#12274 = DIRECTION ( 'NONE',  ( 0.000000000000000000, 0.000000000000000000, 1.000000000000000000 ) ) ;
#12275 = VECTOR ( 'NONE', #9569, 1000.000000000000000 ) ;
#12276 = DIRECTION ( 'NONE',  ( -1.000000000000000000, -0.000000000000000000, -0.000000000000000000 ) ) ;
#12277 = DIRECTION ( 'NONE',  ( -0.000000000000000000, -1.000000000000000000, -0.000000000000000000 ) ) ;
#12278 = ORIENTED_EDGE ( 'NONE', *, *, #3654, .F. ) ;
#12279 = AXIS2_PLACEMENT_3D ( 'NONE', #1666, #34061, #23892 ) ;
#12280 = CARTESIAN_POINT ( 'NONE',  ( 110.7380848894536598, 7.027127293105233764E-16, 12.50000000000000000 ) ) ;
#12281 = VERTEX_POINT ( 'NONE', #18576 ) ;
#12282 = CARTESIAN_POINT ( 'NONE',  ( -500.0000000000000000, -113.0000000000000000, 190.9999999999999716 ) ) ;
#12283 = DIRECTION ( 'NONE',  ( 0.000000000000000000, 0.000000000000000000, 1.000000000000000000 ) ) ;
#12284 = ORIENTED_EDGE ( 'NONE', *, *, #34112, .T. ) ;
#12285 = FACE_OUTER_BOUND ( 'NONE', #24865, .T. ) ;
#12286 = DIRECTION ( 'NONE',  ( -0.2149704402110242940, 0.9766205557100865464, 0.000000000000000000 ) ) ;
#12287 = FACE_BOUND ( 'NONE', #23759, .T. ) ;
#12288 = AXIS2_PLACEMENT_3D ( 'NONE', #11119, #30681, #13786 ) ;
#12289 = CARTESIAN_POINT ( 'NONE',  ( 212.5000000000000000, 0.000000000000000000, 0.000000000000000000 ) ) ;
#12290 = DIRECTION ( 'NONE',  ( 1.000000000000000000, 0.000000000000000000, 0.000000000000000000 ) ) ;
#12291 = CARTESIAN_POINT ( 'NONE',  ( 29.63313772848251659, -13.45665341906703460, 49.43553178847298568 ) ) ;
#12292 = VECTOR ( 'NONE', #32985, 1000.000000000000000 ) ;
#12293 = ORIENTED_EDGE ( 'NONE', *, *, #32968, .F. ) ;
#12294 = EDGE_LOOP ( 'NONE', ( #31138, #6796, #7185, #20705, #24433, #26340, #5425, #21031 ) ) ;
#12295 = DIRECTION ( 'NONE',  ( -0.1063910735369017202, 0.9943243633099136947, -1.000770725407181676E-14 ) ) ;
#12296 = ORIENTED_EDGE ( 'NONE', *, *, #13818, .T. ) ;
#12297 = VECTOR ( 'NONE', #26443, 1000.000000000000000 ) ;
#12298 = DIRECTION ( 'NONE',  ( 0.000000000000000000, 1.836970198721029441E-16, -1.000000000000000000 ) ) ;
#12299 = VECTOR ( 'NONE', #33384, 1000.000000000000000 ) ;
#12300 = DIRECTION ( 'NONE',  ( 1.000000000000000000, 0.000000000000000000, -0.000000000000000000 ) ) ;
#12301 = ORIENTED_EDGE ( 'NONE', *, *, #34159, .T. ) ;
#12302 = DIRECTION ( 'NONE',  ( 1.000000000000000000, 0.000000000000000000, -1.848892746611746966E-32 ) ) ;
#12303 = CARTESIAN_POINT ( 'NONE',  ( 2.789999999999999147, -5.984944020945660803, -31.37417528048448645 ) ) ;
#12304 = EDGE_CURVE ( 'NONE', #8432, #27420, #5009, .T. ) ;
#12305 = CIRCLE ( 'NONE', #29344, 4.750000000000004441 ) ;
#12306 = EDGE_CURVE ( 'NONE', #20173, #29194, #21400, .T. ) ;
#12308 = CYLINDRICAL_SURFACE ( 'NONE', #32876, 7.999999999999979572 ) ;
#12307 = LINE ( 'NONE', #15146, #16760 ) ;
#12309 = VERTEX_POINT ( 'NONE', #22766 ) ;
#12310 = ORIENTED_EDGE ( 'NONE', *, *, #25748, .F. ) ;
#12311 = LINE ( 'NONE', #20316, #12894 ) ;
#12312 = PRODUCT_RELATED_PRODUCT_CATEGORY ( 'part', '', ( #16613 ) ) ;
#12313 = VECTOR ( 'NONE', #9193, 1000.000000000000114 ) ;
#12314 = DIRECTION ( 'NONE',  ( -1.000000000000000000, 0.000000000000000000, -0.000000000000000000 ) ) ;
#12315 = DIRECTION ( 'NONE',  ( 0.9985334138511239299, 0.05413890858541755419, 0.000000000000000000 ) ) ;
#12316 = VERTEX_POINT ( 'NONE', #5530 ) ;
#12317 = B_SPLINE_CURVE_WITH_KNOTS ( 'NONE', 3,
 ( #32393, #31858, #21383, #2316, #29917, #16049 ),
 .UNSPECIFIED., .F., .F.,
 ( 4, 2, 4 ),
 ( 2.185847997378462515E-07, 0.001873416899431755780, 0.003746615214063773666 ),
 .UNSPECIFIED. ) ;
#12318 = CARTESIAN_POINT ( 'NONE',  ( 2.765921099433441999, -23.70329957282570632, -20.11932597908854703 ) ) ;
#12319 = VERTEX_POINT ( 'NONE', #2865 ) ;
#12320 = AXIS2_PLACEMENT_3D ( 'NONE', #1333, #6656, #22874 ) ;
#12321 = CARTESIAN_POINT ( 'NONE',  ( -20.63749999999999929, 0.000000000000000000, -11.80000000000000071 ) ) ;
#12322 = FILL_AREA_STYLE ('',( #20492 ) ) ;
#12323 = DIRECTION ( 'NONE',  ( -0.9289767198167914186, -0.3701381553399144542, 0.000000000000000000 ) ) ;
#12325 = CARTESIAN_POINT ( 'NONE',  ( -6.500000000000000000, 0.000000000000000000, 3.930000000000000160 ) ) ;
#12324 = LINE ( 'NONE', #12494, #34971 ) ;
#12326 = B_SPLINE_CURVE_WITH_KNOTS ( 'NONE', 3,
 ( #24151, #16168, #18834, #15992, #26829, #10987 ),
 .UNSPECIFIED., .F., .F.,
 ( 4, 2, 4 ),
 ( 2.434544809777742014E-07, 0.001873441796234163450, 0.003746640137987348844 ),
 .UNSPECIFIED. ) ;
#12327 = DIRECTION ( 'NONE',  ( 0.000000000000000000, 5.053935297177146739E-49, 1.000000000000000000 ) ) ;
#12328 = CARTESIAN_POINT ( 'NONE',  ( 0.000000000000000000, -14.75935258146432005, 26.65732927035515232 ) ) ;
#12329 = ORIENTED_EDGE ( 'NONE', *, *, #2842, .T. ) ;
#12330 = CARTESIAN_POINT ( 'NONE',  ( 143.0000000000000568, -12.50000000000000888, -14.99999999999998757 ) ) ;
#12331 = PRODUCT_DEFINITION_SHAPE ( 'NONE', 'NONE',  #35152 ) ;
#12332 = VECTOR ( 'NONE', #1999, 1000.000000000000000 ) ;
#12333 = ORIENTED_EDGE ( 'NONE', *, *, #25258, .F. ) ;
#12334 = EDGE_LOOP ( 'NONE', ( #15230, #13, #5084, #32622 ) ) ;
#12335 = VERTEX_POINT ( 'NONE', #27435 ) ;
#12336 = DIRECTION ( 'NONE',  ( -1.000000000000000000, 0.000000000000000000, 0.000000000000000000 ) ) ;
#12337 = EDGE_LOOP ( 'NONE', ( #4632, #8523, #27391, #33417 ) ) ;
#12338 = ORIENTED_EDGE ( 'NONE', *, *, #35018, .T. ) ;
#12339 = ORIENTED_EDGE ( 'NONE', *, *, #31026, .T. ) ;
#12340 = CARTESIAN_POINT ( 'NONE',  ( -10.00000000000000000, 0.000000000000000000, 0.000000000000000000 ) ) ;
#12341 = EDGE_CURVE ( 'NONE', #15752, #1095, #16409, .T. ) ;
#12342 = EDGE_LOOP ( 'NONE', ( #1249, #7484, #9165, #6097 ) ) ;
#12343 = LINE ( 'NONE', #30677, #33414 ) ;
#12344 = LINE ( 'NONE', #25857, #31342 ) ;
#12345 = ORIENTED_EDGE ( 'NONE', *, *, #22390, .T. ) ;
#12346 = EDGE_LOOP ( 'NONE', ( #32721, #16598, #34085, #28075 ) ) ;
#12347 = DIRECTION ( 'NONE',  ( -1.000000000000000000, 0.000000000000000000, 0.000000000000000000 ) ) ;
#12348 = LINE ( 'NONE', #17874, #24325 ) ;
#12349 = ADVANCED_FACE ( 'NONE', ( #31131 ), #3047, .F. ) ;
#12350 = COLOUR_RGB ( '',0.7921568627450980005, 0.8196078431372548767, 0.9333333333333333481 ) ;
#12351 = ADVANCED_FACE ( 'NONE', ( #24573 ), #19096, .T. ) ;
#12352 = FACE_OUTER_BOUND ( 'NONE', #29460, .T. ) ;
#12353 = DIRECTION ( 'NONE',  ( 0.000000000000000000, 1.836970198721029441E-16, -1.000000000000000000 ) ) ;
#12354 = DIRECTION ( 'NONE',  ( -0.000000000000000000, 0.000000000000000000, -1.000000000000000000 ) ) ;
#12355 = EDGE_LOOP ( 'NONE', ( #15753, #33728, #20863, #27836 ) ) ;
#12357 = AXIS2_PLACEMENT_3D ( 'NONE', #15638, #2436, #20619 ) ;
#12356 = DIRECTION ( 'NONE',  ( 1.000000000000000000, 0.000000000000000000, -0.000000000000000000 ) ) ;
#12359 = CARTESIAN_POINT ( 'NONE',  ( -499.9999999999999432, 104.9999999999999858, -187.0000000000000000 ) ) ;
#12358 = VECTOR ( 'NONE', #34698, 1000.000000000000000 ) ;
#12360 = EDGE_CURVE ( 'NONE', #31191, #639, #10733, .T. ) ;
#12361 = EDGE_CURVE ( 'NONE', #6345, #34702, #2732, .T. ) ;
#12362 = CARTESIAN_POINT ( 'NONE',  ( -418.0000000000000000, -105.0000000000000142, 135.9999999999999716 ) ) ;
#12363 = ORIENTED_EDGE ( 'NONE', *, *, #10876, .T. ) ;
#12364 = CARTESIAN_POINT ( 'NONE',  ( 129.3530333899765594, -6.000000000000000000, -62.49999999999999289 ) ) ;
#12365 = CARTESIAN_POINT ( 'NONE',  ( -45.00000000000000000, -38.34433698000722046, -36.69637551990492597 ) ) ;
#12366 = LINE ( 'NONE', #6115, #197 ) ;
#12367 = EDGE_CURVE ( 'NONE', #31704, #31010, #24760, .T. ) ;
#12368 = CARTESIAN_POINT ( 'NONE',  ( -499.9999999999999432, 112.9999999999999574, 194.9999999999999716 ) ) ;
#12370 = DIRECTION ( 'NONE',  ( -1.000000000000000000, -0.000000000000000000, -0.000000000000000000 ) ) ;
#12369 = CARTESIAN_POINT ( 'NONE',  ( 0.006892389992011671226, 14.58972988903167689, 27.20448975989783946 ) ) ;
#12371 = FACE_OUTER_BOUND ( 'NONE', #4858, .T. ) ;
#12372 = VERTEX_POINT ( 'NONE', #17623 ) ;
#12373 = LINE ( 'NONE', #11852, #2486 ) ;
#12375 = CARTESIAN_POINT ( 'NONE',  ( 1.749999999999999778, 27.68252950111338251, 20.44661865013498669 ) ) ;
#12374 = CARTESIAN_POINT ( 'NONE',  ( -5.021133111225196011, -23.57973016998034765, -67.50000000000000000 ) ) ;
#12376 = AXIS2_PLACEMENT_3D ( 'NONE', #22894, #33389, #9014 ) ;
#12377 = ORIENTED_EDGE ( 'NONE', *, *, #10375, .F. ) ;
#12378 = PRODUCT_DEFINITION_SHAPE ( 'NONE', 'NONE',  #35111 ) ;
#12379 = CARTESIAN_POINT ( 'NONE',  ( 145.0000000000000568, -97.56119630548165844, -180.0000000000000000 ) ) ;
#12380 = ORIENTED_EDGE ( 'NONE', *, *, #24823, .T. ) ;
#12381 = AXIS2_PLACEMENT_3D ( 'NONE', #26126, #34854, #31635 ) ;
#12382 = CIRCLE ( 'NONE', #24264, 4.682234377621698584 ) ;
#12383 = B_SPLINE_CURVE_WITH_KNOTS ( 'NONE', 3,
 ( #19977, #31344, #7123, #1106, #9638, #12668 ),
 .UNSPECIFIED., .F., .F.,
 ( 4, 2, 4 ),
 ( 1.991142096567175704E-07, 0.001873397407604852384, 0.003746595701000048073 ),
 .UNSPECIFIED. ) ;
#12384 = ORIENTED_EDGE ( 'NONE', *, *, #30025, .T. ) ;
#12385 = CARTESIAN_POINT ( 'NONE',  ( 108.7736657769335409, -4.337494364694277849, -6.125882734748267389 ) ) ;
#12386 = EDGE_LOOP ( 'NONE', ( #25247, #30983, #7005, #29717 ) ) ;
#12387 = ORIENTED_EDGE ( 'NONE', *, *, #25659, .T. ) ;
#12388 = DIRECTION ( 'NONE',  ( -1.000000000000000000, 0.000000000000000000, 0.000000000000000000 ) ) ;
#12389 = AXIS2_PLACEMENT_3D ( 'NONE', #15286, #7239, #12606 ) ;
#12390 = FACE_OUTER_BOUND ( 'NONE', #12960, .T. ) ;
#12391 = CARTESIAN_POINT ( 'NONE',  ( 2.789999999999999147, 3.909681563761668421, 30.21863799912384962 ) ) ;
#12392 = ORIENTED_EDGE ( 'NONE', *, *, #130, .T. ) ;
#12393 = ORIENTED_EDGE ( 'NONE', *, *, #23070, .F. ) ;
#12394 = CARTESIAN_POINT ( 'NONE',  ( 29.82459402470852083, -33.69708579775584667, -49.43553178847298568 ) ) ;
#12395 = DIRECTION ( 'NONE',  ( -1.000000000000000000, 0.000000000000000000, -1.292961597001347186E-16 ) ) ;
#12396 = LINE ( 'NONE', #4690, #11840 ) ;
#12397 = EDGE_CURVE ( 'NONE', #19123, #108, #33610, .T. ) ;
#12398 = CARTESIAN_POINT ( 'NONE',  ( -445.9999999999999432, 137.0000000000000000, -155.0000000000000000 ) ) ;
#12399 = CARTESIAN_POINT ( 'NONE',  ( -12.00000000000001066, 124.9999999999999716, 155.0000000000000000 ) ) ;
#12400 = VERTEX_POINT ( 'NONE', #22104 ) ;
#12401 = DIRECTION ( 'NONE',  ( -0.000000000000000000, -0.000000000000000000, 1.000000000000000000 ) ) ;
#12402 = CIRCLE ( 'NONE', #32268, 34.41491905851385269 ) ;
#12403 = EDGE_CURVE ( 'NONE', #14044, #25273, #30948, .T. ) ;
#12404 = EDGE_CURVE ( 'NONE', #8355, #28881, #30621, .T. ) ;
#12405 = CARTESIAN_POINT ( 'NONE',  ( 10.96230482721425403, -14.55883922869198344, -77.50000000000000000 ) ) ;
#12406 = ORIENTED_EDGE ( 'NONE', *, *, #24178, .F. ) ;
#12407 = CYLINDRICAL_SURFACE ( 'NONE', #4907, 1.999999999999999112 ) ;
#12408 = CARTESIAN_POINT ( 'NONE',  ( -442.0000000000000000, 124.9999999999999432, -159.0000000000000000 ) ) ;
#12409 = CARTESIAN_POINT ( 'NONE',  ( -20.00000000000004619, -134.9999999999999716, -186.9999999999999716 ) ) ;
#12410 = ORIENTED_EDGE ( 'NONE', *, *, #16611, .T. ) ;
#12411 = AXIS2_PLACEMENT_3D ( 'NONE', #570, #24579, #401 ) ;
#12412 = VECTOR ( 'NONE', #25783, 1000.000000000000000 ) ;
#12413 =( REPRESENTATION_RELATIONSHIP ('NONE','NONE', #23037, #15767 ) REPRESENTATION_RELATIONSHIP_WITH_TRANSFORMATION ( #17612 )SHAPE_REPRESENTATION_RELATIONSHIP( ) );
#12414 = DIRECTION ( 'NONE',  ( 0.000000000000000000, 0.000000000000000000, 1.000000000000000000 ) ) ;
#12415 = VERTEX_POINT ( 'NONE', #27257 ) ;
#12416 = CARTESIAN_POINT ( 'NONE',  ( 2.789999999999999147, -3.506335382740311868, -30.89238256715869468 ) ) ;
#12417 = CARTESIAN_POINT ( 'NONE',  ( -500.0000000000000000, -137.0000000000000000, 155.0000000000000000 ) ) ;
#12418 = ADVANCED_FACE ( 'NONE', ( #3711 ), #9589, .T. ) ;
#12419 = VECTOR ( 'NONE', #8082, 1000.000000000000000 ) ;
#12420 = VERTEX_POINT ( 'NONE', #13739 ) ;
#12421 = DIRECTION ( 'NONE',  ( 0.000000000000000000, 0.000000000000000000, 1.000000000000000000 ) ) ;
#12422 = CARTESIAN_POINT ( 'NONE',  ( -418.0000000000000000, -125.0000000000000000, -101.9999999999999858 ) ) ;
#12423 = EDGE_CURVE ( 'NONE', #30526, #15904, #32308, .T. ) ;
#12424 = ORIENTED_EDGE ( 'NONE', *, *, #17654, .F. ) ;
#12425 = EDGE_CURVE ( 'NONE', #10776, #28035, #11075, .T. ) ;
#12426 = EDGE_CURVE ( 'NONE', #23952, #7073, #34016, .T. ) ;
#12427 = VECTOR ( 'NONE', #14802, 1000.000000000000000 ) ;
#12428 = DIRECTION ( 'NONE',  ( -7.893605728314051750E-14, 1.618803117314786530E-15, 1.000000000000000000 ) ) ;
#12429 = ORIENTED_EDGE ( 'NONE', *, *, #6455, .F. ) ;
#12430 = CARTESIAN_POINT ( 'NONE',  ( 109.5537947374686496, -3.510783659749455499, 12.00105596243589545 ) ) ;
#12431 = ORIENTED_EDGE ( 'NONE', *, *, #20927, .T. ) ;
#12432 = LINE ( 'NONE', #15273, #34339 ) ;
#12433 = ADVANCED_FACE ( 'NONE', ( #1400 ), #1225, .F. ) ;
#12434 = DIRECTION ( 'NONE',  ( 0.000000000000000000, -1.000000000000000000, -2.132064625830773463E-16 ) ) ;
#12435 = CIRCLE ( 'NONE', #5555, 4.000000000000003553 ) ;
#12436 = LINE ( 'NONE', #31454, #6651 ) ;
#12437 = LINE ( 'NONE', #10095, #3439 ) ;
#12438 = ORIENTED_EDGE ( 'NONE', *, *, #30913, .F. ) ;
#12439 = ORIENTED_EDGE ( 'NONE', *, *, #29512, .T. ) ;
#12440 = VECTOR ( 'NONE', #8520, 1000.000000000000000 ) ;
#12441 = ORIENTED_EDGE ( 'NONE', *, *, #4284, .F. ) ;
#12442 = CARTESIAN_POINT ( 'NONE',  ( -430.0000000000000000, -133.0000000000000000, 126.0000000000000000 ) ) ;
#12443 = CARTESIAN_POINT ( 'NONE',  ( -442.0000000000000000, 144.9999999999999716, 155.0000000000000000 ) ) ;
#12444 = CIRCLE ( 'NONE', #7894, 2.000000000000001776 ) ;
#12445 = CARTESIAN_POINT ( 'NONE',  ( -499.9999999999999432, -113.0000000000000000, -159.0000000000000000 ) ) ;
#12446 = CYLINDRICAL_SURFACE ( 'NONE', #27874, 2.000000000000001776 ) ;
#12447 = EDGE_CURVE ( 'NONE', #2115, #3468, #12099, .T. ) ;
#12448 = CARTESIAN_POINT ( 'NONE',  ( 11.99999999999999645, 144.9999999999999716, -162.9999999999999432 ) ) ;
#12449 = CARTESIAN_POINT ( 'NONE',  ( -21.17270648470164218, -7.613573412837966181, 20.00000000000000000 ) ) ;
#12450 = ORIENTED_EDGE ( 'NONE', *, *, #28120, .F. ) ;
#12451 = CARTESIAN_POINT ( 'NONE',  ( 0.02407890056655695096, -8.112136323389137260, 30.01377904834206589 ) ) ;
#12452 = AXIS2_PLACEMENT_3D ( 'NONE', #20106, #9062, #12101 ) ;
#12453 = VERTEX_POINT ( 'NONE', #8211 ) ;
#12454 = CIRCLE ( 'NONE', #13586, 32.54542015209055705 ) ;
#12455 = DIRECTION ( 'NONE',  ( -0.000000000000000000, -0.000000000000000000, 1.000000000000000000 ) ) ;
#12456 = ORIENTED_EDGE ( 'NONE', *, *, #16649, .F. ) ;
#12457 = CARTESIAN_POINT ( 'NONE',  ( -110.1150203881707625, 0.3420146137956290300, -12.50000000000000000 ) ) ;
#12458 = CARTESIAN_POINT ( 'NONE',  ( 2.789999999999999147, 14.59907093257217170, 26.74544485249471393 ) ) ;
#12459 = AXIS2_PLACEMENT_3D ( 'NONE', #14927, #20778, #12434 ) ;
#12460 = CARTESIAN_POINT ( 'NONE',  ( -1.866546971192134421E-16, -26.00523011835690923, 16.24381534199252286 ) ) ;
#12461 = DIRECTION ( 'NONE',  ( -1.000000000000000000, 0.000000000000000000, 0.000000000000000000 ) ) ;
#12462 = SURFACE_STYLE_FILL_AREA ( #31483 ) ;
#12463 = EDGE_LOOP ( 'NONE', ( #788, #4068 ) ) ;
#12464 = VECTOR ( 'NONE', #24321, 1000.000000000000114 ) ;
#12465 = EDGE_CURVE ( 'NONE', #17491, #20271, #12444, .T. ) ;
#12466 = EDGE_CURVE ( 'NONE', #32621, #3111, #5592, .T. ) ;
#12467 = ORIENTED_EDGE ( 'NONE', *, *, #19261, .F. ) ;
#12468 = DIRECTION ( 'NONE',  ( -0.9998902896478877311, 0.01481244975899929928, -3.298893004283004500E-14 ) ) ;
#12469 = ORIENTED_EDGE ( 'NONE', *, *, #3225, .T. ) ;
#12470 = CARTESIAN_POINT ( 'NONE',  ( 0.1835380929791717852, -31.53621309121726313, -6.848028948310281194 ) ) ;
#12471 = AXIS2_PLACEMENT_3D ( 'NONE', #24271, #10232, #15583 ) ;
#12472 = CARTESIAN_POINT ( 'NONE',  ( -15.99999999999998579, 75.55999999999990280, 168.2400000000000091 ) ) ;
#12474 = ADVANCED_FACE ( 'NONE', ( #2096 ), #15460, .F. ) ;
#12473 = ORIENTED_EDGE ( 'NONE', *, *, #28791, .F. ) ;
#12475 = DIRECTION ( 'NONE',  ( -1.848892746611746419E-32, -6.842277657836020854E-49, 1.000000000000000000 ) ) ;
#12476 = LINE ( 'NONE', #29184, #32863 ) ;
#12478 = FACE_OUTER_BOUND ( 'NONE', #7437, .T. ) ;
#12477 = DIRECTION ( 'NONE',  ( 0.000000000000000000, 0.000000000000000000, -1.000000000000000000 ) ) ;
#12479 = ORIENTED_EDGE ( 'NONE', *, *, #29849, .F. ) ;
#12480 = ORIENTED_EDGE ( 'NONE', *, *, #29998, .T. ) ;
#12481 = DIRECTION ( 'NONE',  ( -1.000000000000000000, 0.000000000000000000, -5.546364386991661285E-52 ) ) ;
#12482 = MANIFOLD_SOLID_BREP ( 'Square tube 40 X 40 X 4(1)[15]', #30985 ) ;
#12483 = CARTESIAN_POINT ( 'NONE',  ( 1.749999999999999778, 21.72796464722046039, -26.68861566460872226 ) ) ;
#12484 = CYLINDRICAL_SURFACE ( 'NONE', #31899, 2.524999999999999467 ) ;
#12485 = ORIENTED_EDGE ( 'NONE', *, *, #15512, .T. ) ;
#12486 = CIRCLE ( 'NONE', #28935, 34.41491905851385269 ) ;
#12487 = LINE ( 'NONE', #34535, #19722 ) ;
#12488 = VERTEX_POINT ( 'NONE', #12449 ) ;
#12489 = EDGE_CURVE ( 'NONE', #24841, #33545, #17975, .T. ) ;
#12490 = DIRECTION ( 'NONE',  ( -0.000000000000000000, -1.000000000000000000, -0.000000000000000000 ) ) ;
#12491 = DIRECTION ( 'NONE',  ( 1.000000000000000000, 0.000000000000000000, 0.000000000000000000 ) ) ;
#12492 = PRODUCT_DEFINITION_SHAPE ( 'NONE', 'NONE',  #35192 ) ;
#12493 = CARTESIAN_POINT ( 'NONE',  ( -442.0000000000000000, -125.0000000000000000, 162.9999999999999716 ) ) ;
#12495 = LINE ( 'NONE', #9808, #32724 ) ;
#12494 = CARTESIAN_POINT ( 'NONE',  ( 2.789999999999999147, 31.00221527374952046, -2.344426712874310148 ) ) ;
#12496 = VECTOR ( 'NONE', #13183, 999.9999999999998863 ) ;
#12497 = CARTESIAN_POINT ( 'NONE',  ( 0.000000000000000000, 7.489092610871091793, 29.53582882395389930 ) ) ;
#12498 = DIRECTION ( 'NONE',  ( -0.000000000000000000, -0.000000000000000000, 1.000000000000000000 ) ) ;
#12499 = DIRECTION ( 'NONE',  ( 0.000000000000000000, 0.000000000000000000, -1.000000000000000000 ) ) ;
#12500 = SURFACE_STYLE_FILL_AREA ( #1798 ) ;
#12501 = EDGE_CURVE ( 'NONE', #15497, #7557, #1642, .T. ) ;
#12502 = ADVANCED_FACE ( 'NONE', ( #18494 ), #4564, .F. ) ;
#12503 = ADVANCED_FACE ( 'NONE', ( #12614 ), #15639, .F. ) ;
#12504 = ORIENTED_EDGE ( 'NONE', *, *, #32403, .F. ) ;
#12505 = VERTEX_POINT ( 'NONE', #7594 ) ;
#12506 = ORIENTED_EDGE ( 'NONE', *, *, #11789, .T. ) ;
#12507 = AXIS2_PLACEMENT_3D ( 'NONE', #6354, #33776, #3861 ) ;
#12508 = DIRECTION ( 'NONE',  ( 0.000000000000000000, 1.000000000000000000, -0.000000000000000000 ) ) ;
#12509 = EDGE_LOOP ( 'NONE', ( #20956, #34857, #30946, #21876 ) ) ;
#12510 = ORIENTED_EDGE ( 'NONE', *, *, #33095, .F. ) ;
#12511 = ORIENTED_EDGE ( 'NONE', *, *, #8704, .T. ) ;
#12512 = PLANE ( 'NONE',  #11674 ) ;
#12513 = ORIENTED_EDGE ( 'NONE', *, *, #8543, .T. ) ;
#12514 = DIRECTION ( 'NONE',  ( 0.000000000000000000, 0.000000000000000000, 1.000000000000000000 ) ) ;
#12515 = CARTESIAN_POINT ( 'NONE',  ( 1.040000000000001590, 27.68252950111337896, 20.44661865013498314 ) ) ;
#12516 = VERTEX_POINT ( 'NONE', #34132 ) ;
#12517 = EDGE_LOOP ( 'NONE', ( #6551, #1491, #16660, #10485, #27546, #23812 ) ) ;
#12518 = LINE ( 'NONE', #25681, #20260 ) ;
#12519 = CARTESIAN_POINT ( 'NONE',  ( 28.23027531293552528, -10.15143121711728469, 20.00000000000000000 ) ) ;
#12520 = DIRECTION ( 'NONE',  ( -0.2149704402110242940, 0.9766205557100865464, 0.000000000000000000 ) ) ;
#12521 = CARTESIAN_POINT ( 'NONE',  ( -445.9999999999999432, 104.9999999999999858, -187.0000000000000000 ) ) ;
#12522 = PLANE ( 'NONE',  #10870 ) ;
#12523 = VERTEX_POINT ( 'NONE', #4924 ) ;
#12524 = PLANE ( 'NONE',  #19194 ) ;
#12525 = CARTESIAN_POINT ( 'NONE',  ( 1.040000000000000480, 6.183021911001836735, 33.85493898757064812 ) ) ;
#12526 = PLANE ( 'NONE',  #10799 ) ;
#12527 = ORIENTED_EDGE ( 'NONE', *, *, #324, .T. ) ;
#12528 = CARTESIAN_POINT ( 'NONE',  ( -5.021133111225196011, -23.57973016998034765, -67.50000000000000000 ) ) ;
#12529 = DIRECTION ( 'NONE',  ( -1.000000000000000000, 0.000000000000000000, -0.000000000000000000 ) ) ;
#12530 = CIRCLE ( 'NONE', #1150, 34.41491905851385269 ) ;
#12531 = CARTESIAN_POINT ( 'NONE',  ( -19.99999999999998934, 75.55999999999990280, -172.9900000000000091 ) ) ;
#12533 = DIRECTION ( 'NONE',  ( 0.000000000000000000, 0.000000000000000000, 1.000000000000000000 ) ) ;
#12532 = CARTESIAN_POINT ( 'NONE',  ( -442.0000000000000000, 105.0000000000000142, -101.9999999999999858 ) ) ;
#12534 = EDGE_CURVE ( 'NONE', #29191, #26985, #26653, .T. ) ;
#12535 = CARTESIAN_POINT ( 'NONE',  ( 2.765921099433441555, 24.20451283648857554, -19.51346322004903300 ) ) ;
#12536 = ORIENTED_EDGE ( 'NONE', *, *, #2677, .F. ) ;
#12537 = DIRECTION ( 'NONE',  ( 0.000000000000000000, 1.000000000000000000, 0.000000000000000000 ) ) ;
#12539 = DIRECTION ( 'NONE',  ( -1.000000000000000000, 0.000000000000000000, 0.000000000000000000 ) ) ;
#12538 = DIRECTION ( 'NONE',  ( -1.000000000000000000, -0.000000000000000000, -0.000000000000000000 ) ) ;
#12540 = EDGE_CURVE ( 'NONE', #32759, #10218, #21341, .T. ) ;
#12541 = ADVANCED_FACE ( 'NONE', ( #31636 ), #20449, .F. ) ;
#12542 = VERTEX_POINT ( 'NONE', #6895 ) ;
#12543 = CIRCLE ( 'NONE', #32412, 2.000000000000001776 ) ;
#12544 = CARTESIAN_POINT ( 'NONE',  ( -7.700000000000000178, 1.261386203121773722E-15, 10.30000000000000071 ) ) ;
#12545 = EDGE_CURVE ( 'NONE', #33018, #19775, #17793, .T. ) ;
#12546 = ORIENTED_EDGE ( 'NONE', *, *, #24169, .F. ) ;
#12547 = B_SPLINE_CURVE_WITH_KNOTS ( 'NONE', 3,
 ( #15754, #10219, #31914, #7530 ),
 .UNSPECIFIED., .F., .F.,
 ( 4, 4 ),
 ( 1.976296719774608551E-07, 0.0006879333227023559953 ),
 .UNSPECIFIED. ) ;
#12548 = ORIENTED_EDGE ( 'NONE', *, *, #18123, .T. ) ;
#12549 = DIRECTION ( 'NONE',  ( 0.000000000000000000, 0.7705132427757948044, -0.6374239897486828621 ) ) ;
#12550 = ORIENTED_EDGE ( 'NONE', *, *, #7486, .F. ) ;
#12551 = ORIENTED_EDGE ( 'NONE', *, *, #2718, .F. ) ;
#12552 = AXIS2_PLACEMENT_3D ( 'NONE', #32501, #8652, #16339 ) ;
#12553 = CARTESIAN_POINT ( 'NONE',  ( -3.250000000000000000, -5.838643359331793015, 5.429999999999999716 ) ) ;
#12554 = EDGE_CURVE ( 'NONE', #2370, #8068, #5275, .T. ) ;
#12555 = EDGE_CURVE ( 'NONE', #24340, #10848, #34038, .T. ) ;
#12556 = LINE ( 'NONE', #18092, #21459 ) ;
#12557 = CARTESIAN_POINT ( 'NONE',  ( -500.0000000000000000, -137.0000000000000000, 162.9999999999999716 ) ) ;
#12558 = ORIENTED_EDGE ( 'NONE', *, *, #32968, .T. ) ;
#12559 = ORIENTED_EDGE ( 'NONE', *, *, #3846, .F. ) ;
#12560 = DIRECTION ( 'NONE',  ( -1.000000000000000000, 0.000000000000000000, -0.000000000000000000 ) ) ;
#12561 = CARTESIAN_POINT ( 'NONE',  ( -12.00000000000001066, -124.9999999999999432, -154.9999999999999716 ) ) ;
#12562 = PLANE ( 'NONE',  #28857 ) ;
#12563 = LINE ( 'NONE', #6505, #7304 ) ;
#12564 = DIRECTION ( 'NONE',  ( 0.000000000000000000, 0.000000000000000000, 1.000000000000000000 ) ) ;
#12565 = VERTEX_POINT ( 'NONE', #15989 ) ;
#12566 = VERTEX_POINT ( 'NONE', #19355 ) ;
#12567 = CARTESIAN_POINT ( 'NONE',  ( 2.765921099433442443, 30.61125888652969707, -5.439165181698684570 ) ) ;
#12568 = VECTOR ( 'NONE', #34402, 1000.000000000000000 ) ;
#12569 = DIRECTION ( 'NONE',  ( 0.000000000000000000, 0.000000000000000000, 1.000000000000000000 ) ) ;
#12570 = EDGE_LOOP ( 'NONE', ( #24083, #11768, #6987, #23211, #25515, #24606, #22569, #3079 ) ) ;
#12571 = COLOUR_RGB ( '',0.7921568627450980005, 0.8196078431372548767, 0.9333333333333333481 ) ;
#12572 = MECHANICAL_DESIGN_GEOMETRIC_PRESENTATION_REPRESENTATION (  '', ( #9941 ), #622 ) ;
#12573 = CARTESIAN_POINT ( 'NONE',  ( 0.07094834019209503295, 31.23788557484574113, 5.357780584451035999 ) ) ;
#12574 = FACE_OUTER_BOUND ( 'NONE', #20985, .T. ) ;
#12575 = LINE ( 'NONE', #1875, #5247 ) ;
#12576 = ORIENTED_EDGE ( 'NONE', *, *, #12707, .F. ) ;
#12577 = DIRECTION ( 'NONE',  ( 1.000000000000000000, 0.000000000000000000, 0.000000000000000000 ) ) ;
#12578 = ORIENTED_EDGE ( 'NONE', *, *, #1686, .F. ) ;
#12579 = AXIS2_PLACEMENT_3D ( 'NONE', #10939, #21786, #32634 ) ;
#12581 = CARTESIAN_POINT ( 'NONE',  ( -20.00000000000007461, 136.9999999999999432, -159.0000000000000000 ) ) ;
#12580 = FACE_OUTER_BOUND ( 'NONE', #20078, .T. ) ;
#12582 = DIRECTION ( 'NONE',  ( 0.000000000000000000, -0.000000000000000000, 1.000000000000000000 ) ) ;
#12583 = VECTOR ( 'NONE', #6099, 1000.000000000000000 ) ;
#12584 = ORIENTED_EDGE ( 'NONE', *, *, #15594, .F. ) ;
#12585 = DIRECTION ( 'NONE',  ( 0.000000000000000000, 1.000000000000000000, -3.374343856708137958E-53 ) ) ;
#12586 = DIRECTION ( 'NONE',  ( 0.000000000000000000, 0.000000000000000000, 1.000000000000000000 ) ) ;
#12587 = ADVANCED_FACE ( 'NONE', ( #27007 ), #30195, .T. ) ;
#12588 = ADVANCED_FACE ( 'NONE', ( #2615, #13483, #24484 ), #13319, .T. ) ;
#12589 = ORIENTED_EDGE ( 'NONE', *, *, #1463, .T. ) ;
#12590 = AXIS2_PLACEMENT_3D ( 'NONE', #4441, #20318, #17662 ) ;
#12591 = EDGE_CURVE ( 'NONE', #13149, #5999, #16694, .T. ) ;
#12592 = EDGE_CURVE ( 'NONE', #24229, #19626, #23972, .T. ) ;
#12593 = CARTESIAN_POINT ( 'NONE',  ( 796.5387082891206774, 978.0329673548293385, 1753.598338701304101 ) ) ;
#12594 = CIRCLE ( 'NONE', #23380, 3.999999999999976019 ) ;
#12595 = EDGE_LOOP ( 'NONE', ( #97, #21219, #1436, #313 ) ) ;
#12596 = CARTESIAN_POINT ( 'NONE',  ( 99.86168570827183544, -2.560920621327513746, 12.23601723495363380 ) ) ;
#12597 = EDGE_LOOP ( 'NONE', ( #24455, #11564, #20783, #23848, #20384, #25425, #32022, #18339 ) ) ;
#12598 = LINE ( 'NONE', #1385, #26389 ) ;
#12599 = CARTESIAN_POINT ( 'NONE',  ( -12.00000000000001066, 134.9999999999999432, -194.9999999999999432 ) ) ;
#12600 = LINE ( 'NONE', #1211, #18621 ) ;
#12601 = DIRECTION ( 'NONE',  ( 0.000000000000000000, -1.000000000000000000, 0.000000000000000000 ) ) ;
#12602 = ITEM_DEFINED_TRANSFORMATION ( 'NONE', 'NONE', #16129,  #28566 ) ;
#12603 = ORIENTED_EDGE ( 'NONE', *, *, #31, .T. ) ;
#12604 = ORIENTED_EDGE ( 'NONE', *, *, #34862, .F. ) ;
#12605 = ORIENTED_EDGE ( 'NONE', *, *, #13434, .F. ) ;
#12606 = DIRECTION ( 'NONE',  ( 0.000000000000000000, 0.000000000000000000, 1.000000000000000000 ) ) ;
#12607 = EDGE_CURVE ( 'NONE', #29267, #16011, #14737, .T. ) ;
#12609 = AXIS2_PLACEMENT_3D ( 'NONE', #34128, #20273, #17448 ) ;
#12608 = CARTESIAN_POINT ( 'NONE',  ( 0.000000000000000000, 6.992329373473909019E-15, 49.43553178847298568 ) ) ;
#12610 = LINE ( 'NONE', #12792, #13929 ) ;
#12611 = DIRECTION ( 'NONE',  ( 1.000000000000000000, 0.000000000000000000, 0.000000000000000000 ) ) ;
#12613 = CARTESIAN_POINT ( 'NONE',  ( 0.000000000000000000, 0.000000000000000000, 0.000000000000000000 ) ) ;
#12612 =( REPRESENTATION_RELATIONSHIP ('NONE','NONE', #23037, #15767 ) REPRESENTATION_RELATIONSHIP_WITH_TRANSFORMATION ( #26855 )SHAPE_REPRESENTATION_RELATIONSHIP( ) );
#12614 = FACE_OUTER_BOUND ( 'NONE', #22713, .T. ) ;
#12615 = ORIENTED_EDGE ( 'NONE', *, *, #20251, .F. ) ;
#12616 = PRODUCT_DEFINITION_SHAPE ( 'NONE', 'NONE',  #35173 ) ;
#12617 = FACE_OUTER_BOUND ( 'NONE', #25678, .T. ) ;
#12618 = DIRECTION ( 'NONE',  ( -0.000000000000000000, -1.000000000000000000, -0.000000000000000000 ) ) ;
#12619 = VECTOR ( 'NONE', #30124, 1000.000000000000000 ) ;
#12621 = EDGE_CURVE ( 'NONE', #842, #10465, #22019, .T. ) ;
#12620 = EDGE_LOOP ( 'NONE', ( #29355, #18631, #22360, #6765 ) ) ;
#12622 = EDGE_CURVE ( 'NONE', #29816, #31010, #2263, .T. ) ;
#12623 = VECTOR ( 'NONE', #26656, 1000.000000000000000 ) ;
#12624 = VECTOR ( 'NONE', #4202, 1000.000000000000114 ) ;
#12626 = AXIS2_PLACEMENT_3D ( 'NONE', #2610, #10639, #17176 ) ;
#12625 = LINE ( 'NONE', #23461, #17788 ) ;
#12627 = VERTEX_POINT ( 'NONE', #32862 ) ;
#12628 = MECHANICAL_DESIGN_GEOMETRIC_PRESENTATION_REPRESENTATION (  '', ( #4077 ), #23408 ) ;
#12629 = FACE_OUTER_BOUND ( 'NONE', #19329, .T. ) ;
#12630 = CARTESIAN_POINT ( 'NONE',  ( -361.0000000000000000, -125.0000000000000284, 166.9999999999999716 ) ) ;
#12631 = DIRECTION ( 'NONE',  ( 0.000000000000000000, 0.000000000000000000, 1.000000000000000000 ) ) ;
#12632 = CARTESIAN_POINT ( 'NONE',  ( -361.0000000000000000, -125.0000000000000284, 181.0000000000000000 ) ) ;
#12633 = ORIENTED_EDGE ( 'NONE', *, *, #7162, .T. ) ;
#12634 = AXIS2_PLACEMENT_3D ( 'NONE', #8306, #5616, #16873 ) ;
#12635 = ORIENTED_EDGE ( 'NONE', *, *, #29374, .T. ) ;
#12636 = EDGE_CURVE ( 'NONE', #19693, #4380, #29505, .T. ) ;
#12637 = EDGE_CURVE ( 'NONE', #15405, #18132, #24348, .T. ) ;
#12638 = DIRECTION ( 'NONE',  ( -0.1063910735369017202, 0.9943243633099136947, -1.000770725407181676E-14 ) ) ;
#12639 = VERTEX_POINT ( 'NONE', #10464 ) ;
#12640 = ADVANCED_FACE ( 'NONE', ( #7775 ), #11630, .F. ) ;
#12641 = AXIS2_PLACEMENT_3D ( 'NONE', #1931, #32354, #29168 ) ;
#12642 = CARTESIAN_POINT ( 'NONE',  ( -442.0000000000000000, -105.0000000000000142, 159.0000000000000000 ) ) ;
#12643 = B_SPLINE_CURVE_WITH_KNOTS ( 'NONE', 3,
 ( #12280, #30953, #14422, #23130, #9758, #6380, #4050, #17978, #6731, #28628, #1229, #28104, #14601, #22944, #25246, #33972, #22769, #28287, #9595, #3881, #4230, #14774, #12102, #11748, #9426, #20281, #31133, #17625, #28454, #14945, #20452, #31294, #17796, #25961, #34317, #4568, #29152, #31989, #2441, #10110, #4748, #23814 ),
 .UNSPECIFIED., .F., .F.,
 ( 4, 2, 2, 2, 2, 2, 2, 2, 2, 2, 2, 2, 2, 2, 2, 2, 2, 2, 2, 2, 4 ),
 ( 6.816353745294061091E-19, 0.001137415812192694954, 0.002274831624385389474, 0.003412247436578083343, 0.003980955342674430061, 0.004549663248770777213, 0.005687079060963441159, 0.006824494873156104237, 0.007393202779252454858, 0.007961910685348804612, 0.009099326497541465955, 0.009668034403637816576, 0.01023674230973416720, 0.01137415812192686844, 0.01251157393411956795, 0.01364898974631226745, 0.01478640555850496870, 0.01535511346460131932, 0.01592382137069766820, 0.01706123718289036598, 0.01819865299508306375 ),
 .UNSPECIFIED. ) ;
#12644 = AXIS2_PLACEMENT_3D ( 'NONE', #6285, #19850, #20024 ) ;
#12645 = CARTESIAN_POINT ( 'NONE',  ( 212.5000000000000000, 9.184850993605147944E-16, -7.500000000000000000 ) ) ;
#12646 = CARTESIAN_POINT ( 'NONE',  ( 109.5190789905360447, -3.554721378204152682, 6.612463615769124559 ) ) ;
#12647 = AXIS2_PLACEMENT_3D ( 'NONE', #30382, #19192, #14202 ) ;
#12648 = ORIENTED_EDGE ( 'NONE', *, *, #20513, .F. ) ;
#12649 = CARTESIAN_POINT ( 'NONE',  ( 1.394999999999999574, -30.28730148581150416, -16.34215476954067015 ) ) ;
#12651 = CARTESIAN_POINT ( 'NONE',  ( 129.3530333899765594, -6.000000000000000000, -62.49999999999999289 ) ) ;
#12650 = CARTESIAN_POINT ( 'NONE',  ( -20.02113311122498729, -1.691831803474588058, -87.50000000000000000 ) ) ;
#12652 = ORIENTED_EDGE ( 'NONE', *, *, #17340, .F. ) ;
#12653 = ORIENTED_EDGE ( 'NONE', *, *, #31414, .F. ) ;
#12654 = DIRECTION ( 'NONE',  ( 0.000000000000000000, 1.836970198721029441E-16, -1.000000000000000000 ) ) ;
#12655 = VERTEX_POINT ( 'NONE', #10813 ) ;
#12656 = DIRECTION ( 'NONE',  ( -0.000000000000000000, 1.000000000000000000, 3.017235169886638201E-16 ) ) ;
#12657 = DIRECTION ( 'NONE',  ( 1.000000000000000000, 0.000000000000000000, 0.000000000000000000 ) ) ;
#12658 = ORIENTED_EDGE ( 'NONE', *, *, #12186, .F. ) ;
#12659 = EDGE_CURVE ( 'NONE', #15568, #22002, #17945, .T. ) ;
#12660 = EDGE_CURVE ( 'NONE', #22062, #30758, #8487, .T. ) ;
#12661 = CARTESIAN_POINT ( 'NONE',  ( 0.000000000000000000, -33.69708579775585378, -36.68877005347594178 ) ) ;
#12662 = PRODUCT_DEFINITION_SHAPE ( 'NONE', 'NONE',  #35119 ) ;
#12663 = ORIENTED_EDGE ( 'NONE', *, *, #22437, .F. ) ;
#12664 = FACE_BOUND ( 'NONE', #9225, .T. ) ;
#12665 = DIRECTION ( 'NONE',  ( 0.000000000000000000, -1.000000000000000000, 6.123233995736766036E-17 ) ) ;
#12666 = EDGE_CURVE ( 'NONE', #16274, #24474, #8131, .T. ) ;
#12667 = CARTESIAN_POINT ( 'NONE',  ( -3.250000000000000000, 5.404196845913421754, 3.930000000000000160 ) ) ;
#12669 = CARTESIAN_POINT ( 'NONE',  ( 2.765921099433441999, -31.05158812718222450, 1.559667679918499417 ) ) ;
#12668 = CARTESIAN_POINT ( 'NONE',  ( 1.749999999999999778, 34.10861917999616111, 4.581348211832198203 ) ) ;
#12670 = EDGE_CURVE ( 'NONE', #23952, #18561, #5455, .T. ) ;
#12671 = AXIS2_PLACEMENT_3D ( 'NONE', #1411, #17799, #12283 ) ;
#12672 = CIRCLE ( 'NONE', #13807, 3.999999999999976019 ) ;
#12673 = VECTOR ( 'NONE', #14157, 1000.000000000000000 ) ;
#12675 = EDGE_CURVE ( 'NONE', #13441, #19968, #32331, .T. ) ;
#12674 = CARTESIAN_POINT ( 'NONE',  ( 10.17231796313407344, -1.579009122040562207, -77.50000000000000000 ) ) ;
#12676 = FACE_OUTER_BOUND ( 'NONE', #15104, .T. ) ;
#12677 = CARTESIAN_POINT ( 'NONE',  ( -35.00000000000000000, -46.95407462254104303, 36.69637551990492597 ) ) ;
#12678 =( NAMED_UNIT ( * ) PLANE_ANGLE_UNIT ( ) SI_UNIT ( $, .RADIAN. ) );
#12679 = EDGE_LOOP ( 'NONE', ( #11561, #32794, #8312, #23816 ) ) ;
#12680 =( NAMED_UNIT ( * ) PLANE_ANGLE_UNIT ( ) SI_UNIT ( $, .RADIAN. ) );
#12681 = ORIENTED_EDGE ( 'NONE', *, *, #17944, .F. ) ;
#12682 = ORIENTED_EDGE ( 'NONE', *, *, #34139, .F. ) ;
#12683 = CARTESIAN_POINT ( 'NONE',  ( -20.00000000000007461, 144.9999999999999432, -187.0000000000000000 ) ) ;
#12684 = DIRECTION ( 'NONE',  ( 2.631201909438060585E-14, -5.396010391056496978E-16, 1.000000000000000000 ) ) ;
#12685 = ORIENTED_EDGE ( 'NONE', *, *, #25748, .T. ) ;
#12686 = ORIENTED_EDGE ( 'NONE', *, *, #32593, .F. ) ;
#12687 = ORIENTED_EDGE ( 'NONE', *, *, #24169, .T. ) ;
#12688 = ADVANCED_FACE ( 'NONE', ( #11882 ), #9190, .T. ) ;
#12689 = CARTESIAN_POINT ( 'NONE',  ( 0.000000000000000000, 3.524919873834583163E-15, 68.31122994652405112 ) ) ;
#12691 = AXIS2_PLACEMENT_3D ( 'NONE', #8193, #2851, #5161 ) ;
#12690 = ITEM_DEFINED_TRANSFORMATION ( 'NONE', 'NONE', #8715,  #28566 ) ;
#12692 = ORIENTED_EDGE ( 'NONE', *, *, #1128, .T. ) ;
#12693 = LINE ( 'NONE', #29407, #26630 ) ;
#12694 = AXIS2_PLACEMENT_3D ( 'NONE', #1371, #3844, #12414 ) ;
#12695 = PLANE ( 'NONE',  #4041 ) ;
#12696 = VERTEX_POINT ( 'NONE', #14376 ) ;
#12697 = VECTOR ( 'NONE', #34371, 1000.000000000000000 ) ;
#12698 = ORIENTED_EDGE ( 'NONE', *, *, #33503, .F. ) ;
#12699 = AXIS2_PLACEMENT_3D ( 'NONE', #11847, #12014, #31050 ) ;
#12700 = CARTESIAN_POINT ( 'NONE',  ( -499.9999999999999432, 144.9999999999999716, 187.0000000000000000 ) ) ;
#12701 = CARTESIAN_POINT ( 'NONE',  ( -361.0000000000000000, -125.0000000000000284, 166.9999999999999716 ) ) ;
#12702 = EDGE_CURVE ( 'NONE', #32635, #32497, #25935, .T. ) ;
#12703 = CARTESIAN_POINT ( 'NONE',  ( 0.07098928180586180914, 29.95554370010543366, 10.35423322779187316 ) ) ;
#12704 = CARTESIAN_POINT ( 'NONE',  ( 0.000000000000000000, 27.60935207499572996, -12.89090262359622585 ) ) ;
#12705 = CARTESIAN_POINT ( 'NONE',  ( 4.815661544189684840, -32.18716788982705168, 49.43553178847298568 ) ) ;
#12706 = ORIENTED_EDGE ( 'NONE', *, *, #29369, .T. ) ;
#12707 = EDGE_CURVE ( 'NONE', #4626, #24390, #3489, .T. ) ;
#12708 = DIRECTION ( 'NONE',  ( -1.000000000000000000, 6.792721752314501023E-48, -3.697785493223492838E-32 ) ) ;
#12709 = CARTESIAN_POINT ( 'NONE',  ( -355.0000000000000000, 118.9999999999999716, 130.0000000000000000 ) ) ;
#12710 = EDGE_CURVE ( 'NONE', #797, #34043, #33218, .T. ) ;
#12711 = DIRECTION ( 'NONE',  ( -1.000000000000000000, 0.000000000000000000, 0.000000000000000000 ) ) ;
#12712 = ORIENTED_EDGE ( 'NONE', *, *, #8582, .T. ) ;
#12713 = CARTESIAN_POINT ( 'NONE',  ( 8.000000000000000000, 0.000000000000000000, 0.000000000000000000 ) ) ;
#12714 = CARTESIAN_POINT ( 'NONE',  ( 0.000000000000000000, 3.524919873834583163E-15, 68.31122994652405112 ) ) ;
#12715 = DIRECTION ( 'NONE',  ( 0.000000000000000000, 0.000000000000000000, 1.000000000000000000 ) ) ;
#12717 = CARTESIAN_POINT ( 'NONE',  ( -105.1752859088571626, 5.114965439436506500, -5.485173521317547873 ) ) ;
#12716 = DIRECTION ( 'NONE',  ( 0.000000000000000000, 1.000000000000000000, 5.053935297177146739E-49 ) ) ;
#12718 = VECTOR ( 'NONE', #11264, 1000.000000000000000 ) ;
#12719 = PLANE ( 'NONE',  #10447 ) ;
#12720 = ORIENTED_EDGE ( 'NONE', *, *, #30005, .F. ) ;
#12721 = CARTESIAN_POINT ( 'NONE',  ( 109.8671414378377165, 3.044914778013033452, -12.12453154756074092 ) ) ;
#12722 = CARTESIAN_POINT ( 'NONE',  ( 0.02849990174189666672, 11.02838903529590198, -7.898269865231970499 ) ) ;
#12723 = AXIS2_PLACEMENT_3D ( 'NONE', #24172, #26498, #32191 ) ;
#12725 = ORIENTED_EDGE ( 'NONE', *, *, #11459, .T. ) ;
#12724 = VECTOR ( 'NONE', #32995, 1000.000000000000000 ) ;
#12726 = DIRECTION ( 'NONE',  ( -0.000000000000000000, -2.309213040847544338E-50, -1.000000000000000000 ) ) ;
#12727 = ORIENTED_EDGE ( 'NONE', *, *, #9770, .T. ) ;
#12728 = EDGE_LOOP ( 'NONE', ( #1988, #26335, #33246, #6193, #4436, #21000, #3188, #25962 ) ) ;
#12729 = DIRECTION ( 'NONE',  ( 0.000000000000000000, 0.000000000000000000, 1.000000000000000000 ) ) ;
#12730 = VERTEX_POINT ( 'NONE', #3318 ) ;
#12731 = EDGE_LOOP ( 'NONE', ( #308, #21879, #16333, #1807, #2508 ) ) ;
#12732 = CARTESIAN_POINT ( 'NONE',  ( -500.0000000000000000, 136.9999999999999432, -155.0000000000000000 ) ) ;
#12733 = AXIS2_PLACEMENT_3D ( 'NONE', #5122, #11009, #21858 ) ;
#12734 = CARTESIAN_POINT ( 'NONE',  ( 2.789999999999999147, -27.53147453683434520, 13.05640081644830097 ) ) ;
#12735 = FACE_OUTER_BOUND ( 'NONE', #20878, .T. ) ;
#12736 = ORIENTED_EDGE ( 'NONE', *, *, #3252, .F. ) ;
#12737 = VERTEX_POINT ( 'NONE', #31089 ) ;
#12738 = DIRECTION ( 'NONE',  ( 0.000000000000000000, 1.000000000000000000, -3.374343856708137958E-53 ) ) ;
#12739 = DIRECTION ( 'NONE',  ( 0.000000000000000000, -1.000000000000000000, 3.374343856708137958E-53 ) ) ;
#12740 = LINE ( 'NONE', #4351, #2155 ) ;
#12741 = B_SPLINE_CURVE_WITH_KNOTS ( 'NONE', 3,
 ( #9470, #3764, #6603, #1277, #9289, #30655 ),
 .UNSPECIFIED., .F., .F.,
 ( 4, 2, 4 ),
 ( 2.126639591840487065E-07, 0.001873410972133594376, 0.003746609280308004809 ),
 .UNSPECIFIED. ) ;
#12742 = EDGE_CURVE ( 'NONE', #25655, #2254, #25379, .T. ) ;
#12743 = DIRECTION ( 'NONE',  ( 0.000000000000000000, 1.310824597558155437E-49, 1.000000000000000000 ) ) ;
#12744 = CARTESIAN_POINT ( 'NONE',  ( -499.9999999999999432, 136.9999999999999432, -187.0000000000000000 ) ) ;
#12745 = UNCERTAINTY_MEASURE_WITH_UNIT (LENGTH_MEASURE( 1.000000000000000082E-05 ), #33072, 'distance_accuracy_value', 'NONE');
#12746 = ORIENTED_EDGE ( 'NONE', *, *, #9566, .F. ) ;
#12747 = AXIS2_PLACEMENT_3D ( 'NONE', #15896, #18905, #18564 ) ;
#12748 = VERTEX_POINT ( 'NONE', #11518 ) ;
#12749 = CARTESIAN_POINT ( 'NONE',  ( 1.749999999999999778, 34.10861917999616111, 4.581348211832198203 ) ) ;
#12750 = ADVANCED_FACE ( 'NONE', ( #30729 ), #17051, .T. ) ;
#12751 = AXIS2_PLACEMENT_3D ( 'NONE', #21940, #32788, #30121 ) ;
#12752 = CIRCLE ( 'NONE', #34329, 1.999999999999999556 ) ;
#12753 = DIRECTION ( 'NONE',  ( -0.000000000000000000, 0.000000000000000000, 1.000000000000000000 ) ) ;
#12754 = ORIENTED_EDGE ( 'NONE', *, *, #14404, .T. ) ;
#12755 = EDGE_CURVE ( 'NONE', #18803, #31336, #2758, .T. ) ;
#12756 = CARTESIAN_POINT ( 'NONE',  ( -410.0000000000000568, -125.0000000000000000, 162.9999999999999716 ) ) ;
#12757 = DIRECTION ( 'NONE',  ( -1.000000000000000000, -0.000000000000000000, -0.000000000000000000 ) ) ;
#12758 = ORIENTED_EDGE ( 'NONE', *, *, #21261, .T. ) ;
#12759 = FACE_OUTER_BOUND ( 'NONE', #33634, .T. ) ;
#12760 = ORIENTED_EDGE ( 'NONE', *, *, #12659, .F. ) ;
#12761 = DIRECTION ( 'NONE',  ( 1.000000000000000000, 0.000000000000000000, 0.000000000000000000 ) ) ;
#12762 = ORIENTED_EDGE ( 'NONE', *, *, #31516, .T. ) ;
#12763 = DIRECTION ( 'NONE',  ( -0.7621620551276359068, 0.6473862847818281363, 0.000000000000000000 ) ) ;
#12764 = CARTESIAN_POINT ( 'NONE',  ( 28.23027531293552528, -10.15143121711728469, 0.000000000000000000 ) ) ;
#12765 = ADVANCED_FACE ( 'NONE', ( #30560 ), #20063, .T. ) ;
#12766 = AXIS2_PLACEMENT_3D ( 'NONE', #2249, #34833, #29838 ) ;
#12767 = EDGE_LOOP ( 'NONE', ( #32048, #28767, #24933, #2203 ) ) ;
#12768 = FACE_OUTER_BOUND ( 'NONE', #15181, .T. ) ;
#12769 = DIRECTION ( 'NONE',  ( 0.4684084406997904848, 0.8835120444460226041, 0.000000000000000000 ) ) ;
#12770 = CIRCLE ( 'NONE', #33202, 11.22499999999999787 ) ;
#12771 = ORIENTED_EDGE ( 'NONE', *, *, #6056, .F. ) ;
#12772 = CARTESIAN_POINT ( 'NONE',  ( -20.63749999999999574, 1.738998454789241549E-15, 14.20000000000000107 ) ) ;
#12773 = VECTOR ( 'NONE', #8754, 1000.000000000000000 ) ;
#12774 = DIRECTION ( 'NONE',  ( -0.1063910735369225230, 0.9943243633099118073, -1.000770725407345128E-14 ) ) ;
#12775 = CIRCLE ( 'NONE', #13333, 8.000000000000007105 ) ;
#12776 = ORIENTED_EDGE ( 'NONE', *, *, #12209, .F. ) ;
#12777 = CARTESIAN_POINT ( 'NONE',  ( 109.8638085254334982, -3.050121699374164219, 12.12320065612944475 ) ) ;
#12778 = ORIENTED_EDGE ( 'NONE', *, *, #15174, .T. ) ;
#12779 = CARTESIAN_POINT ( 'NONE',  ( 0.000000000000000000, 3.524919873834583163E-15, 68.31122994652405112 ) ) ;
#12780 = AXIS2_PLACEMENT_3D ( 'NONE', #23393, #15228, #26067 ) ;
#12781 = FACE_OUTER_BOUND ( 'NONE', #11519, .T. ) ;
#12782 = CARTESIAN_POINT ( 'NONE',  ( -100.9573452668279003, -3.150844840328200558, -6.812360382669040426 ) ) ;
#12783 = DIRECTION ( 'NONE',  ( 1.000000000000000000, 0.000000000000000000, -1.848892746611746966E-32 ) ) ;
#12784 = ITEM_DEFINED_TRANSFORMATION ( 'NONE', 'NONE', #5853,  #28566 ) ;
#12785 = VERTEX_POINT ( 'NONE', #8655 ) ;
#12786 = ORIENTED_EDGE ( 'NONE', *, *, #33046, .T. ) ;
#12787 = ORIENTED_EDGE ( 'NONE', *, *, #23509, .F. ) ;
#12788 = FACE_OUTER_BOUND ( 'NONE', #22531, .T. ) ;
#12789 = ADVANCED_FACE ( 'NONE', ( #11346 ), #13575, .T. ) ;
#12790 = FACE_OUTER_BOUND ( 'NONE', #24394, .T. ) ;
#12791 = CIRCLE ( 'NONE', #23600, 10.00000000000000000 ) ;
#12792 = CARTESIAN_POINT ( 'NONE',  ( 37.09133285470120711, -7.633836879289874311, 68.31122994652405112 ) ) ;
#12793 = CARTESIAN_POINT ( 'NONE',  ( 1.749999999999999778, 6.183021911002332338, -33.85493898757056286 ) ) ;
#12794 = DIRECTION ( 'NONE',  ( -1.000000000000000000, -0.000000000000000000, -0.000000000000000000 ) ) ;
#12795 =( NAMED_UNIT ( * ) SI_UNIT ( $, .STERADIAN. ) SOLID_ANGLE_UNIT ( ) );
#12796 = ORIENTED_EDGE ( 'NONE', *, *, #15077, .T. ) ;
#12797 = EDGE_CURVE ( 'NONE', #33874, #7570, #22193, .T. ) ;
#12798 = DIRECTION ( 'NONE',  ( 0.000000000000000000, 1.000000000000000000, 0.000000000000000000 ) ) ;
#12799 = EDGE_CURVE ( 'NONE', #27908, #30767, #8459, .T. ) ;
#12800 = CARTESIAN_POINT ( 'NONE',  ( -14.84098889165989377, 28.96462362251113376, -36.68877005347593467 ) ) ;
#12801 = LINE ( 'NONE', #8483, #6549 ) ;
#12802 = CARTESIAN_POINT ( 'NONE',  ( -410.0000000000000568, -137.0000000000000000, 154.9999999999999716 ) ) ;
#12803 = VERTEX_POINT ( 'NONE', #30377 ) ;
#12804 = AXIS2_PLACEMENT_3D ( 'NONE', #6604, #17505, #6780 ) ;
#12805 = EDGE_CURVE ( 'NONE', #29324, #14034, #9020, .T. ) ;
#12806 = EDGE_CURVE ( 'NONE', #10968, #18461, #5976, .T. ) ;
#12807 = DIRECTION ( 'NONE',  ( -0.000000000000000000, 1.000000000000000000, -0.000000000000000000 ) ) ;
#12808 = EDGE_LOOP ( 'NONE', ( #1146, #32235, #28832, #22275 ) ) ;
#12809 = DIRECTION ( 'NONE',  ( 0.000000000000000000, 0.000000000000000000, 1.000000000000000000 ) ) ;
#12810 = EDGE_CURVE ( 'NONE', #14097, #6836, #17585, .T. ) ;
#12811 = PLANE ( 'NONE',  #4186 ) ;
#12812 = CARTESIAN_POINT ( 'NONE',  ( -20.02113311122478123, 16.12922284503173742, -67.50000000000000000 ) ) ;
#12813 = LINE ( 'NONE', #1588, #14508 ) ;
#12814 = DIRECTION ( 'NONE',  ( -1.300283923313630633E-47, 0.000000000000000000, -1.000000000000000000 ) ) ;
#12815 = EDGE_LOOP ( 'NONE', ( #21504, #27109, #16380, #16175, #7688, #28355, #19688, #13744 ) ) ;
#12816 = VECTOR ( 'NONE', #14671, 1000.000000000000000 ) ;
#12817 = ORIENTED_EDGE ( 'NONE', *, *, #11405, .F. ) ;
#12818 = CARTESIAN_POINT ( 'NONE',  ( 761.1790569936631528, 1358.431095301644291, 1753.598338701303646 ) ) ;
#12819 = AXIS2_PLACEMENT_3D ( 'NONE', #8842, #32865, #16520 ) ;
#12820 = B_SPLINE_CURVE_WITH_KNOTS ( 'NONE', 3,
 ( #34599, #29258, #12722, #18594, #15561, #15388, #26223, #23387 ),
 .UNSPECIFIED., .F., .F.,
 ( 4, 2, 2, 4 ),
 ( 0.007886720825438824772, 0.009850969036564027198, 0.01181521724768923136, 0.01574371366993963794 ),
 .UNSPECIFIED. ) ;
#12821 = VERTEX_POINT ( 'NONE', #33396 ) ;
#12822 = VECTOR ( 'NONE', #23456, 1000.000000000000000 ) ;
#12823 = CARTESIAN_POINT ( 'NONE',  ( 0.07098930119792198901, -31.01706505092331057, -6.518161977769946880 ) ) ;
#12824 = PLANE ( 'NONE',  #26373 ) ;
#12825 = DIRECTION ( 'NONE',  ( 0.000000000000000000, 1.131431318426415506E-52, 1.000000000000000000 ) ) ;
#12826 = VECTOR ( 'NONE', #9033, 1000.000000000000000 ) ;
#12827 = ORIENTED_EDGE ( 'NONE', *, *, #16062, .F. ) ;
#12828 = CIRCLE ( 'NONE', #6560, 3.999999999999976019 ) ;
#12829 = CARTESIAN_POINT ( 'NONE',  ( 20.89386240318430765, 24.95297350523388502, 49.43553178847298568 ) ) ;
#12831 = DIRECTION ( 'NONE',  ( -1.232595164407830946E-32, -3.421138828918010427E-49, 1.000000000000000000 ) ) ;
#12830 = LINE ( 'NONE', #9456, #21293 ) ;
#12832 = ORIENTED_EDGE ( 'NONE', *, *, #1751, .F. ) ;
#12833 = VERTEX_POINT ( 'NONE', #658 ) ;
#12834 = CARTESIAN_POINT ( 'NONE',  ( 2.033800780387780449, 22.02446183774672761, -25.79073883748058549 ) ) ;
#12835 = ORIENTED_EDGE ( 'NONE', *, *, #17849, .F. ) ;
#12836 = CARTESIAN_POINT ( 'NONE',  ( 0.000000000000000000, 6.992329373473909019E-15, 49.43553178847298568 ) ) ;
#12837 = DIRECTION ( 'NONE',  ( -1.000000000000000000, -0.000000000000000000, -0.000000000000000000 ) ) ;
#12838 = VERTEX_POINT ( 'NONE', #9376 ) ;
#12839 = AXIS2_PLACEMENT_3D ( 'NONE', #5263, #13130, #16158 ) ;
#12840 = DIRECTION ( 'NONE',  ( 0.000000000000000000, 1.310824597558155437E-49, 1.000000000000000000 ) ) ;
#12841 = ADVANCED_FACE ( 'NONE', ( #3140 ), #6329, .F. ) ;
#12842 = EDGE_CURVE ( 'NONE', #17480, #13509, #9786, .T. ) ;
#12843 = ORIENTED_EDGE ( 'NONE', *, *, #28977, .T. ) ;
#12844 = CARTESIAN_POINT ( 'NONE',  ( 11.99999999999999822, -115.0000000000000142, 155.0000000000000000 ) ) ;
#12845 = CARTESIAN_POINT ( 'NONE',  ( -430.0000000000000000, -131.0000000000000000, 130.0000000000000000 ) ) ;
#12846 = DIRECTION ( 'NONE',  ( -0.000000000000000000, -1.000000000000000000, -0.000000000000000000 ) ) ;
#12848 = LINE ( 'NONE', #9985, #15117 ) ;
#12847 = CYLINDRICAL_SURFACE ( 'NONE', #17364, 4.000000000000003553 ) ;
#12849 = DIRECTION ( 'NONE',  ( 1.000000000000000000, 0.000000000000000000, 0.000000000000000000 ) ) ;
#12850 = CARTESIAN_POINT ( 'NONE',  ( 0.000000000000000000, 29.94779062842797401, -5.619744560738746841 ) ) ;
#12851 = LINE ( 'NONE', #21023, #10506 ) ;
#12852 = DIRECTION ( 'NONE',  ( -1.000000000000000000, 0.000000000000000000, -0.000000000000000000 ) ) ;
#12853 = AXIS2_PLACEMENT_3D ( 'NONE', #13412, #24066, #28684 ) ;
#12854 = EDGE_CURVE ( 'NONE', #24248, #27019, #7375, .T. ) ;
#12855 = EDGE_LOOP ( 'NONE', ( #13695, #3364, #1118, #15492 ) ) ;
#12856 = ORIENTED_EDGE ( 'NONE', *, *, #32657, .T. ) ;
#12858 = ORIENTED_EDGE ( 'NONE', *, *, #16494, .F. ) ;
#12857 = EDGE_CURVE ( 'NONE', #25712, #4047, #5109, .T. ) ;
#12859 = EDGE_CURVE ( 'NONE', #1876, #29973, #5617, .T. ) ;
#12860 = ADVANCED_FACE ( 'NONE', ( #9708 ), #15900, .T. ) ;
#12861 = AXIS2_PLACEMENT_3D ( 'NONE', #20008, #30853, #7148 ) ;
#12862 = CARTESIAN_POINT ( 'NONE',  ( 117.4999999999998579, 0.000000000000000000, 0.000000000000000000 ) ) ;
#12863 = CARTESIAN_POINT ( 'NONE',  ( 775.9388085958107695, 1370.717311669189257, 1753.598338701303419 ) ) ;
#12864 = ORIENTED_EDGE ( 'NONE', *, *, #4115, .F. ) ;
#12865 = EDGE_LOOP ( 'NONE', ( #29599, #18345, #9557, #34184 ) ) ;
#12866 = ORIENTED_EDGE ( 'NONE', *, *, #6057, .F. ) ;
#12867 = CARTESIAN_POINT ( 'NONE',  ( 1.749999999999999778, 27.68252950111368094, -20.44661865013457458 ) ) ;
#12868 = AXIS2_PLACEMENT_3D ( 'NONE', #3923, #26303, #19803 ) ;
#12869 = LINE ( 'NONE', #13042, #24369 ) ;
#12870 = EDGE_CURVE ( 'NONE', #18597, #13218, #7031, .T. ) ;
#12871 = ORIENTED_EDGE ( 'NONE', *, *, #2830, .F. ) ;
#12872 = DIRECTION ( 'NONE',  ( -1.000000000000000000, 0.000000000000000000, 0.000000000000000000 ) ) ;
#12873 = CARTESIAN_POINT ( 'NONE',  ( 2.789999999999999147, 0.000000000000000000, 0.000000000000000000 ) ) ;
#12874 = EDGE_LOOP ( 'NONE', ( #992, #289, #9171, #2590 ) ) ;
#12875 = ORIENTED_EDGE ( 'NONE', *, *, #30630, .F. ) ;
#12876 =( REPRESENTATION_RELATIONSHIP ('NONE','NONE', #23037, #28231 ) REPRESENTATION_RELATIONSHIP_WITH_TRANSFORMATION ( #34566 )SHAPE_REPRESENTATION_RELATIONSHIP( ) );
#12877 = DIRECTION ( 'NONE',  ( 0.000000000000000000, 0.000000000000000000, 1.000000000000000000 ) ) ;
#12878 = CARTESIAN_POINT ( 'NONE',  ( -8.214752480152773925E-14, 25.77088461037005729, -16.61521147790355002 ) ) ;
#12880 = PRESENTATION_LAYER_ASSIGNMENT (  '', '', ( #23097 ) ) ;
#12879 = B_SPLINE_CURVE_WITH_KNOTS ( 'NONE', 3,
 ( #26097, #4712, #23096, #17759 ),
 .UNSPECIFIED., .F., .F.,
 ( 4, 4 ),
 ( 2.122664452422532254E-07, 0.0006879480821238661593 ),
 .UNSPECIFIED. ) ;
#12881 = FACE_OUTER_BOUND ( 'NONE', #29316, .T. ) ;
#12882 = CARTESIAN_POINT ( 'NONE',  ( 21.85761591200894216, 30.91355005303806180, 49.43553178847298568 ) ) ;
#12883 = DIRECTION ( 'NONE',  ( -1.000000000000000000, 0.000000000000000000, 0.000000000000000000 ) ) ;
#12884 = EDGE_LOOP ( 'NONE', ( #28990, #30063, #12604, #32934 ) ) ;
#12885 = DIRECTION ( 'NONE',  ( -1.000000000000000000, -3.469446951953834515E-18, 0.000000000000000000 ) ) ;
#12886 = DIRECTION ( 'NONE',  ( 1.000000000000000000, 0.000000000000000000, 0.000000000000000000 ) ) ;
#12887 = ADVANCED_FACE ( 'NONE', ( #28756, #20753 ), #17749, .T. ) ;
#12888 = ORIENTED_EDGE ( 'NONE', *, *, #20133, .T. ) ;
#12889 = DIRECTION ( 'NONE',  ( -0.6473862847818272481, 0.7621620551276367950, 1.400068981865443616E-16 ) ) ;
#12890 = CARTESIAN_POINT ( 'NONE',  ( 12.00000000000001066, -28.99999999999999645, 154.9999999999999716 ) ) ;
#12891 = CARTESIAN_POINT ( 'NONE',  ( 106.9022939876274592, 5.416883352271473662, -5.187895480218550404 ) ) ;
#12893 = CARTESIAN_POINT ( 'NONE',  ( -104.3114314540143965, 5.080227507390846498, -5.518150456212834953 ) ) ;
#12892 = CARTESIAN_POINT ( 'NONE',  ( 1.749999999999999778, 21.72796464722008380, 26.68861566460903489 ) ) ;
#12894 = VECTOR ( 'NONE', #12481, 1000.000000000000000 ) ;
#12895 = B_SPLINE_CURVE_WITH_KNOTS ( 'NONE', 3,
 ( #20377, #31225, #20207, #23219, #3975, #9680 ),
 .UNSPECIFIED., .F., .F.,
 ( 4, 2, 4 ),
 ( 4.404817030623842623E-07, 0.001874269627226452005, 0.003748098772749841601 ),
 .UNSPECIFIED. ) ;
#12896 = DIRECTION ( 'NONE',  ( 0.000000000000000000, 1.000000000000000000, 0.000000000000000000 ) ) ;
#12897 = ORIENTED_EDGE ( 'NONE', *, *, #28604, .F. ) ;
#12898 = CARTESIAN_POINT ( 'NONE',  ( 100.6912675671779880, 3.794064876973125777, -11.91123467351735776 ) ) ;
#12900 = DIRECTION ( 'NONE',  ( 0.000000000000000000, -1.000000000000000000, -2.465190328815662439E-32 ) ) ;
#12899 = DIRECTION ( 'NONE',  ( -1.000000000000000000, 0.000000000000000000, 0.000000000000000000 ) ) ;
#12901 = AXIS2_PLACEMENT_3D ( 'NONE', #30151, #10944, #445 ) ;
#12902 = ORIENTED_EDGE ( 'NONE', *, *, #13300, .T. ) ;
#12903 = FACE_BOUND ( 'NONE', #31352, .T. ) ;
#12904 = CIRCLE ( 'NONE', #17473, 32.54542015209054995 ) ;
#12905 = ORIENTED_EDGE ( 'NONE', *, *, #9566, .T. ) ;
#12906 = EDGE_CURVE ( 'NONE', #28422, #20858, #2054, .T. ) ;
#12907 = EDGE_CURVE ( 'NONE', #12488, #32903, #1703, .T. ) ;
#12908 = EDGE_LOOP ( 'NONE', ( #13992, #15521, #15968, #16779 ) ) ;
#12909 = DIRECTION ( 'NONE',  ( -1.000000000000000000, 0.000000000000000000, 0.000000000000000000 ) ) ;
#12910 = EDGE_LOOP ( 'NONE', ( #25875, #33507 ) ) ;
#12911 = ORIENTED_EDGE ( 'NONE', *, *, #32525, .F. ) ;
#12912 = CARTESIAN_POINT ( 'NONE',  ( 4.815661544189684840, -32.18716788982705168, 49.43553178847298568 ) ) ;
#12913 = PRODUCT_DEFINITION_SHAPE ( 'NONE', 'NONE',  #35155 ) ;
#12914 = VECTOR ( 'NONE', #9281, 1000.000000000000000 ) ;
#12915 = DIRECTION ( 'NONE',  ( 1.000000000000000000, 0.000000000000000000, -1.232595164407831220E-32 ) ) ;
#12916 = PLANE ( 'NONE',  #2900 ) ;
#12917 = ORIENTED_EDGE ( 'NONE', *, *, #30425, .T. ) ;
#12918 = ORIENTED_EDGE ( 'NONE', *, *, #26274, .T. ) ;
#12919 = LINE ( 'NONE', #10765, #15709 ) ;
#12920 = CARTESIAN_POINT ( 'NONE',  ( -349.0000000000000000, 124.9999999999999432, 181.0000000000000000 ) ) ;
#12921 = CARTESIAN_POINT ( 'NONE',  ( 2.789999999999999147, 23.28319895603578971, 21.86437915510226659 ) ) ;
#12922 = CARTESIAN_POINT ( 'NONE',  ( -418.0000000000000000, -104.9999999999999858, -162.9999999999999716 ) ) ;
#12923 = LINE ( 'NONE', #4518, #4566 ) ;
#12924 = ORIENTED_EDGE ( 'NONE', *, *, #1405, .F. ) ;
#12925 = LINE ( 'NONE', #34625, #13376 ) ;
#12926 = CARTESIAN_POINT ( 'NONE',  ( -19.99999999999998934, -32.99999999999997158, -175.0000000000000000 ) ) ;
#12927 = EDGE_LOOP ( 'NONE', ( #33102, #4335, #3099, #14793 ) ) ;
#12928 = CIRCLE ( 'NONE', #32796, 7.999999999999979572 ) ;
#12929 = CARTESIAN_POINT ( 'NONE',  ( -143.0000000000000568, -85.49999999999998579, 65.00000000000000000 ) ) ;
#12930 = CARTESIAN_POINT ( 'NONE',  ( 2.790000000000082636, -7.838364976555836527, 29.64395146466208431 ) ) ;
#12931 = DIRECTION ( 'NONE',  ( 1.000000000000000000, 0.000000000000000000, 0.000000000000000000 ) ) ;
#12932 = ORIENTED_EDGE ( 'NONE', *, *, #30322, .T. ) ;
#12933 = CARTESIAN_POINT ( 'NONE',  ( 2.789999999999999147, 12.39602498911143869, 27.80127684205872285 ) ) ;
#12934 = ORIENTED_EDGE ( 'NONE', *, *, #15611, .T. ) ;
#12935 = CARTESIAN_POINT ( 'NONE',  ( -442.0000000000000000, 105.0000000000000142, 159.0000000000000000 ) ) ;
#12936 = VERTEX_POINT ( 'NONE', #26087 ) ;
#12938 = CARTESIAN_POINT ( 'NONE',  ( -15.99999999999998579, -32.99999999999997158, -154.9999999999999716 ) ) ;
#12937 = SURFACE_STYLE_FILL_AREA ( #26264 ) ;
#12939 = AXIS2_PLACEMENT_3D ( 'NONE', #5185, #26911, #15544 ) ;
#12940 = AXIS2_PLACEMENT_3D ( 'NONE', #25646, #17667, #14647 ) ;
#12941 = ORIENTED_EDGE ( 'NONE', *, *, #31065, .T. ) ;
#12942 = DIRECTION ( 'NONE',  ( 1.000000000000000000, 0.000000000000000000, 0.000000000000000000 ) ) ;
#12943 = CARTESIAN_POINT ( 'NONE',  ( 2.261199760199078757, 27.45925096103250240, 18.99654502929957900 ) ) ;
#12944 = EDGE_CURVE ( 'NONE', #34260, #12785, #11054, .T. ) ;
#12945 = ORIENTED_EDGE ( 'NONE', *, *, #4431, .T. ) ;
#12946 = VECTOR ( 'NONE', #3830, 1000.000000000000000 ) ;
#12947 = ADVANCED_FACE ( 'NONE', ( #31938 ), #27231, .T. ) ;
#12948 = ADVANCED_FACE ( 'NONE', ( #23768 ), #10066, .F. ) ;
#12949 = DIRECTION ( 'NONE',  ( -7.893605728314051750E-14, 1.618803117314786530E-15, 1.000000000000000000 ) ) ;
#12950 = ORIENTED_EDGE ( 'NONE', *, *, #18613, .F. ) ;
#12951 = CARTESIAN_POINT ( 'NONE',  ( 103.4895502457613645, -5.548707632555107239, 11.20129239819138789 ) ) ;
#12952 = PRODUCT_RELATED_PRODUCT_CATEGORY ( 'part', '', ( #11202 ) ) ;
#12953 = EDGE_LOOP ( 'NONE', ( #29843, #29622, #17738, #16727 ) ) ;
#12954 = DIRECTION ( 'NONE',  ( -2.891205793294674875E-16, -7.888609052210118054E-31, -1.000000000000000000 ) ) ;
#12955 = LINE ( 'NONE', #18647, #5055 ) ;
#12956 = CARTESIAN_POINT ( 'NONE',  ( -99.92868254684908891, -0.6892679340434103574, -7.470251853870532699 ) ) ;
#12957 = CARTESIAN_POINT ( 'NONE',  ( 2.789999999999999147, -26.96806452364372575, -14.11722088188941804 ) ) ;
#12958 = ORIENTED_EDGE ( 'NONE', *, *, #7333, .T. ) ;
#12959 = ORIENTED_EDGE ( 'NONE', *, *, #22190, .T. ) ;
#12960 = EDGE_LOOP ( 'NONE', ( #24836, #6352, #23231, #10771 ) ) ;
#12961 = DIRECTION ( 'NONE',  ( -2.736911063134582149E-48, 7.888609052210118054E-31, 1.000000000000000000 ) ) ;
#12962 = DIRECTION ( 'NONE',  ( 0.000000000000000000, 0.000000000000000000, -1.000000000000000000 ) ) ;
#12963 = CIRCLE ( 'NONE', #27730, 4.750000000000004441 ) ;
#12964 = FACE_OUTER_BOUND ( 'NONE', #6130, .T. ) ;
#12965 = FACE_OUTER_BOUND ( 'NONE', #23359, .T. ) ;
#12966 = LINE ( 'NONE', #21318, #24263 ) ;
#12967 = ORIENTED_EDGE ( 'NONE', *, *, #16765, .T. ) ;
#12968 = DIRECTION ( 'NONE',  ( -0.000000000000000000, -1.836970198721029688E-16, 1.000000000000000000 ) ) ;
#12969 = DIRECTION ( 'NONE',  ( -1.000000000000000000, -0.000000000000000000, -0.000000000000000000 ) ) ;
#12970 = CIRCLE ( 'NONE', #16386, 30.47050528711511674 ) ;
#12971 = CARTESIAN_POINT ( 'NONE',  ( -18.45373714011839539, 26.80790850550483029, -36.68877005347593467 ) ) ;
#12972 = EDGE_LOOP ( 'NONE', ( #31313, #14636 ) ) ;
#12973 = CARTESIAN_POINT ( 'NONE',  ( 0.1134162231553477451, -2.627030748436328889, -13.50000000000000000 ) ) ;
#12974 = ORIENTED_EDGE ( 'NONE', *, *, #27882, .F. ) ;
#12975 = LINE ( 'NONE', #17801, #24531 ) ;
#12976 = DIRECTION ( 'NONE',  ( 1.000000000000000000, 0.000000000000000000, 0.000000000000000000 ) ) ;
#12977 = AXIS2_PLACEMENT_3D ( 'NONE', #29041, #4301, #26375 ) ;
#12978 = EDGE_LOOP ( 'NONE', ( #16606, #34035, #21068, #2241 ) ) ;
#12979 = EDGE_CURVE ( 'NONE', #10757, #4201, #15073, .T. ) ;
#12980 = FACE_OUTER_BOUND ( 'NONE', #2051, .T. ) ;
#12981 = DIRECTION ( 'NONE',  ( 0.000000000000000000, 0.000000000000000000, -1.000000000000000000 ) ) ;
#12982 = CARTESIAN_POINT ( 'NONE',  ( -15.99999999999998579, 4.559999999999908127, 172.9900000000000091 ) ) ;
#12983 = EDGE_CURVE ( 'NONE', #31630, #2660, #17580, .T. ) ;
#12984 = EDGE_LOOP ( 'NONE', ( #20355, #27528, #30670 ) ) ;
#12985 = CIRCLE ( 'NONE', #14125, 32.54542015209055705 ) ;
#12986 = VERTEX_POINT ( 'NONE', #23084 ) ;
#12987 = CARTESIAN_POINT ( 'NONE',  ( 768.4489308355631465, 1229.883081805944812, 1753.598338701303192 ) ) ;
#12988 = CIRCLE ( 'NONE', #33941, 2.033421858999710619 ) ;
#12989 = ADVANCED_FACE ( 'NONE', ( #33929 ), #32640, .F. ) ;
#12990 = ORIENTED_EDGE ( 'NONE', *, *, #27186, .T. ) ;
#12991 = DIRECTION ( 'NONE',  ( 0.000000000000000000, 5.053935297177146739E-49, 1.000000000000000000 ) ) ;
#12992 = B_SPLINE_CURVE_WITH_KNOTS ( 'NONE', 3,
 ( #19827, #589, #20818, #20646 ),
 .UNSPECIFIED., .F., .F.,
 ( 4, 4 ),
 ( 0.005298517298376331439, 0.005985383706685557664 ),
 .UNSPECIFIED. ) ;
#12993 = AXIS2_PLACEMENT_3D ( 'NONE', #21222, #10192, #21042 ) ;
#12994 = LINE ( 'NONE', #15138, #25468 ) ;
#12995 = DIRECTION ( 'NONE',  ( -1.000000000000000000, -0.000000000000000000, -0.000000000000000000 ) ) ;
#12996 = LINE ( 'NONE', #10495, #26152 ) ;
#12997 = EDGE_CURVE ( 'NONE', #23325, #2234, #30085, .T. ) ;
#12998 = CONTEXT_DEPENDENT_SHAPE_REPRESENTATION ( #9443, #6611 ) ;
#12999 = ORIENTED_EDGE ( 'NONE', *, *, #1833, .T. ) ;
#13000 = CARTESIAN_POINT ( 'NONE',  ( 22.89764159710611224, 17.63622956525712127, -77.50000000000000000 ) ) ;
#13001 = EDGE_CURVE ( 'NONE', #7776, #25782, #24380, .T. ) ;
#13002 = VECTOR ( 'NONE', #21540, 1000.000000000000114 ) ;
#13003 = ADVANCED_FACE ( 'NONE', ( #18962 ), #5410, .F. ) ;
#13005 = CARTESIAN_POINT ( 'NONE',  ( -45.05956070192387841, -32.65143121711728469, 20.00000000000000000 ) ) ;
#13004 = DIRECTION ( 'NONE',  ( 3.697785493223492838E-32, 1.934419779023891545E-16, -1.000000000000000000 ) ) ;
#13006 = AXIS2_PLACEMENT_3D ( 'NONE', #9967, #34527, #4961 ) ;
#13007 = EDGE_LOOP ( 'NONE', ( #1034, #11033, #5520, #4438 ) ) ;
#13008 = ORIENTED_EDGE ( 'NONE', *, *, #12906, .F. ) ;
#13009 = CARTESIAN_POINT ( 'NONE',  ( -143.0000000000000568, -45.49999999999999289, 51.88904920397793319 ) ) ;
#13010 = ORIENTED_EDGE ( 'NONE', *, *, #19064, .F. ) ;
#13011 = DIRECTION ( 'NONE',  ( -1.000000000000000000, 0.000000000000000000, -1.300283923313630633E-47 ) ) ;
#13012 = CARTESIAN_POINT ( 'NONE',  ( -7.700000000000000178, 1.224646799147353059E-15, 9.999999999999998224 ) ) ;
#13013 = ORIENTED_EDGE ( 'NONE', *, *, #1959, .T. ) ;
#13014 = AXIS2_PLACEMENT_3D ( 'NONE', #20603, #31115, #12083 ) ;
#13015 = CARTESIAN_POINT ( 'NONE',  ( -15.99999999999998579, 112.9999999999999574, -175.0000000000000284 ) ) ;
#13016 = PRODUCT_DEFINITION_SHAPE ( 'NONE', 'NONE',  #35198 ) ;
#13017 = B_SPLINE_CURVE_WITH_KNOTS ( 'NONE', 3,
 ( #30768, #3877, #1052, #12097, #23293, #19754 ),
 .UNSPECIFIED., .F., .F.,
 ( 4, 2, 4 ),
 ( 2.257612537733862618E-07, 0.001873424083712457808, 0.003746622406171142526 ),
 .UNSPECIFIED. ) ;
#13018 = CARTESIAN_POINT ( 'NONE',  ( -5.210000000000000853, 0.000000000000000000, 0.000000000000000000 ) ) ;
#13019 = ORIENTED_EDGE ( 'NONE', *, *, #12423, .T. ) ;
#13020 = CARTESIAN_POINT ( 'NONE',  ( -7.654999999999999361, 1.414467053015192657E-16, 4.679999999999999716 ) ) ;
#13021 = CARTESIAN_POINT ( 'NONE',  ( 2.789999999999999147, 11.30192140231272191, -28.29696565125058072 ) ) ;
#13022 = DIRECTION ( 'NONE',  ( 0.000000000000000000, -1.000000000000000000, -1.224646799147353207E-16 ) ) ;
#13023 = VECTOR ( 'NONE', #14732, 1000.000000000000000 ) ;
#13025 = DIRECTION ( 'NONE',  ( 0.000000000000000000, 1.000000000000000000, -3.374343856708137958E-53 ) ) ;
#13024 = LINE ( 'NONE', #18551, #3679 ) ;
#13026 = DIRECTION ( 'NONE',  ( 0.000000000000000000, 1.000000000000000000, 5.145227585319922065E-49 ) ) ;
#13027 = CARTESIAN_POINT ( 'NONE',  ( 187.4264068711928530, -12.50000000000000888, -14.99999999999998757 ) ) ;
#13028 = CARTESIAN_POINT ( 'NONE',  ( 2.790000000000080860, 18.20059223136379600, -24.67675383855231885 ) ) ;
#13029 = CONICAL_SURFACE ( 'NONE', #32901, 13.50000000000000000, 1.047197551196600296 ) ;
#13030 = VERTEX_POINT ( 'NONE', #18789 ) ;
#13031 = ORIENTED_EDGE ( 'NONE', *, *, #10213, .F. ) ;
#13032 = VERTEX_POINT ( 'NONE', #27131 ) ;
#13033 = EDGE_CURVE ( 'NONE', #27628, #35091, #10413, .T. ) ;
#13034 = VECTOR ( 'NONE', #20050, 1000.000000000000000 ) ;
#13035 = ADVANCED_FACE ( 'NONE', ( #18445 ), #13271, .F. ) ;
#13036 = CARTESIAN_POINT ( 'NONE',  ( 0.000000000000000000, 0.000000000000000000, 0.000000000000000000 ) ) ;
#13037 = EDGE_CURVE ( 'NONE', #25124, #17976, #3373, .T. ) ;
#13038 = CARTESIAN_POINT ( 'NONE',  ( 822.4997240610812241, 1334.697290463531772, 1332.896119909287108 ) ) ;
#13039 = VERTEX_POINT ( 'NONE', #2915 ) ;
#13040 = EDGE_LOOP ( 'NONE', ( #22858, #13505, #21745, #17163 ) ) ;
#13041 = DIRECTION ( 'NONE',  ( -1.000000000000000000, 0.000000000000000000, 0.000000000000000000 ) ) ;
#13042 = CARTESIAN_POINT ( 'NONE',  ( 145.0000000000000568, -88.29863524074325198, -74.12844257252345415 ) ) ;
#13043 = DIRECTION ( 'NONE',  ( 0.000000000000000000, 0.000000000000000000, 1.000000000000000000 ) ) ;
#13044 = DIRECTION ( 'NONE',  ( -1.000000000000000000, 0.000000000000000000, 0.000000000000000000 ) ) ;
#13045 = EDGE_LOOP ( 'NONE', ( #11355, #32619, #21428, #10856 ) ) ;
#13046 = ORIENTED_EDGE ( 'NONE', *, *, #8352, .T. ) ;
#13047 = CARTESIAN_POINT ( 'NONE',  ( 15.99999999999998579, 75.55999999999990280, -172.9900000000000091 ) ) ;
#13048 = CARTESIAN_POINT ( 'NONE',  ( -32.54223829851967764, 0.4550817492056100644, 68.31122994652405112 ) ) ;
#13049 = PLANE ( 'NONE',  #23835 ) ;
#13051 = EDGE_CURVE ( 'NONE', #15452, #29720, #2224, .T. ) ;
#13050 = CARTESIAN_POINT ( 'NONE',  ( 2.789999999999999147, -27.53147453683434520, 13.05640081644830097 ) ) ;
#13052 = DIRECTION ( 'NONE',  ( -0.000000000000000000, -0.000000000000000000, -1.000000000000000000 ) ) ;
#13053 = ORIENTED_EDGE ( 'NONE', *, *, #20298, .T. ) ;
#13054 = LINE ( 'NONE', #13404, #33963 ) ;
#13055 = DIRECTION ( 'NONE',  ( 1.000000000000000000, 0.000000000000000000, 0.000000000000000000 ) ) ;
#13056 = AXIS2_PLACEMENT_3D ( 'NONE', #29235, #23718, #34576 ) ;
#13057 = DIRECTION ( 'NONE',  ( 0.000000000000000000, 0.000000000000000000, 1.000000000000000000 ) ) ;
#13058 = EDGE_CURVE ( 'NONE', #18790, #26143, #10600, .T. ) ;
#13059 = CARTESIAN_POINT ( 'NONE',  ( -347.0000000000000000, -125.0000000000000284, 114.0000000000000000 ) ) ;
#13060 = PLANE ( 'NONE',  #20095 ) ;
#13062 = DIRECTION ( 'NONE',  ( 0.000000000000000000, 1.000000000000000000, 1.224646799147353207E-16 ) ) ;
#13061 = DIRECTION ( 'NONE',  ( 0.000000000000000000, 1.836970198721029441E-16, -1.000000000000000000 ) ) ;
#13063 = ADVANCED_FACE ( 'NONE', ( #16122 ), #15775, .F. ) ;
#13064 = EDGE_CURVE ( 'NONE', #9815, #32472, #12486, .T. ) ;
#13065 = CARTESIAN_POINT ( 'NONE',  ( 1.394999999999999574, 14.40815186467776243, 31.25366880301324457 ) ) ;
#13066 = ORIENTED_EDGE ( 'NONE', *, *, #18944, .F. ) ;
#13067 = CARTESIAN_POINT ( 'NONE',  ( -442.0000000000000000, 124.9999999999999574, -187.0000000000000000 ) ) ;
#13069 = CARTESIAN_POINT ( 'NONE',  ( -355.0000000000000000, 130.9999999999999716, 111.9999999999999858 ) ) ;
#13068 = CARTESIAN_POINT ( 'NONE',  ( -18.38714294329533416, -33.09555747561021377, 68.31122994652405112 ) ) ;
#13070 = ADVANCED_FACE ( 'NONE', ( #2569 ), #2745, .T. ) ;
#13071 = CIRCLE ( 'NONE', #7939, 10.87635688602997597 ) ;
#13072 = ORIENTED_EDGE ( 'NONE', *, *, #16795, .T. ) ;
#13073 = DIRECTION ( 'NONE',  ( 1.000000000000000000, 0.000000000000000000, 0.000000000000000000 ) ) ;
#13074 = VERTEX_POINT ( 'NONE', #81 ) ;
#13075 = ADVANCED_FACE ( 'NONE', ( #21790 ), #21900, .F. ) ;
#13076 = EDGE_CURVE ( 'NONE', #33119, #5849, #8482, .T. ) ;
#13077 =( REPRESENTATION_RELATIONSHIP ('NONE','NONE', #23037, #15767 ) REPRESENTATION_RELATIONSHIP_WITH_TRANSFORMATION ( #33783 )SHAPE_REPRESENTATION_RELATIONSHIP( ) );
#13078 = VERTEX_POINT ( 'NONE', #5579 ) ;
#13079 = CARTESIAN_POINT ( 'NONE',  ( -442.0000000000000000, -105.0000000000000142, 162.9999999999999716 ) ) ;
#13080 = ORIENTED_EDGE ( 'NONE', *, *, #25550, .F. ) ;
#13081 = ORIENTED_EDGE ( 'NONE', *, *, #13239, .F. ) ;
#13082 = DIRECTION ( 'NONE',  ( 1.000000000000000000, 3.040835319149746090E-31, 1.232595164407830946E-32 ) ) ;
#13083 = DIRECTION ( 'NONE',  ( 0.000000000000000000, -1.000000000000000000, 0.000000000000000000 ) ) ;
#13084 = CARTESIAN_POINT ( 'NONE',  ( 2.789999999999999591, 0.000000000000000000, 3.000000000000000000 ) ) ;
#13085 = ORIENTED_EDGE ( 'NONE', *, *, #12755, .F. ) ;
#13086 = ORIENTED_EDGE ( 'NONE', *, *, #893, .T. ) ;
#13087 = CARTESIAN_POINT ( 'NONE',  ( 19.99999999999998934, 144.9999999999999716, 162.9999999999999716 ) ) ;
#13088 = CYLINDRICAL_SURFACE ( 'NONE', #18629, 4.750000000000004441 ) ;
#13089 = CARTESIAN_POINT ( 'NONE',  ( -19.99999999999998934, 134.9999999999998863, 162.9999999999999716 ) ) ;
#13090 = DIRECTION ( 'NONE',  ( 0.000000000000000000, 0.000000000000000000, -1.000000000000000000 ) ) ;
#13091 = CARTESIAN_POINT ( 'NONE',  ( -442.0000000000000000, -105.0000000000000142, 132.0000000000000000 ) ) ;
#13092 = ORIENTED_EDGE ( 'NONE', *, *, #7857, .T. ) ;
#13093 = VECTOR ( 'NONE', #21913, 1000.000000000000000 ) ;
#13094 = DIRECTION ( 'NONE',  ( 0.000000000000000000, 1.836970198721029441E-16, -1.000000000000000000 ) ) ;
#13095 = FACE_OUTER_BOUND ( 'NONE', #18643, .T. ) ;
#13096 = ORIENTED_EDGE ( 'NONE', *, *, #11055, .T. ) ;
#13097 = FACE_OUTER_BOUND ( 'NONE', #28017, .T. ) ;
#13098 = CARTESIAN_POINT ( 'NONE',  ( -17.07420202168509604, 33.79163469797343566, -36.68877005347593467 ) ) ;
#13099 = CARTESIAN_POINT ( 'NONE',  ( 11.99999999999999645, 144.9999999999999716, -175.0000000000000284 ) ) ;
#13100 = ORIENTED_EDGE ( 'NONE', *, *, #32383, .T. ) ;
#13101 = EDGE_CURVE ( 'NONE', #17435, #32572, #13596, .T. ) ;
#13102 = DIRECTION ( 'NONE',  ( 0.000000000000000000, -1.000000000000000000, 0.000000000000000000 ) ) ;
#13103 = ORIENTED_EDGE ( 'NONE', *, *, #25006, .T. ) ;
#13104 = ADVANCED_FACE ( 'NONE', ( #13095 ), #18619, .T. ) ;
#13105 = CARTESIAN_POINT ( 'NONE',  ( -499.9999999999999432, -113.0000000000000000, -155.0000000000000000 ) ) ;
#13106 = EDGE_LOOP ( 'NONE', ( #7308, #1215, #32524, #25166 ) ) ;
#13108 = DIRECTION ( 'NONE',  ( 0.000000000000000000, 1.000000000000000000, -6.842277657836020854E-49 ) ) ;
#13107 = CARTESIAN_POINT ( 'NONE',  ( 0.07406964051085589140, 28.96583153378254849, 12.96313068902594878 ) ) ;
#13109 = DIRECTION ( 'NONE',  ( 0.000000000000000000, 1.310824597558155437E-49, 1.000000000000000000 ) ) ;
#13110 = EDGE_CURVE ( 'NONE', #6878, #22746, #11950, .T. ) ;
#13111 = ORIENTED_EDGE ( 'NONE', *, *, #25853, .T. ) ;
#13112 = CARTESIAN_POINT ( 'NONE',  ( 2.123179190381536685, -33.69708579775584667, 68.31122994652405112 ) ) ;
#13113 = ADVANCED_FACE ( 'NONE', ( #6465 ), #17366, .F. ) ;
#13114 = DIRECTION ( 'NONE',  ( 0.000000000000000000, 1.836970198721029934E-16, -1.000000000000000000 ) ) ;
#13115 = ORIENTED_EDGE ( 'NONE', *, *, #24288, .F. ) ;
#13116 = VECTOR ( 'NONE', #16332, 1000.000000000000000 ) ;
#13117 = DIRECTION ( 'NONE',  ( -7.552623087826156950E-14, 1.920549054132217378E-14, 0.9999999999999998890 ) ) ;
#13118 = EDGE_LOOP ( 'NONE', ( #11501, #5227, #4835, #6720 ) ) ;
#13119 = PLANE ( 'NONE',  #26136 ) ;
#13120 = VERTEX_POINT ( 'NONE', #25514 ) ;
#13121 = FACE_OUTER_BOUND ( 'NONE', #2389, .T. ) ;
#13122 = CARTESIAN_POINT ( 'NONE',  ( -106.6942439354515955, -4.837552664684794834, -5.733718144795174609 ) ) ;
#13123 = VECTOR ( 'NONE', #5703, 1000.000000000000000 ) ;
#13124 = DIRECTION ( 'NONE',  ( 0.000000000000000000, 0.000000000000000000, -1.000000000000000000 ) ) ;
#13125 = ITEM_DEFINED_TRANSFORMATION ( 'NONE', 'NONE', #25197,  #28566 ) ;
#13126 = ORIENTED_EDGE ( 'NONE', *, *, #27672, .F. ) ;
#13127 = ORIENTED_EDGE ( 'NONE', *, *, #32454, .F. ) ;
#13128 = AXIS2_PLACEMENT_3D ( 'NONE', #4197, #15608, #1192 ) ;
#13129 = EDGE_LOOP ( 'NONE', ( #7506, #21027, #8446, #8378 ) ) ;
#13130 = DIRECTION ( 'NONE',  ( -3.469446951953832974E-18, -1.000000000000000000, -7.888609052210116302E-31 ) ) ;
#13131 = EDGE_CURVE ( 'NONE', #4232, #501, #14690, .T. ) ;
#13132 = DIRECTION ( 'NONE',  ( 0.000000000000000000, -1.000000000000000000, -1.541976423090495633E-16 ) ) ;
#13133 = CARTESIAN_POINT ( 'NONE',  ( 15.99999999999998579, 75.55999999999990280, -168.2400000000000091 ) ) ;
#13134 = CYLINDRICAL_SURFACE ( 'NONE', #26444, 1.155000000000000027 ) ;
#13135 = FACE_OUTER_BOUND ( 'NONE', #20558, .T. ) ;
#13136 = CARTESIAN_POINT ( 'NONE',  ( 15.99999999999998579, -32.99999999999997158, -175.0000000000000000 ) ) ;
#13137 = DIRECTION ( 'NONE',  ( 0.000000000000000000, 2.309213040847544338E-50, 1.000000000000000000 ) ) ;
#13138 = ORIENTED_EDGE ( 'NONE', *, *, #2196, .T. ) ;
#13139 = AXIS2_PLACEMENT_3D ( 'NONE', #19885, #25377, #3487 ) ;
#13140 = EDGE_CURVE ( 'NONE', #24525, #28865, #17608, .T. ) ;
#13141 = DIRECTION ( 'NONE',  ( 0.000000000000000000, -1.000000000000000000, 0.000000000000000000 ) ) ;
#13142 = PLANE ( 'NONE',  #9761 ) ;
#13143 = CIRCLE ( 'NONE', #5713, 32.54542015209054995 ) ;
#13144 = EDGE_CURVE ( 'NONE', #25632, #15499, #3274, .T. ) ;
#13145 = DIRECTION ( 'NONE',  ( 1.000000000000000000, 3.469446951953834515E-18, 0.000000000000000000 ) ) ;
#13146 = VERTEX_POINT ( 'NONE', #33355 ) ;
#13147 = EDGE_CURVE ( 'NONE', #29871, #20735, #17011, .T. ) ;
#13148 = FACE_OUTER_BOUND ( 'NONE', #7583, .T. ) ;
#13149 = VERTEX_POINT ( 'NONE', #11300 ) ;
#13150 = CYLINDRICAL_SURFACE ( 'NONE', #14918, 7.999999999999979572 ) ;
#13151 = FACE_OUTER_BOUND ( 'NONE', #4861, .T. ) ;
#13153 = ORIENTED_EDGE ( 'NONE', *, *, #7207, .T. ) ;
#13152 = CIRCLE ( 'NONE', #13723, 2.033421858999710619 ) ;
#13154 = LINE ( 'NONE', #24503, #29654 ) ;
#13155 = AXIS2_PLACEMENT_3D ( 'NONE', #32652, #27312, #274 ) ;
#13156 = DIRECTION ( 'NONE',  ( 0.000000000000000000, 0.000000000000000000, 1.000000000000000000 ) ) ;
#13157 = FACE_OUTER_BOUND ( 'NONE', #5922, .T. ) ;
#13158 = VECTOR ( 'NONE', #18191, 1000.000000000000000 ) ;
#13159 = VERTEX_POINT ( 'NONE', #19847 ) ;
#13160 = EDGE_LOOP ( 'NONE', ( #16926, #18776, #20340, #13686, #18608, #5113 ) ) ;
#13161 = CARTESIAN_POINT ( 'NONE',  ( 760.1504316191185353, 1307.440339905750307, 1753.598338701302964 ) ) ;
#13162 = ORIENTED_EDGE ( 'NONE', *, *, #31469, .T. ) ;
#13163 = CARTESIAN_POINT ( 'NONE',  ( 18.92820323027550344, -124.9999999999999432, -158.9999999999999716 ) ) ;
#13164 = AXIS2_PLACEMENT_3D ( 'NONE', #34041, #1646, #34570 ) ;
#13165 = CARTESIAN_POINT ( 'NONE',  ( -500.0000000000000000, -141.0000000000000000, 162.9999999999999716 ) ) ;
#13166 = CYLINDRICAL_SURFACE ( 'NONE', #9371, 4.309328216469825001 ) ;
#13167 = CYLINDRICAL_SURFACE ( 'NONE', #25572, 8.000000000000007105 ) ;
#13168 = ITEM_DEFINED_TRANSFORMATION ( 'NONE', 'NONE', #743,  #28566 ) ;
#13169 = ORIENTED_EDGE ( 'NONE', *, *, #15906, .F. ) ;
#13170 = LINE ( 'NONE', #21529, #23778 ) ;
#13172 = DIRECTION ( 'NONE',  ( 1.000000000000000000, 0.000000000000000000, 0.000000000000000000 ) ) ;
#13171 = DIRECTION ( 'NONE',  ( -0.5155538571770215128, 0.8568571761675892740, 0.000000000000000000 ) ) ;
#13174 = ORIENTED_EDGE ( 'NONE', *, *, #5463, .F. ) ;
#13173 = VECTOR ( 'NONE', #24672, 1000.000000000000000 ) ;
#13175 = VERTEX_POINT ( 'NONE', #27659 ) ;
#13176 = DIRECTION ( 'NONE',  ( 0.000000000000000000, 0.000000000000000000, 1.000000000000000000 ) ) ;
#13177 = VECTOR ( 'NONE', #14211, 1000.000000000000000 ) ;
#13178 = EDGE_CURVE ( 'NONE', #33934, #20222, #25336, .T. ) ;
#13179 = ORIENTED_EDGE ( 'NONE', *, *, #17273, .T. ) ;
#13180 = AXIS2_PLACEMENT_3D ( 'NONE', #12029, #6660, #25893 ) ;
#13181 = AXIS2_PLACEMENT_3D ( 'NONE', #18019, #1966, #21015 ) ;
#13182 = EDGE_CURVE ( 'NONE', #22127, #21805, #26672, .T. ) ;
#13183 = DIRECTION ( 'NONE',  ( -0.000000000000000000, 0.08715574274766170471, 0.9961946980917453232 ) ) ;
#13184 = LINE ( 'NONE', #29193, #5165 ) ;
#13185 = ORIENTED_EDGE ( 'NONE', *, *, #25983, .T. ) ;
#13186 = DIRECTION ( 'NONE',  ( 0.000000000000000000, 0.000000000000000000, 1.000000000000000000 ) ) ;
#13187 = EDGE_CURVE ( 'NONE', #26665, #23603, #20018, .T. ) ;
#13188 = CARTESIAN_POINT ( 'NONE',  ( 14.70109753509668948, 34.88954974633767137, -36.68877005347593467 ) ) ;
#13189 = ORIENTED_EDGE ( 'NONE', *, *, #17932, .T. ) ;
#13190 = EDGE_CURVE ( 'NONE', #10395, #21456, #3619, .T. ) ;
#13191 = FACE_OUTER_BOUND ( 'NONE', #708, .T. ) ;
#13192 = DIRECTION ( 'NONE',  ( 0.9476531711828023452, -0.3193015301359802827, -0.000000000000000000 ) ) ;
#13193 = AXIS2_PLACEMENT_3D ( 'NONE', #831, #9017, #20407 ) ;
#13194 = CARTESIAN_POINT ( 'NONE',  ( -10.00000000000000000, 0.000000000000000000, 0.000000000000000000 ) ) ;
#13196 = CARTESIAN_POINT ( 'NONE',  ( 2.789999999999999147, -31.68806325674604452, -4.003133335385915537 ) ) ;
#13195 = CARTESIAN_POINT ( 'NONE',  ( -418.0000000000000000, -105.0000000000000142, -155.0000000000000000 ) ) ;
#13197 = CARTESIAN_POINT ( 'NONE',  ( -445.9999999999999432, -105.0000000000000142, -77.99999999999997158 ) ) ;
#13198 = DIRECTION ( 'NONE',  ( 0.000000000000000000, 0.000000000000000000, 1.000000000000000000 ) ) ;
#13199 = DIRECTION ( 'NONE',  ( -1.000000000000000000, 0.000000000000000000, 0.000000000000000000 ) ) ;
#13200 = ADVANCED_FACE ( 'NONE', ( #14509 ), #24978, .T. ) ;
#13201 = AXIS2_PLACEMENT_3D ( 'NONE', #33983, #9438, #6572 ) ;
#13202 = EDGE_LOOP ( 'NONE', ( #20758, #12155 ) ) ;
#13203 = AXIS2_PLACEMENT_3D ( 'NONE', #1662, #34715, #1493 ) ;
#13204 = B_SPLINE_CURVE_WITH_KNOTS ( 'NONE', 3,
 ( #30862, #20369, #9671, #4143, #14861, #3799, #6467, #31559 ),
 .UNSPECIFIED., .F., .F.,
 ( 4, 2, 2, 4 ),
 ( 0.007886720825438786608, 0.009850969036563997708, 0.01181521724768920881, 0.01574371366993962754 ),
 .UNSPECIFIED. ) ;
#13205 = FACE_OUTER_BOUND ( 'NONE', #11636, .T. ) ;
#13206 = DIRECTION ( 'NONE',  ( 1.000000000000000000, 0.000000000000000000, 0.000000000000000000 ) ) ;
#13207 = AXIS2_PLACEMENT_3D ( 'NONE', #26480, #24154, #32341 ) ;
#13208 = UNCERTAINTY_MEASURE_WITH_UNIT (LENGTH_MEASURE( 1.000000000000000082E-05 ), #26894, 'distance_accuracy_value', 'NONE');
#13209 = VECTOR ( 'NONE', #29686, 1000.000000000000000 ) ;
#13210 = ORIENTED_EDGE ( 'NONE', *, *, #34109, .T. ) ;
#13211 = ORIENTED_EDGE ( 'NONE', *, *, #17782, .F. ) ;
#13212 = CARTESIAN_POINT ( 'NONE',  ( 20.73027531293552528, -10.15143121711728469, 20.00000000000000000 ) ) ;
#13213 = ORIENTED_EDGE ( 'NONE', *, *, #18459, .T. ) ;
#13214 = CARTESIAN_POINT ( 'NONE',  ( 36.10877985260814427, 11.38239727801116352, 68.31122994652405112 ) ) ;
#13215 = DIRECTION ( 'NONE',  ( 3.697785493223492838E-32, 1.934419779023891545E-16, -1.000000000000000000 ) ) ;
#13216 = DIRECTION ( 'NONE',  ( -1.000000000000000000, -0.000000000000000000, -0.000000000000000000 ) ) ;
#13217 = ORIENTED_EDGE ( 'NONE', *, *, #19511, .T. ) ;
#13218 = VERTEX_POINT ( 'NONE', #6111 ) ;
#13219 = DIRECTION ( 'NONE',  ( 0.000000000000000000, 0.000000000000000000, -1.000000000000000000 ) ) ;
#13220 = CLOSED_SHELL ( 'NONE', ( #31020, #31771, #4026, #27427, #26992, #25080, #20239, #18103, #12765, #857, #17289, #26550, #7582, #24003, #11320, #20974, #15491, #18656, #24778, #3115, #17396, #6164, #19459, #27512, #4718, #9088, #22555 ) ) ;
#13221 = CARTESIAN_POINT ( 'NONE',  ( -414.0000000000000568, -104.9999999999999858, -162.9999999999999716 ) ) ;
#13222 = EDGE_CURVE ( 'NONE', #30722, #17724, #16652, .T. ) ;
#13223 = DIRECTION ( 'NONE',  ( -0.6473862847818285804, -0.7621620551276356847, -0.000000000000000000 ) ) ;
#13224 = LINE ( 'NONE', #24404, #1755 ) ;
#13225 = DIRECTION ( 'NONE',  ( 1.000000000000000000, 0.000000000000000000, 0.000000000000000000 ) ) ;
#13226 = EDGE_LOOP ( 'NONE', ( #33738, #18960, #20944, #14319 ) ) ;
#13227 = DIRECTION ( 'NONE',  ( -1.000000000000000000, -0.000000000000000000, -0.000000000000000000 ) ) ;
#13228 = DIRECTION ( 'NONE',  ( 0.000000000000000000, 7.888609052210118054E-31, 1.000000000000000000 ) ) ;
#13229 = DIRECTION ( 'NONE',  ( -1.000000000000000000, 0.000000000000000000, 0.000000000000000000 ) ) ;
#13230 = VECTOR ( 'NONE', #24071, 1000.000000000000000 ) ;
#13231 = AXIS2_PLACEMENT_3D ( 'NONE', #4191, #1539, #30911 ) ;
#13232 = ADVANCED_FACE ( 'NONE', ( #11842 ), #22691, .F. ) ;
#13233 = PLANE ( 'NONE',  #11230 ) ;
#13234 = CARTESIAN_POINT ( 'NONE',  ( -418.0000000000000000, 109.0000000000000142, 154.9999999999999716 ) ) ;
#13235 = EDGE_CURVE ( 'NONE', #20173, #18637, #8445, .T. ) ;
#13236 = CARTESIAN_POINT ( 'NONE',  ( -262.5000000000000000, 1.224646799147353256E-15, -10.00000000000000000 ) ) ;
#13238 = CARTESIAN_POINT ( 'NONE',  ( 0.02407890056655695096, 30.61125888652961891, 5.439165181699118889 ) ) ;
#13237 = LINE ( 'NONE', #31897, #18469 ) ;
#13239 = EDGE_CURVE ( 'NONE', #22194, #33693, #30330, .T. ) ;
#13240 = EDGE_CURVE ( 'NONE', #17691, #19198, #31775, .T. ) ;
#13241 = CARTESIAN_POINT ( 'NONE',  ( 2.719051664055850637, 24.79283726477138217, -19.74402504231769129 ) ) ;
#13242 = ORIENTED_EDGE ( 'NONE', *, *, #14879, .T. ) ;
#13243 = CARTESIAN_POINT ( 'NONE',  ( 99.30025296260937751, 0.7624844131070424025, -12.48227001241056655 ) ) ;
#13244 = LINE ( 'NONE', #26928, #25950 ) ;
#13245 = ORIENTED_EDGE ( 'NONE', *, *, #24251, .T. ) ;
#13246 = CARTESIAN_POINT ( 'NONE',  ( 2.789999999999999147, 9.869977788041397915, -30.37666815053925973 ) ) ;
#13247 = ORIENTED_EDGE ( 'NONE', *, *, #22419, .T. ) ;
#13248 = ADVANCED_FACE ( 'NONE', ( #33888, #6990 ), #23545, .F. ) ;
#13249 = AXIS2_PLACEMENT_3D ( 'NONE', #6397, #16585, #27418 ) ;
#13250 = AXIS2_PLACEMENT_3D ( 'NONE', #22071, #11754, #8709 ) ;
#13251 = PRESENTATION_LAYER_ASSIGNMENT (  '', '', ( #23398 ) ) ;
#13252 = AXIS2_PLACEMENT_3D ( 'NONE', #27269, #30118, #5374 ) ;
#13253 = EDGE_LOOP ( 'NONE', ( #4347, #16089, #16877, #11176 ) ) ;
#13254 = DIRECTION ( 'NONE',  ( 1.000000000000000000, 0.000000000000000000, 0.000000000000000000 ) ) ;
#13255 = ORIENTED_EDGE ( 'NONE', *, *, #5554, .T. ) ;
#13256 = VERTEX_POINT ( 'NONE', #1490 ) ;
#13257 = CARTESIAN_POINT ( 'NONE',  ( 1.749999999999999778, 0.000000000000000000, 0.000000000000000000 ) ) ;
#13258 = ADVANCED_FACE ( 'NONE', ( #15376 ), #20198, .F. ) ;
#13260 = ADVANCED_FACE ( 'NONE', ( #23036 ), #4486, .T. ) ;
#13259 = DIRECTION ( 'NONE',  ( 0.000000000000000000, 0.000000000000000000, 1.000000000000000000 ) ) ;
#13261 = DIRECTION ( 'NONE',  ( 1.000000000000000000, 0.000000000000000000, 0.000000000000000000 ) ) ;
#13262 = EDGE_LOOP ( 'NONE', ( #21144, #206, #19035, #32374, #11903, #8173 ) ) ;
#13263 = ORIENTED_EDGE ( 'NONE', *, *, #24443, .T. ) ;
#13264 = CARTESIAN_POINT ( 'NONE',  ( -365.0000000000000000, 132.9999999999999716, 113.9999999999999858 ) ) ;
#13265 = DIRECTION ( 'NONE',  ( 0.000000000000000000, 0.000000000000000000, -1.000000000000000000 ) ) ;
#13266 = PLANE ( 'NONE',  #3931 ) ;
#13267 = FACE_OUTER_BOUND ( 'NONE', #20170, .T. ) ;
#13268 = VERTEX_POINT ( 'NONE', #25691 ) ;
#13269 = LINE ( 'NONE', #24275, #15694 ) ;
#13270 = AXIS2_PLACEMENT_3D ( 'NONE', #4145, #3445, #25518 ) ;
#13271 = PLANE ( 'NONE',  #34632 ) ;
#13272 = ORIENTED_EDGE ( 'NONE', *, *, #25574, .F. ) ;
#13273 = DIRECTION ( 'NONE',  ( -0.000000000000000000, 1.000000000000000000, 0.000000000000000000 ) ) ;
#13274 = DIRECTION ( 'NONE',  ( -0.000000000000000000, 0.000000000000000000, 1.000000000000000000 ) ) ;
#13275 = CARTESIAN_POINT ( 'NONE',  ( 11.99999999999999645, -141.0000000000000000, 174.9999999999999432 ) ) ;
#13276 = VERTEX_POINT ( 'NONE', #28714 ) ;
#13277 = AXIS2_PLACEMENT_3D ( 'NONE', #9614, #14792, #26144 ) ;
#13278 = LINE ( 'NONE', #34810, #29709 ) ;
#13279 = ORIENTED_EDGE ( 'NONE', *, *, #26224, .F. ) ;
#13280 = AXIS2_PLACEMENT_3D ( 'NONE', #1543, #841, #9385 ) ;
#13281 = ADVANCED_FACE ( 'NONE', ( #4315 ), #12526, .F. ) ;
#13282 = ADVANCED_FACE ( 'NONE', ( #31556 ), #20367, .T. ) ;
#13283 = AXIS2_PLACEMENT_3D ( 'NONE', #7295, #13022, #1451 ) ;
#13284 = DIRECTION ( 'NONE',  ( 0.000000000000000000, -1.000000000000000000, -1.224646799147353207E-16 ) ) ;
#13285 = ORIENTED_EDGE ( 'NONE', *, *, #15548, .T. ) ;
#13287 = FACE_OUTER_BOUND ( 'NONE', #16367, .T. ) ;
#13286 = CARTESIAN_POINT ( 'NONE',  ( 0.006892432010618929766, -3.550547054313539341, -30.66493323461388698 ) ) ;
#13288 = FILL_AREA_STYLE_COLOUR ( '', #12571 ) ;
#13289 = ORIENTED_EDGE ( 'NONE', *, *, #4561, .F. ) ;
#13290 = DIRECTION ( 'NONE',  ( -0.000000000000000000, -1.000000000000000000, -0.000000000000000000 ) ) ;
#13291 = CARTESIAN_POINT ( 'NONE',  ( 42.44043929807611448, -20.15143121711728469, 20.00000000000000000 ) ) ;
#13292 = ORIENTED_EDGE ( 'NONE', *, *, #33893, .F. ) ;
#13293 = EDGE_CURVE ( 'NONE', #27359, #11247, #4141, .T. ) ;
#13294 = CIRCLE ( 'NONE', #20678, 2.525000000000000355 ) ;
#13295 = CARTESIAN_POINT ( 'NONE',  ( 771.9066388424148499, 1197.567557597692257, 1753.598338701304101 ) ) ;
#13296 = VERTEX_POINT ( 'NONE', #31045 ) ;
#13297 = CARTESIAN_POINT ( 'NONE',  ( -106.3655922539543326, 4.941456866685308924, 5.642756420309243737 ) ) ;
#13298 = ORIENTED_EDGE ( 'NONE', *, *, #18967, .F. ) ;
#13299 = FACE_BOUND ( 'NONE', #33843, .T. ) ;
#13300 = EDGE_CURVE ( 'NONE', #33860, #6574, #2805, .T. ) ;
#13301 = EDGE_CURVE ( 'NONE', #8875, #29676, #25874, .T. ) ;
#13302 = AXIS2_PLACEMENT_3D ( 'NONE', #9909, #28434, #25756 ) ;
#13303 = EDGE_CURVE ( 'NONE', #34313, #13897, #34232, .T. ) ;
#13304 = AXIS2_PLACEMENT_3D ( 'NONE', #10380, #7517, #21236 ) ;
#13305 = CARTESIAN_POINT ( 'NONE',  ( -107.5877143847361452, -4.424201595130941023, -6.060139114164995178 ) ) ;
#13306 = DIRECTION ( 'NONE',  ( 0.000000000000000000, 1.000000000000000000, 1.934419779023891545E-16 ) ) ;
#13307 = ORIENTED_EDGE ( 'NONE', *, *, #12239, .F. ) ;
#13308 = ORIENTED_EDGE ( 'NONE', *, *, #18257, .F. ) ;
#13309 = CIRCLE ( 'NONE', #30365, 2.036051781435508801 ) ;
#13310 = PRODUCT_DEFINITION_SHAPE ( 'NONE', 'NONE',  #35241 ) ;
#13311 = ORIENTED_EDGE ( 'NONE', *, *, #16050, .F. ) ;
#13312 = DIRECTION ( 'NONE',  ( 1.000000000000000000, 0.000000000000000000, -1.232595164407831220E-32 ) ) ;
#13313 = LINE ( 'NONE', #5448, #6082 ) ;
#13314 = ADVANCED_FACE ( 'NONE', ( #9669 ), #9843, .F. ) ;
#13315 = CARTESIAN_POINT ( 'NONE',  ( 0.02407890056655651728, -3.506335382740735529, 30.89238256715863784 ) ) ;
#13316 = CARTESIAN_POINT ( 'NONE',  ( 1.395000000000002238, 32.09669216789236401, 12.41728656686386500 ) ) ;
#13317 = PLANE ( 'NONE',  #4552 ) ;
#13318 = CARTESIAN_POINT ( 'NONE',  ( -8.267476927982267298, 31.47782073335735831, 68.31122994652405112 ) ) ;
#13319 = PLANE ( 'NONE',  #2204 ) ;
#13320 = ORIENTED_EDGE ( 'NONE', *, *, #25602, .F. ) ;
#13321 = DIRECTION ( 'NONE',  ( -1.000000000000000000, -0.000000000000000000, -0.000000000000000000 ) ) ;
#13322 = DIRECTION ( 'NONE',  ( 1.000000000000000000, 0.000000000000000000, 0.000000000000000000 ) ) ;
#13323 = CARTESIAN_POINT ( 'NONE',  ( 1.749999999999999778, 31.89769921723006263, -12.91988538846924151 ) ) ;
#13324 = VERTEX_POINT ( 'NONE', #9325 ) ;
#13325 = AXIS2_PLACEMENT_3D ( 'NONE', #32318, #18646, #34654 ) ;
#13326 = CARTESIAN_POINT ( 'NONE',  ( -442.0000000000000000, 141.0000000000000000, -175.0000000000000000 ) ) ;
#13327 = ORIENTED_EDGE ( 'NONE', *, *, #30783, .F. ) ;
#13328 = CIRCLE ( 'NONE', #9356, 1.999999999999999112 ) ;
#13329 = CARTESIAN_POINT ( 'NONE',  ( -108.1248180926981632, 4.063332493481114582, -11.82279441766105599 ) ) ;
#13330 = CYLINDRICAL_SURFACE ( 'NONE', #17312, 7.999999999999979572 ) ;
#13331 = CARTESIAN_POINT ( 'NONE',  ( -29.72561944762171393, -13.25111019240559251, 68.31122994652405112 ) ) ;
#13332 = ORIENTED_EDGE ( 'NONE', *, *, #34592, .T. ) ;
#13333 = AXIS2_PLACEMENT_3D ( 'NONE', #8943, #6609, #19815 ) ;
#13334 = DIRECTION ( 'NONE',  ( -1.000000000000000000, -0.000000000000000000, -0.000000000000000000 ) ) ;
#13335 = CARTESIAN_POINT ( 'NONE',  ( -5.210000000000000853, 0.000000000000000000, 0.000000000000000000 ) ) ;
#13336 = FACE_OUTER_BOUND ( 'NONE', #25393, .T. ) ;
#13337 = AXIS2_PLACEMENT_3D ( 'NONE', #21526, #29360, #15489 ) ;
#13338 = VERTEX_POINT ( 'NONE', #28885 ) ;
#13339 = ORIENTED_EDGE ( 'NONE', *, *, #31613, .T. ) ;
#13340 = DIRECTION ( 'NONE',  ( -0.1063910735369017202, 0.9943243633099136947, -1.000770725407181676E-14 ) ) ;
#13341 =( REPRESENTATION_RELATIONSHIP ('NONE','NONE', #23037, #28231 ) REPRESENTATION_RELATIONSHIP_WITH_TRANSFORMATION ( #11113 )SHAPE_REPRESENTATION_RELATIONSHIP( ) );
#13342 = FACE_OUTER_BOUND ( 'NONE', #34635, .T. ) ;
#13343 = VERTEX_POINT ( 'NONE', #6642 ) ;
#13344 = DIRECTION ( 'NONE',  ( 1.000000000000000000, 0.000000000000000000, 0.000000000000000000 ) ) ;
#13345 = EDGE_CURVE ( 'NONE', #32269, #18432, #17540, .T. ) ;
#13346 = CARTESIAN_POINT ( 'NONE',  ( 4.748287528889715493E-15, 32.54542015209057837, -87.50000000000000000 ) ) ;
#13347 = ADVANCED_FACE ( 'NONE', ( #3340 ), #1033, .T. ) ;
#13348 = AXIS2_PLACEMENT_3D ( 'NONE', #5563, #8956, #19830 ) ;
#13349 = CARTESIAN_POINT ( 'NONE',  ( 5.021133111224576062, 14.09580098603202458, -67.50000000000000000 ) ) ;
#13350 = CARTESIAN_POINT ( 'NONE',  ( -102.6980701398429403, -4.579683091146231178, 5.941712070794215705 ) ) ;
#13351 = VERTEX_POINT ( 'NONE', #25757 ) ;
#13352 = CARTESIAN_POINT ( 'NONE',  ( -442.0000000000000000, -109.0000000000000142, -174.9999999999999716 ) ) ;
#13353 = CYLINDRICAL_SURFACE ( 'NONE', #20337, 2.524999999999999467 ) ;
#13355 = DIRECTION ( 'NONE',  ( -1.000000000000000000, -0.000000000000000000, -0.000000000000000000 ) ) ;
#13354 = LINE ( 'NONE', #24188, #16201 ) ;
#13356 = CIRCLE ( 'NONE', #17917, 3.999999999999976019 ) ;
#13357 = EDGE_LOOP ( 'NONE', ( #15065, #32264, #326, #35078 ) ) ;
#13358 = ORIENTED_EDGE ( 'NONE', *, *, #24493, .F. ) ;
#13359 = VECTOR ( 'NONE', #10706, 1000.000000000000114 ) ;
#13360 = LINE ( 'NONE', #13009, #4933 ) ;
#13361 = VERTEX_POINT ( 'NONE', #9400 ) ;
#13362 = FACE_OUTER_BOUND ( 'NONE', #34890, .T. ) ;
#13363 = DIRECTION ( 'NONE',  ( 1.000000000000000000, 0.000000000000000000, 0.000000000000000000 ) ) ;
#13364 = EDGE_LOOP ( 'NONE', ( #21199, #14823, #6385, #12754 ) ) ;
#13365 = DIRECTION ( 'NONE',  ( 0.000000000000000000, 1.000000000000000000, 5.145227585319922065E-49 ) ) ;
#13366 = CARTESIAN_POINT ( 'NONE',  ( -20.00000000000007461, 112.9999999999999574, -187.0000000000000000 ) ) ;
#13367 = ORIENTED_EDGE ( 'NONE', *, *, #1342, .F. ) ;
#13368 = DIRECTION ( 'NONE',  ( 0.000000000000000000, 1.836970198721029441E-16, -1.000000000000000000 ) ) ;
#13369 = CARTESIAN_POINT ( 'NONE',  ( -349.0000000000000000, -135.0000000000000000, 113.9999999999999858 ) ) ;
#13370 = CYLINDRICAL_SURFACE ( 'NONE', #7006, 34.41491905851385269 ) ;
#13371 = CARTESIAN_POINT ( 'NONE',  ( 19.99999999999998224, 144.9999999999999716, -162.9999999999999432 ) ) ;
#13372 = CIRCLE ( 'NONE', #25854, 7.999999999999992895 ) ;
#13373 = CARTESIAN_POINT ( 'NONE',  ( 19.99999999999998934, 75.55999999999990280, -168.2400000000000091 ) ) ;
#13374 = CARTESIAN_POINT ( 'NONE',  ( -0.9727285265192152641, -1.747512292859696670, 0.000000000000000000 ) ) ;
#13375 = CARTESIAN_POINT ( 'NONE',  ( 11.99999999999999645, -55.00000000000000711, 162.9999999999999716 ) ) ;
#13376 = VECTOR ( 'NONE', #16120, 1000.000000000000114 ) ;
#13377 = ORIENTED_EDGE ( 'NONE', *, *, #31577, .T. ) ;
#13379 = AXIS2_PLACEMENT_3D ( 'NONE', #31147, #3199, #28117 ) ;
#13378 = DIRECTION ( 'NONE',  ( -0.000000000000000000, 1.836970198721029688E-16, -1.000000000000000000 ) ) ;
#13380 = DIRECTION ( 'NONE',  ( -0.3821446942676031133, 0.9241025011561869729, 9.267623407333104135E-15 ) ) ;
#13381 = ORIENTED_EDGE ( 'NONE', *, *, #26035, .F. ) ;
#13382 = AXIS2_PLACEMENT_3D ( 'NONE', #618, #30699, #28382 ) ;
#13383 = ORIENTED_EDGE ( 'NONE', *, *, #11222, .F. ) ;
#13384 = ADVANCED_FACE ( 'NONE', ( #14576 ), #27898, .T. ) ;
#13385 = ADVANCED_FACE ( 'NONE', ( #17434, #22394 ), #3511, .T. ) ;
#13386 = DIRECTION ( 'NONE',  ( 0.000000000000000000, 0.000000000000000000, 1.000000000000000000 ) ) ;
#13387 = DIRECTION ( 'NONE',  ( 2.631201909438060585E-14, -5.396010391056496978E-16, 1.000000000000000000 ) ) ;
#13388 = ORIENTED_EDGE ( 'NONE', *, *, #22996, .F. ) ;
#13389 = PRODUCT_DEFINITION ( 'UNKNOWN', '', #12196, #27440 ) ;
#13390 = CARTESIAN_POINT ( 'NONE',  ( -45.00000000000000000, -46.95407462254104303, -36.69637551990492597 ) ) ;
#13391 = DIRECTION ( 'NONE',  ( 0.8276889981568903432, -0.5611870653623828309, 0.000000000000000000 ) ) ;
#13392 = ITEM_DEFINED_TRANSFORMATION ( 'NONE', 'NONE', #17857,  #28566 ) ;
#13393 = VECTOR ( 'NONE', #23076, 1000.000000000000000 ) ;
#13394 = FACE_BOUND ( 'NONE', #27036, .T. ) ;
#13395 = ORIENTED_EDGE ( 'NONE', *, *, #20099, .F. ) ;
#13396 = VERTEX_POINT ( 'NONE', #14217 ) ;
#13397 = DIRECTION ( 'NONE',  ( -0.4198891015602651544, 0.9075754196709567845, 0.000000000000000000 ) ) ;
#13398 = VECTOR ( 'NONE', #33529, 1000.000000000000000 ) ;
#13399 = DIRECTION ( 'NONE',  ( -0.000000000000000000, -0.000000000000000000, 1.000000000000000000 ) ) ;
#13400 = CARTESIAN_POINT ( 'NONE',  ( 0.000000000000000000, 2.005524111408653720, -31.87689292423236154 ) ) ;
#13401 = CARTESIAN_POINT ( 'NONE',  ( 0.5248942638477641642, 14.91070698422159779, 29.86438609618750561 ) ) ;
#13402 = PLANE ( 'NONE',  #17722 ) ;
#13403 = ORIENTED_EDGE ( 'NONE', *, *, #8543, .F. ) ;
#13404 = CARTESIAN_POINT ( 'NONE',  ( -12.00000000000001066, 124.9999999999999716, 190.9999999999999716 ) ) ;
#13405 = DIRECTION ( 'NONE',  ( -0.4684084406997903738, -0.8835120444460228262, -1.622985295858433536E-16 ) ) ;
#13406 = CARTESIAN_POINT ( 'NONE',  ( 2.789999999999999147, -17.95514392185434360, 25.38201125280350468 ) ) ;
#13407 = VECTOR ( 'NONE', #25828, 1000.000000000000000 ) ;
#13408 = DIRECTION ( 'NONE',  ( -1.000000000000000000, 0.000000000000000000, 0.000000000000000000 ) ) ;
#13409 = CARTESIAN_POINT ( 'NONE',  ( 11.99999999999995559, -134.9999999999999716, -162.9999999999999432 ) ) ;
#13410 = DIRECTION ( 'NONE',  ( 0.000000000000000000, 0.000000000000000000, 1.000000000000000000 ) ) ;
#13412 = CARTESIAN_POINT ( 'NONE',  ( -11.99999999999998224, -134.9999999999999716, 162.9999999999999716 ) ) ;
#13411 = CARTESIAN_POINT ( 'NONE',  ( 0.000000000000000000, 3.004629197474321612E-15, 13.50000000000000000 ) ) ;
#13413 = DIRECTION ( 'NONE',  ( -1.000000000000000000, -0.000000000000000000, -0.000000000000000000 ) ) ;
#13414 = ORIENTED_EDGE ( 'NONE', *, *, #14391, .T. ) ;
#13415 = DIRECTION ( 'NONE',  ( 3.697785493223492838E-32, 1.934419779023891545E-16, -1.000000000000000000 ) ) ;
#13417 = CARTESIAN_POINT ( 'NONE',  ( -500.0000000000000000, -105.0000000000000142, 187.0000000000000000 ) ) ;
#13416 = CARTESIAN_POINT ( 'NONE',  ( 8.000000000000000000, 0.000000000000000000, 0.000000000000000000 ) ) ;
#13418 = AXIS2_PLACEMENT_3D ( 'NONE', #23360, #28185, #34219 ) ;
#13419 = EDGE_LOOP ( 'NONE', ( #23438, #17052, #26256, #3301 ) ) ;
#13420 = CARTESIAN_POINT ( 'NONE',  ( -12.00000000000001066, -24.99999999999999289, -175.0000000000000000 ) ) ;
#13421 = CIRCLE ( 'NONE', #20807, 2.036051781435508801 ) ;
#13422 = ORIENTED_EDGE ( 'NONE', *, *, #31452, .T. ) ;
#13423 = ADVANCED_FACE ( 'NONE', ( #860 ), #33592, .F. ) ;
#13424 = VERTEX_POINT ( 'NONE', #14401 ) ;
#13425 = CARTESIAN_POINT ( 'NONE',  ( 0.000000000000000000, 2.281310696040539424E-14, -36.68877005347592757 ) ) ;
#13426 = ORIENTED_EDGE ( 'NONE', *, *, #3698, .F. ) ;
#13427 = ORIENTED_EDGE ( 'NONE', *, *, #31469, .F. ) ;
#13428 = EDGE_CURVE ( 'NONE', #23263, #1567, #25483, .T. ) ;
#13429 = DIRECTION ( 'NONE',  ( -1.000000000000000000, -0.000000000000000000, -0.000000000000000000 ) ) ;
#13430 = AXIS2_PLACEMENT_3D ( 'NONE', #24904, #19592, #30437 ) ;
#13431 = LINE ( 'NONE', #27473, #29434 ) ;
#13432 = CARTESIAN_POINT ( 'NONE',  ( 50.00050000000000239, 0.000000000000000000, 0.000000000000000000 ) ) ;
#13433 = ORIENTED_EDGE ( 'NONE', *, *, #26467, .T. ) ;
#13434 = EDGE_CURVE ( 'NONE', #10218, #5629, #25403, .T. ) ;
#13435 = ORIENTED_EDGE ( 'NONE', *, *, #3240, .T. ) ;
#13436 = CARTESIAN_POINT ( 'NONE',  ( 12.46788440507150320, 30.06253867087537657, 68.31122994652405112 ) ) ;
#13437 = CARTESIAN_POINT ( 'NONE',  ( 0.000000000000000000, 3.524919873834583163E-15, 68.31122994652405112 ) ) ;
#13438 = ADVANCED_FACE ( 'NONE', ( #19909 ), #22921, .F. ) ;
#13439 = CARTESIAN_POINT ( 'NONE',  ( -6.500000000000000000, 0.000000000000000000, 3.180000000000000160 ) ) ;
#13440 = LINE ( 'NONE', #11124, #14289 ) ;
#13441 = VERTEX_POINT ( 'NONE', #30751 ) ;
#13442 = AXIS2_PLACEMENT_3D ( 'NONE', #22847, #33694, #31035 ) ;
#13443 = DIRECTION ( 'NONE',  ( 0.000000000000000000, 0.000000000000000000, 1.000000000000000000 ) ) ;
#13444 = DIRECTION ( 'NONE',  ( 0.000000000000000000, 4.122115190439938353E-15, -1.000000000000000000 ) ) ;
#13445 = VERTEX_POINT ( 'NONE', #20262 ) ;
#13446 = DIRECTION ( 'NONE',  ( 8.433758354584418579E-81, -1.000000000000000000, -3.421138828918010427E-49 ) ) ;
#13447 = CARTESIAN_POINT ( 'NONE',  ( -349.0000000000000000, 134.9999999999999716, 128.0000000000000000 ) ) ;
#13448 = CARTESIAN_POINT ( 'NONE',  ( 2.606461794449805858, -30.93445778156022641, -9.191712967691181291 ) ) ;
#13449 = ORIENTED_EDGE ( 'NONE', *, *, #15855, .T. ) ;
#13450 = LINE ( 'NONE', #24281, #4103 ) ;
#13451 = VERTEX_POINT ( 'NONE', #19730 ) ;
#13452 = CARTESIAN_POINT ( 'NONE',  ( 19.99999999999996092, -134.9999999999999716, 162.9999999999999716 ) ) ;
#13453 = ORIENTED_EDGE ( 'NONE', *, *, #31449, .T. ) ;
#13454 = CARTESIAN_POINT ( 'NONE',  ( 19.99999999999998224, -55.00000000000000711, -158.9999999999999716 ) ) ;
#13455 = DIRECTION ( 'NONE',  ( 0.000000000000000000, -1.000000000000000000, 0.000000000000000000 ) ) ;
#13456 = ORIENTED_EDGE ( 'NONE', *, *, #4477, .F. ) ;
#13457 = FACE_OUTER_BOUND ( 'NONE', #28066, .T. ) ;
#13458 = DIRECTION ( 'NONE',  ( 0.000000000000000000, 1.000000000000000000, -2.225651257388386197E-16 ) ) ;
#13459 = VECTOR ( 'NONE', #10152, 1000.000000000000000 ) ;
#13460 = ORIENTED_EDGE ( 'NONE', *, *, #29540, .F. ) ;
#13461 = VECTOR ( 'NONE', #4744, 1000.000000000000000 ) ;
#13462 = ORIENTED_EDGE ( 'NONE', *, *, #10951, .T. ) ;
#13463 = FACE_OUTER_BOUND ( 'NONE', #27191, .T. ) ;
#13464 = CARTESIAN_POINT ( 'NONE',  ( -107.2958507442938014, 4.573766672917669140, 5.944761500833684487 ) ) ;
#13465 = ORIENTED_EDGE ( 'NONE', *, *, #4767, .F. ) ;
#13466 = ORIENTED_EDGE ( 'NONE', *, *, #25680, .T. ) ;
#13467 = DIRECTION ( 'NONE',  ( 1.000000000000000000, 0.000000000000000000, 1.300283923313630633E-47 ) ) ;
#13468 = EDGE_CURVE ( 'NONE', #32774, #17833, #25554, .T. ) ;
#13469 = CARTESIAN_POINT ( 'NONE',  ( -100.6805073636512589, -2.744499711777490081, -6.981349484866706590 ) ) ;
#13470 = DIRECTION ( 'NONE',  ( 0.000000000000000000, 0.000000000000000000, -1.000000000000000000 ) ) ;
#13471 = EDGE_CURVE ( 'NONE', #20282, #12420, #17634, .T. ) ;
#13472 = ORIENTED_EDGE ( 'NONE', *, *, #28939, .F. ) ;
#13473 = ADVANCED_FACE ( 'NONE', ( #22750 ), #31111, .T. ) ;
#13474 = VERTEX_POINT ( 'NONE', #9215 ) ;
#13475 = ORIENTED_EDGE ( 'NONE', *, *, #9337, .F. ) ;
#13476 = DIRECTION ( 'NONE',  ( 1.000000000000000000, 0.000000000000000000, 0.000000000000000000 ) ) ;
#13477 = AXIS2_PLACEMENT_3D ( 'NONE', #26460, #1900, #29131 ) ;
#13478 = DIRECTION ( 'NONE',  ( -1.000000000000000000, -0.000000000000000000, -0.000000000000000000 ) ) ;
#13479 = DIRECTION ( 'NONE',  ( -1.000000000000000000, 0.000000000000000000, 0.000000000000000000 ) ) ;
#13480 = DIRECTION ( 'NONE',  ( -0.000000000000000000, 1.000000000000000000, -0.000000000000000000 ) ) ;
#13481 = CARTESIAN_POINT ( 'NONE',  ( 12.00000000000001066, -134.9999999999999716, 155.0000000000000000 ) ) ;
#13482 = DIRECTION ( 'NONE',  ( 0.000000000000000000, 0.000000000000000000, 1.000000000000000000 ) ) ;
#13483 = FACE_BOUND ( 'NONE', #6967, .T. ) ;
#13484 = VERTEX_POINT ( 'NONE', #17605 ) ;
#13485 = AXIS2_PLACEMENT_3D ( 'NONE', #25604, #22947, #28457 ) ;
#13486 = FACE_BOUND ( 'NONE', #12294, .T. ) ;
#13487 = CYLINDRICAL_SURFACE ( 'NONE', #14913, 7.999999999999979572 ) ;
#13488 = ADVANCED_FACE ( 'NONE', ( #6174 ), #28435, .F. ) ;
#13489 = FACE_OUTER_BOUND ( 'NONE', #2869, .T. ) ;
#13490 = EDGE_LOOP ( 'NONE', ( #27023, #14891, #23412, #861 ) ) ;
#13491 = AXIS2_PLACEMENT_3D ( 'NONE', #3963, #10020, #31553 ) ;
#13492 = CARTESIAN_POINT ( 'NONE',  ( 0.000000000000000000, 30.40449935640659973, -2.004522720844279959 ) ) ;
#13493 = EDGE_LOOP ( 'NONE', ( #10927, #31887, #25141, #12339 ) ) ;
#13494 = CARTESIAN_POINT ( 'NONE',  ( -100.5730760456114865, 2.567831768330361530, -12.23432884111322316 ) ) ;
#13495 = EDGE_CURVE ( 'NONE', #21641, #143, #30402, .T. ) ;
#13496 = CARTESIAN_POINT ( 'NONE',  ( 10.00000000000000000, -1.505030548027689319, 3.180000000000000160 ) ) ;
#13497 = AXIS2_PLACEMENT_3D ( 'NONE', #31591, #25909, #10059 ) ;
#13498 = EDGE_CURVE ( 'NONE', #15995, #10280, #27726, .T. ) ;
#13499 = ORIENTED_EDGE ( 'NONE', *, *, #5372, .F. ) ;
#13500 = CYLINDRICAL_SURFACE ( 'NONE', #17740, 7.999999999999979572 ) ;
#13501 = LINE ( 'NONE', #24336, #3148 ) ;
#13502 = DIRECTION ( 'NONE',  ( -0.000000000000000000, -0.000000000000000000, 1.000000000000000000 ) ) ;
#13503 = EDGE_CURVE ( 'NONE', #33936, #509, #9353, .T. ) ;
#13504 = ORIENTED_EDGE ( 'NONE', *, *, #1438, .F. ) ;
#13505 = ORIENTED_EDGE ( 'NONE', *, *, #12554, .T. ) ;
#13506 = VECTOR ( 'NONE', #16857, 1000.000000000000000 ) ;
#13507 = DIRECTION ( 'NONE',  ( -7.893605728314050488E-14, 1.618803117314786135E-15, 0.9999999999999998890 ) ) ;
#13508 = CARTESIAN_POINT ( 'NONE',  ( 1.040000000000002922, -34.41385771548413430, 0.2702793785568980978 ) ) ;
#13509 = VERTEX_POINT ( 'NONE', #17957 ) ;
#13510 = LINE ( 'NONE', #21860, #26025 ) ;
#13511 = DIRECTION ( 'NONE',  ( -1.000000000000000000, -0.000000000000000000, -0.000000000000000000 ) ) ;
#13512 = AXIS2_PLACEMENT_3D ( 'NONE', #8925, #19627, #6235 ) ;
#13513 = AXIS2_PLACEMENT_3D ( 'NONE', #30368, #2953, #33212 ) ;
#13514 = CARTESIAN_POINT ( 'NONE',  ( 0.0001801434340936737804, -25.83993731729792742, -16.24881338200996694 ) ) ;
#13515 = CARTESIAN_POINT ( 'NONE',  ( -45.00000000000000000, 3.353962854566122864, 15.81122994652406355 ) ) ;
#13516 = ITEM_DEFINED_TRANSFORMATION ( 'NONE', 'NONE', #13277,  #28566 ) ;
#13517 = EDGE_CURVE ( 'NONE', #9925, #11163, #20948, .T. ) ;
#13518 = VERTEX_POINT ( 'NONE', #10260 ) ;
#13519 = EDGE_CURVE ( 'NONE', #18998, #13672, #9073, .T. ) ;
#13520 = VERTEX_POINT ( 'NONE', #7227 ) ;
#13521 = CARTESIAN_POINT ( 'NONE',  ( 9.199999999999999289, 15.58845726811990495, 0.000000000000000000 ) ) ;
#13522 = AXIS2_PLACEMENT_3D ( 'NONE', #31758, #7367, #1530 ) ;
#13524 = CARTESIAN_POINT ( 'NONE',  ( 99.26191511054601335, -2.804307960831458189E-14, 7.500000000000241585 ) ) ;
#13523 = LINE ( 'NONE', #24523, #34968 ) ;
#13525 = ORIENTED_EDGE ( 'NONE', *, *, #9542, .F. ) ;
#13526 = ORIENTED_EDGE ( 'NONE', *, *, #5604, .T. ) ;
#13527 = CARTESIAN_POINT ( 'NONE',  ( -12.00000000000001066, 112.9999999999999574, 155.0000000000000000 ) ) ;
#13528 = VERTEX_POINT ( 'NONE', #18131 ) ;
#13529 = LINE ( 'NONE', #2661, #13002 ) ;
#13530 = LINE ( 'NONE', #24366, #16588 ) ;
#13531 = VERTEX_POINT ( 'NONE', #7574 ) ;
#13532 = ORIENTED_EDGE ( 'NONE', *, *, #8928, .T. ) ;
#13533 = CARTESIAN_POINT ( 'NONE',  ( -418.0000000000000000, -105.0000000000000142, 107.9999999999999858 ) ) ;
#13534 = VECTOR ( 'NONE', #2554, 1000.000000000000114 ) ;
#13535 = DIRECTION ( 'NONE',  ( 1.000000000000000000, 3.469446951953834515E-18, 0.000000000000000000 ) ) ;
#13536 = ORIENTED_EDGE ( 'NONE', *, *, #8436, .T. ) ;
#13537 = CARTESIAN_POINT ( 'NONE',  ( 0.000000000000000000, 0.000000000000000000, 5.429999999999999716 ) ) ;
#13538 = DIRECTION ( 'NONE',  ( 0.000000000000000000, 1.000000000000000000, 5.053935297177146739E-49 ) ) ;
#13539 = CARTESIAN_POINT ( 'NONE',  ( -32.54223829851967764, 0.4550817492056293823, -36.68877005347593467 ) ) ;
#13540 = EDGE_CURVE ( 'NONE', #763, #27942, #28781, .T. ) ;
#13541 = CARTESIAN_POINT ( 'NONE',  ( -5.021133111224679091, 24.02303923978504940, -67.50000000000000000 ) ) ;
#13542 = AXIS2_PLACEMENT_3D ( 'NONE', #6941, #6774, #1963 ) ;
#13543 = AXIS2_PLACEMENT_3D ( 'NONE', #907, #27947, #19427 ) ;
#13544 = EDGE_CURVE ( 'NONE', #30505, #9756, #33108, .T. ) ;
#13545 =( REPRESENTATION_RELATIONSHIP ('NONE','NONE', #23037, #28231 ) REPRESENTATION_RELATIONSHIP_WITH_TRANSFORMATION ( #4639 )SHAPE_REPRESENTATION_RELATIONSHIP( ) );
#13546 = DIRECTION ( 'NONE',  ( 0.000000000000000000, 0.000000000000000000, 1.000000000000000000 ) ) ;
#13547 = DIRECTION ( 'NONE',  ( 1.000000000000000000, 0.000000000000000000, -1.232595164407831220E-32 ) ) ;
#13548 = CARTESIAN_POINT ( 'NONE',  ( 2.789999999999999147, 24.98605633783575897, 17.38589710834512658 ) ) ;
#13549 = AXIS2_PLACEMENT_3D ( 'NONE', #16601, #6558, #9060 ) ;
#13550 = ORIENTED_EDGE ( 'NONE', *, *, #24252, .F. ) ;
#13551 = CARTESIAN_POINT ( 'NONE',  ( 0.000000000000000000, -11.13185981125894486, 28.36429779836949194 ) ) ;
#13552 = DIRECTION ( 'NONE',  ( 0.8802570610565354503, -0.4744971090113307977, -9.690914676546728526E-15 ) ) ;
#13553 = EDGE_CURVE ( 'NONE', #20910, #10814, #14215, .T. ) ;
#13554 = ORIENTED_EDGE ( 'NONE', *, *, #32660, .F. ) ;
#13555 = ORIENTED_EDGE ( 'NONE', *, *, #26917, .F. ) ;
#13556 = VECTOR ( 'NONE', #12656, 1000.000000000000000 ) ;
#13557 = CIRCLE ( 'NONE', #10143, 7.999999999999979572 ) ;
#13558 = CARTESIAN_POINT ( 'NONE',  ( 1.749999999999999778, 0.000000000000000000, 0.000000000000000000 ) ) ;
#13559 = CONTEXT_DEPENDENT_SHAPE_REPRESENTATION ( #3497, #16907 ) ;
#13560 = ORIENTED_EDGE ( 'NONE', *, *, #4669, .T. ) ;
#13561 = FACE_OUTER_BOUND ( 'NONE', #12570, .T. ) ;
#13562 = SURFACE_STYLE_USAGE ( .BOTH. , #2692 ) ;
#13563 = CONTEXT_DEPENDENT_SHAPE_REPRESENTATION ( #8539, #14511 ) ;
#13564 = VECTOR ( 'NONE', #18525, 1000.000000000000000 ) ;
#13565 = DIRECTION ( 'NONE',  ( -0.000000000000000000, -0.000000000000000000, -1.000000000000000000 ) ) ;
#13566 = EDGE_LOOP ( 'NONE', ( #13599, #21130, #9656, #16415 ) ) ;
#13567 = EDGE_LOOP ( 'NONE', ( #8524, #21708, #31458, #34872, #6024, #28151 ) ) ;
#13568 = CARTESIAN_POINT ( 'NONE',  ( 1.532562817202168137, 32.50931595846690669, 68.31122994652405112 ) ) ;
#13570 = EDGE_CURVE ( 'NONE', #11101, #1704, #13637, .T. ) ;
#13569 = DIRECTION ( 'NONE',  ( 0.9985334138511240409, -0.05413890858541543089, -9.945156166269024927E-18 ) ) ;
#13571 = CARTESIAN_POINT ( 'NONE',  ( 0.7181323043387221050, -1.866624223957557893, 5.429999999999999716 ) ) ;
#13572 = LINE ( 'NONE', #2179, #10858 ) ;
#13573 = CARTESIAN_POINT ( 'NONE',  ( -10.00000000000000000, 0.000000000000000000, 0.000000000000000000 ) ) ;
#13574 = EDGE_LOOP ( 'NONE', ( #29565, #8088, #15285, #537 ) ) ;
#13575 = TOROIDAL_SURFACE ( 'NONE', #26649, 13.00000000000000000, 1.799999999999999822 ) ;
#13576 = CARTESIAN_POINT ( 'NONE',  ( -418.0000000000000000, -104.9999999999999716, -187.0000000000000000 ) ) ;
#13577 = CARTESIAN_POINT ( 'NONE',  ( -499.9999999999999432, 112.9999999999999574, -190.9999999999999716 ) ) ;
#13578 = FACE_OUTER_BOUND ( 'NONE', #10190, .T. ) ;
#13579 = DIRECTION ( 'NONE',  ( 1.000000000000000000, 0.000000000000000000, 0.000000000000000000 ) ) ;
#13580 = ADVANCED_FACE ( 'NONE', ( #16674 ), #13119, .T. ) ;
#13581 = CARTESIAN_POINT ( 'NONE',  ( 0.1835382038249109005, 7.231184547465314694, 31.45056812073516994 ) ) ;
#13582 = FACE_OUTER_BOUND ( 'NONE', #25745, .T. ) ;
#13583 = EDGE_CURVE ( 'NONE', #14377, #7094, #5600, .T. ) ;
#13584 = CARTESIAN_POINT ( 'NONE',  ( 32.54460952423471554, 0.2297037030477364072, 49.43553178847298568 ) ) ;
#13585 = EDGE_CURVE ( 'NONE', #15904, #22409, #5254, .T. ) ;
#13586 = AXIS2_PLACEMENT_3D ( 'NONE', #24358, #27869, #3313 ) ;
#13587 = CARTESIAN_POINT ( 'NONE',  ( 27.64943126350854286, -17.16721653852533791, 49.43553178847298568 ) ) ;
#13588 = ORIENTED_EDGE ( 'NONE', *, *, #13733, .F. ) ;
#13589 = CARTESIAN_POINT ( 'NONE',  ( -441.9999999999999432, -105.0000000000000142, -73.99999999999998579 ) ) ;
#13591 = CYLINDRICAL_SURFACE ( 'NONE', #24232, 3.999999999999976019 ) ;
#13590 = DIRECTION ( 'NONE',  ( -1.000000000000000000, -0.000000000000000000, -0.000000000000000000 ) ) ;
#13592 = ORIENTED_EDGE ( 'NONE', *, *, #28076, .F. ) ;
#13593 = CARTESIAN_POINT ( 'NONE',  ( 2.783107618865146016, -23.57982834652860049, 19.92325699910536940 ) ) ;
#13594 = PRODUCT_DEFINITION_SHAPE ( 'NONE', 'NONE',  #35193 ) ;
#13595 = ORIENTED_EDGE ( 'NONE', *, *, #13182, .F. ) ;
#13596 = CIRCLE ( 'NONE', #28389, 10.30000000000000071 ) ;
#13597 = VERTEX_POINT ( 'NONE', #29658 ) ;
#13598 = DIRECTION ( 'NONE',  ( 0.000000000000000000, -1.000000000000000000, -2.465190328815662439E-32 ) ) ;
#13599 = ORIENTED_EDGE ( 'NONE', *, *, #19261, .T. ) ;
#13600 = VERTEX_POINT ( 'NONE', #107 ) ;
#13601 = CARTESIAN_POINT ( 'NONE',  ( -418.0000000000000000, -105.0000000000000142, -101.9999999999999858 ) ) ;
#13602 = AXIS2_PLACEMENT_3D ( 'NONE', #24403, #16254, #22106 ) ;
#13603 = CARTESIAN_POINT ( 'NONE',  ( 11.99999999999999645, 144.9999999999999716, -186.9999999999999716 ) ) ;
#13604 = CARTESIAN_POINT ( 'NONE',  ( 2.790000000000082192, -27.65011189337340625, -13.25424764731434557 ) ) ;
#13605 = ORIENTED_EDGE ( 'NONE', *, *, #1015, .F. ) ;
#13606 = VERTEX_POINT ( 'NONE', #16146 ) ;
#13607 = DIRECTION ( 'NONE',  ( 0.000000000000000000, 1.836970198721029688E-16, -1.000000000000000000 ) ) ;
#13608 = LINE ( 'NONE', #2385, #4405 ) ;
#13609 = CARTESIAN_POINT ( 'NONE',  ( 109.6573908833661903, -3.356891575080633849, -12.04186941445821724 ) ) ;
#13610 = CARTESIAN_POINT ( 'NONE',  ( 2.783128948453668983, 7.365904273040312589, 29.97784191786588082 ) ) ;
#13611 = VERTEX_POINT ( 'NONE', #19336 ) ;
#13612 = CARTESIAN_POINT ( 'NONE',  ( 10.17231796313409298, 8.346743312457581609, -87.50000000000000000 ) ) ;
#13613 = CARTESIAN_POINT ( 'NONE',  ( 0.000000000000000000, 0.000000000000000000, 0.000000000000000000 ) ) ;
#13614 = EDGE_LOOP ( 'NONE', ( #29935, #33227, #27432, #16278 ) ) ;
#13615 = EDGE_CURVE ( 'NONE', #9940, #3430, #23953, .T. ) ;
#13616 = PLANE ( 'NONE',  #9955 ) ;
#13617 = DIRECTION ( 'NONE',  ( 1.000000000000000000, 0.000000000000000000, 0.000000000000000000 ) ) ;
#13618 = EDGE_CURVE ( 'NONE', #8598, #5515, #26987, .T. ) ;
#13619 = DIRECTION ( 'NONE',  ( 1.000000000000000000, -0.000000000000000000, 0.000000000000000000 ) ) ;
#13620 = VECTOR ( 'NONE', #29488, 1000.000000000000000 ) ;
#13621 = CARTESIAN_POINT ( 'NONE',  ( -12.00000000000001066, 124.9999999999999716, 155.0000000000000000 ) ) ;
#13622 = ORIENTED_EDGE ( 'NONE', *, *, #6086, .T. ) ;
#13623 = EDGE_CURVE ( 'NONE', #23058, #27275, #13071, .T. ) ;
#13624 = CARTESIAN_POINT ( 'NONE',  ( -418.0000000000000000, -137.0000000000000000, -175.0000000000000000 ) ) ;
#13625 = ORIENTED_EDGE ( 'NONE', *, *, #23297, .T. ) ;
#13626 = EDGE_CURVE ( 'NONE', #17170, #549, #843, .T. ) ;
#13627 = LINE ( 'NONE', #24286, #24795 ) ;
#13628 = FILL_AREA_STYLE ('',( #13288 ) ) ;
#13629 = VECTOR ( 'NONE', #19059, 1000.000000000000000 ) ;
#13630 = VERTEX_POINT ( 'NONE', #13814 ) ;
#13631 = FILL_AREA_STYLE ('',( #21291 ) ) ;
#13632 = FACE_OUTER_BOUND ( 'NONE', #13646, .T. ) ;
#13633 = ADVANCED_FACE ( 'NONE', ( #33862 ), #6966, .T. ) ;
#13634 = ORIENTED_EDGE ( 'NONE', *, *, #31016, .T. ) ;
#13635 = ORIENTED_EDGE ( 'NONE', *, *, #9437, .T. ) ;
#13636 = DIRECTION ( 'NONE',  ( -1.000000000000000000, 6.792721752314501023E-48, -3.697785493223492838E-32 ) ) ;
#13637 = LINE ( 'NONE', #21640, #23304 ) ;
#13638 = ORIENTED_EDGE ( 'NONE', *, *, #17021, .T. ) ;
#13639 = ORIENTED_EDGE ( 'NONE', *, *, #5961, .F. ) ;
#13640 = CARTESIAN_POINT ( 'NONE',  ( -499.9999999999999432, -137.0000000000000000, -159.0000000000000000 ) ) ;
#13641 = AXIS2_PLACEMENT_3D ( 'NONE', #23154, #31317, #28652 ) ;
#13642 = SURFACE_SIDE_STYLE ('',( #17960 ) ) ;
#13643 = CARTESIAN_POINT ( 'NONE',  ( 23.93847777447631131, 22.04889236939138542, 49.43553178847298568 ) ) ;
#13644 = CARTESIAN_POINT ( 'NONE',  ( -32.32899628990713126, -3.747048406849353697, 68.31122994652405112 ) ) ;
#13645 = ORIENTED_EDGE ( 'NONE', *, *, #19386, .F. ) ;
#13646 = EDGE_LOOP ( 'NONE', ( #22529, #195, #3986, #25537 ) ) ;
#13647 = DIRECTION ( 'NONE',  ( -1.000000000000000000, -0.000000000000000000, -0.000000000000000000 ) ) ;
#13648 = DIRECTION ( 'NONE',  ( -5.546364386991661285E-52, 0.000000000000000000, 1.000000000000000000 ) ) ;
#13649 = PLANE ( 'NONE',  #2687 ) ;
#13650 = DIRECTION ( 'NONE',  ( -1.000000000000000000, 0.000000000000000000, 0.000000000000000000 ) ) ;
#13651 = CARTESIAN_POINT ( 'NONE',  ( 50.00050000000000239, 0.000000000000000000, 10.00000000000000000 ) ) ;
#13652 = DIRECTION ( 'NONE',  ( -1.000000000000000000, 0.000000000000000000, 0.000000000000000000 ) ) ;
#13653 = CARTESIAN_POINT ( 'NONE',  ( 2.630124765083918348, -1.866624223957557893, -0.7500000000000000000 ) ) ;
#13654 = ORIENTED_EDGE ( 'NONE', *, *, #31961, .T. ) ;
#13655 = DIRECTION ( 'NONE',  ( 0.000000000000000000, 1.000000000000000000, 1.224646799147353207E-16 ) ) ;
#13656 = DIRECTION ( 'NONE',  ( -1.000000000000000000, 0.000000000000000000, 0.000000000000000000 ) ) ;
#13657 = CARTESIAN_POINT ( 'NONE',  ( -9.359714067160018747E-16, 0.6596962799436644209, -13.49999999999999822 ) ) ;
#13658 = ORIENTED_EDGE ( 'NONE', *, *, #17443, .T. ) ;
#13659 = CARTESIAN_POINT ( 'NONE',  ( -499.9999999999999432, -113.0000000000000000, -159.0000000000000000 ) ) ;
#13660 = ORIENTED_EDGE ( 'NONE', *, *, #937, .T. ) ;
#13661 = EDGE_CURVE ( 'NONE', #4938, #29908, #13995, .T. ) ;
#13662 = CARTESIAN_POINT ( 'NONE',  ( -109.9487023029381589, 1.336696757081942799, -12.43272095415539624 ) ) ;
#13663 = EDGE_CURVE ( 'NONE', #33397, #4380, #20171, .T. ) ;
#13664 = CYLINDRICAL_SURFACE ( 'NONE', #6475, 3.999999999999976019 ) ;
#13665 = AXIS2_PLACEMENT_3D ( 'NONE', #27949, #14797, #1427 ) ;
#13666 = VERTEX_POINT ( 'NONE', #28524 ) ;
#13667 = ADVANCED_FACE ( 'NONE', ( #20507 ), #34206, .F. ) ;
#13668 = ADVANCED_FACE ( 'NONE', ( #31360 ), #31532, .F. ) ;
#13669 = CARTESIAN_POINT ( 'NONE',  ( 1.394999999999999574, 14.89726405156260292, -31.02351007835962093 ) ) ;
#13670 = DIRECTION ( 'NONE',  ( 0.000000000000000000, 0.000000000000000000, 1.000000000000000000 ) ) ;
#13671 = DIRECTION ( 'NONE',  ( 0.9985334138511239299, -0.05413890858541752643, -0.000000000000000000 ) ) ;
#13672 = VERTEX_POINT ( 'NONE', #31021 ) ;
#13673 = ORIENTED_EDGE ( 'NONE', *, *, #22257, .F. ) ;
#13674 = CIRCLE ( 'NONE', #3506, 2.033421858999711507 ) ;
#13675 = DIRECTION ( 'NONE',  ( 2.631201909438060585E-14, -5.396010391056496978E-16, 1.000000000000000000 ) ) ;
#13676 = CARTESIAN_POINT ( 'NONE',  ( 0.000000000000000000, -7.666252171205713672, 29.49034198003804974 ) ) ;
#13677 = ORIENTED_EDGE ( 'NONE', *, *, #21203, .T. ) ;
#13678 = B_SPLINE_CURVE_WITH_KNOTS ( 'NONE', 3,
 ( #13713, #8369, #11227, #22078, #32919, #8540 ),
 .UNSPECIFIED., .F., .F.,
 ( 4, 2, 4 ),
 ( 4.404817011858791706E-07, 0.001874269613276467825, 0.003748098744851749778 ),
 .UNSPECIFIED. ) ;
#13679 = DIRECTION ( 'NONE',  ( -0.9635499925192230197, -0.2675283385292205329, 0.000000000000000000 ) ) ;
#13680 = EDGE_CURVE ( 'NONE', #14310, #3870, #22729, .T. ) ;
#13681 = CARTESIAN_POINT ( 'NONE',  ( 2.789999999999999147, 11.80989368511462523, 28.76039115933989976 ) ) ;
#13682 = CARTESIAN_POINT ( 'NONE',  ( 1.749999999999999778, 14.89726405156260469, -31.02351007835961383 ) ) ;
#13683 = CARTESIAN_POINT ( 'NONE',  ( -105.3468572192119694, -5.115148824049938092, 5.485002510375799112 ) ) ;
#13684 = EDGE_LOOP ( 'NONE', ( #12087, #14465, #17262, #1074 ) ) ;
#13685 = ORIENTED_EDGE ( 'NONE', *, *, #30624, .T. ) ;
#13686 = ORIENTED_EDGE ( 'NONE', *, *, #30619, .F. ) ;
#13687 = CIRCLE ( 'NONE', #2315, 7.999999999999979572 ) ;
#13688 = LINE ( 'NONE', #13352, #32231 ) ;
#13690 = AXIS2_PLACEMENT_3D ( 'NONE', #15448, #12783, #18482 ) ;
#13689 = LINE ( 'NONE', #24884, #34188 ) ;
#13691 = EDGE_CURVE ( 'NONE', #34601, #13338, #19320, .T. ) ;
#13692 = CYLINDRICAL_SURFACE ( 'NONE', #26951, 7.999999999999979572 ) ;
#13693 = ADVANCED_FACE ( 'NONE', ( #25848 ), #23187, .F. ) ;
#13694 = VERTEX_POINT ( 'NONE', #15180 ) ;
#13695 = ORIENTED_EDGE ( 'NONE', *, *, #15033, .F. ) ;
#13696 = DIRECTION ( 'NONE',  ( 1.000000000000000000, 3.469446951953834515E-18, 0.000000000000000000 ) ) ;
#13697 = ORIENTED_EDGE ( 'NONE', *, *, #8101, .F. ) ;
#13698 = CARTESIAN_POINT ( 'NONE',  ( 2.765921099433443331, 18.59128259035506758, -24.91982945642901726 ) ) ;
#13699 = CARTESIAN_POINT ( 'NONE',  ( -28.23027531293552528, -10.15143121711728469, 0.000000000000000000 ) ) ;
#13700 = VERTEX_POINT ( 'NONE', #14834 ) ;
#13701 = ORIENTED_EDGE ( 'NONE', *, *, #19414, .F. ) ;
#13702 = CARTESIAN_POINT ( 'NONE',  ( 15.99999999999998579, 75.55999999999990280, -177.7400000000000091 ) ) ;
#13703 = AXIS2_PLACEMENT_3D ( 'NONE', #13921, #16604, #11252 ) ;
#13705 = CARTESIAN_POINT ( 'NONE',  ( 21.24400529595486731, -24.65555945140049232, 49.43553178847298568 ) ) ;
#13704 = VECTOR ( 'NONE', #18118, 1000.000000000000000 ) ;
#13706 = ORIENTED_EDGE ( 'NONE', *, *, #1640, .F. ) ;
#13707 = DIRECTION ( 'NONE',  ( 0.000000000000000000, 0.000000000000000000, 1.000000000000000000 ) ) ;
#13708 = CYLINDRICAL_SURFACE ( 'NONE', #12051, 3.999999999999976019 ) ;
#13709 = CARTESIAN_POINT ( 'NONE',  ( 2.261199742870364293, -28.88016830755709563, 16.75753762755134701 ) ) ;
#13710 = CARTESIAN_POINT ( 'NONE',  ( 18.63894936814906345, 26.67946662374789213, 49.43553178847298568 ) ) ;
#13711 = EDGE_CURVE ( 'NONE', #8526, #23276, #29266, .T. ) ;
#13712 = EDGE_CURVE ( 'NONE', #4380, #24256, #30353, .T. ) ;
#13713 = CARTESIAN_POINT ( 'NONE',  ( 1.749999999999999778, -2.430610048905780030, -34.32897884578301984 ) ) ;
#13714 = CYLINDRICAL_SURFACE ( 'NONE', #3120, 2.000000000000001776 ) ;
#13715 = CIRCLE ( 'NONE', #2898, 1.154999999999999805 ) ;
#13716 = FILL_AREA_STYLE ('',( #24910 ) ) ;
#13717 = EDGE_CURVE ( 'NONE', #26511, #7371, #32379, .T. ) ;
#13718 = EDGE_LOOP ( 'NONE', ( #16530, #4915, #11291, #34500, #2268, #20208 ) ) ;
#13719 = DIRECTION ( 'NONE',  ( -1.000000000000000000, -0.000000000000000000, -0.000000000000000000 ) ) ;
#13720 = CARTESIAN_POINT ( 'NONE',  ( 787.0597240610709378, 1354.848721680646577, 1505.886119909295303 ) ) ;
#13721 = EDGE_LOOP ( 'NONE', ( #694, #27702, #25001, #28605 ) ) ;
#13722 = ORIENTED_EDGE ( 'NONE', *, *, #19861, .F. ) ;
#13723 = AXIS2_PLACEMENT_3D ( 'NONE', #8359, #16562, #22066 ) ;
#13724 = CARTESIAN_POINT ( 'NONE',  ( 106.3567858119077840, 5.578687132273540961, 5.013157219915588492 ) ) ;
#13725 = PRODUCT_CONTEXT ( 'NONE', #29182, 'mechanical' ) ;
#13726 = VECTOR ( 'NONE', #18889, 1000.000000000000000 ) ;
#13727 = ORIENTED_EDGE ( 'NONE', *, *, #3932, .F. ) ;
#13728 = AXIS2_PLACEMENT_3D ( 'NONE', #282, #30709, #805 ) ;
#13729 = AXIS2_PLACEMENT_3D ( 'NONE', #4447, #29204, #4797 ) ;
#13730 = CARTESIAN_POINT ( 'NONE',  ( -414.0000000000000568, 113.0000000000000000, 154.9999999999999716 ) ) ;
#13731 = ADVANCED_FACE ( 'NONE', ( #1293 ), #28691, .T. ) ;
#13732 = ITEM_DEFINED_TRANSFORMATION ( 'NONE', 'NONE', #4757,  #28566 ) ;
#13733 = EDGE_CURVE ( 'NONE', #13268, #2439, #23348, .T. ) ;
#13735 = LINE ( 'NONE', #29752, #30041 ) ;
#13734 = DIRECTION ( 'NONE',  ( 0.000000000000000000, 0.000000000000000000, -1.000000000000000000 ) ) ;
#13736 = ORIENTED_EDGE ( 'NONE', *, *, #2763, .F. ) ;
#13737 = ORIENTED_EDGE ( 'NONE', *, *, #15682, .T. ) ;
#13738 = FACE_OUTER_BOUND ( 'NONE', #25317, .T. ) ;
#13739 = CARTESIAN_POINT ( 'NONE',  ( 1.040000000000001368, -30.28730148581149706, -16.34215476954066304 ) ) ;
#13740 = EDGE_CURVE ( 'NONE', #34596, #292, #25669, .T. ) ;
#13741 = PLANE ( 'NONE',  #9939 ) ;
#13742 = CARTESIAN_POINT ( 'NONE',  ( 2.765921099433441110, -27.96208973699912548, 13.59246946040177129 ) ) ;
#13743 = CARTESIAN_POINT ( 'NONE',  ( -430.0000000000000000, 114.9999999999999574, 113.9999999999999858 ) ) ;
#13744 = ORIENTED_EDGE ( 'NONE', *, *, #4129, .F. ) ;
#13745 = AXIS2_PLACEMENT_3D ( 'NONE', #521, #166, #27384 ) ;
#13746 = FACE_OUTER_BOUND ( 'NONE', #15572, .T. ) ;
#13747 = CARTESIAN_POINT ( 'NONE',  ( -500.0000000000000000, -145.0000000000000000, 187.0000000000000000 ) ) ;
#13748 = CARTESIAN_POINT ( 'NONE',  ( 2.033589665237263144, -17.72288109958232383, 28.91649664306117629 ) ) ;
#13749 = ADVANCED_FACE ( 'NONE', ( #22175 ), #4117, .T. ) ;
#13750 =( REPRESENTATION_RELATIONSHIP ('NONE','NONE', #23037, #28231 ) REPRESENTATION_RELATIONSHIP_WITH_TRANSFORMATION ( #34659 )SHAPE_REPRESENTATION_RELATIONSHIP( ) );
#13751 = EDGE_CURVE ( 'NONE', #34323, #11236, #16858, .T. ) ;
#13752 = B_SPLINE_CURVE_WITH_KNOTS ( 'NONE', 3,
 ( #31008, #938, #8457, #9112, #13803, #30833 ),
 .UNSPECIFIED., .F., .F.,
 ( 4, 2, 4 ),
 ( 2.248981763129687575E-07, 0.001873423219693742293, 0.003746621541211171691 ),
 .UNSPECIFIED. ) ;
#13753 = CARTESIAN_POINT ( 'NONE',  ( -13.53398258527560749, -35.36769364574537633, -36.68877005347593467 ) ) ;
#13754 = SURFACE_STYLE_USAGE ( .BOTH. , #16438 ) ;
#13755 = CARTESIAN_POINT ( 'NONE',  ( -418.0000000000000000, -137.0000000000000000, 154.9999999999999716 ) ) ;
#13758 = CARTESIAN_POINT ( 'NONE',  ( 0.000000000000000000, 49.99999999999999289, 0.000000000000000000 ) ) ;
#13757 = DIRECTION ( 'NONE',  ( -1.300283923313630633E-47, 0.000000000000000000, -1.000000000000000000 ) ) ;
#13756 = AXIS2_PLACEMENT_3D ( 'NONE', #26139, #28118, #34151 ) ;
#13759 = VECTOR ( 'NONE', #6690, 1000.000000000000000 ) ;
#13760 = AXIS2_PLACEMENT_3D ( 'NONE', #4715, #18124, #4020 ) ;
#13761 = CARTESIAN_POINT ( 'NONE',  ( 1.040000000000000702, -10.37741591188916779, 32.81304455236864470 ) ) ;
#13763 = ORIENTED_EDGE ( 'NONE', *, *, #23923, .F. ) ;
#13762 = AXIS2_PLACEMENT_3D ( 'NONE', #15821, #23809, #1739 ) ;
#13765 = AXIS2_PLACEMENT_3D ( 'NONE', #32915, #24543, #22074 ) ;
#13764 = DIRECTION ( 'NONE',  ( -1.000000000000000000, 0.000000000000000000, -5.546364386991661285E-52 ) ) ;
#13767 = FACE_BOUND ( 'NONE', #28107, .T. ) ;
#13766 = FACE_OUTER_BOUND ( 'NONE', #1353, .T. ) ;
#13768 = VERTEX_POINT ( 'NONE', #4818 ) ;
#13769 = DIRECTION ( 'NONE',  ( 1.000000000000000000, 0.000000000000000000, 0.000000000000000000 ) ) ;
#13770 = VERTEX_POINT ( 'NONE', #34735 ) ;
#13771 = VERTEX_POINT ( 'NONE', #26718 ) ;
#13772 = DIRECTION ( 'NONE',  ( 0.000000000000000000, 1.000000000000000000, 1.836970198721029688E-16 ) ) ;
#13773 = ORIENTED_EDGE ( 'NONE', *, *, #26319, .T. ) ;
#13774 = ORIENTED_EDGE ( 'NONE', *, *, #21049, .T. ) ;
#13775 = DIRECTION ( 'NONE',  ( -0.6051742151937650194, -0.7960930657056438653, 0.000000000000000000 ) ) ;
#13776 = EDGE_CURVE ( 'NONE', #32621, #25011, #17093, .T. ) ;
#13778 = CIRCLE ( 'NONE', #26268, 3.999999999999976019 ) ;
#13777 = ITEM_DEFINED_TRANSFORMATION ( 'NONE', 'NONE', #32583,  #28566 ) ;
#13779 = EDGE_CURVE ( 'NONE', #16592, #30042, #15949, .T. ) ;
#13780 = DIRECTION ( 'NONE',  ( 0.000000000000000000, 1.310824597558155437E-49, 1.000000000000000000 ) ) ;
#13781 = AXIS2_PLACEMENT_3D ( 'NONE', #26963, #5582, #19318 ) ;
#13782 = PLANE ( 'NONE',  #27321 ) ;
#13783 = ORIENTED_EDGE ( 'NONE', *, *, #34069, .T. ) ;
#13784 = VERTEX_POINT ( 'NONE', #12683 ) ;
#13785 = CIRCLE ( 'NONE', #13207, 2.085824230283342740 ) ;
#13786 = DIRECTION ( 'NONE',  ( 0.000000000000000000, 1.131431318426415506E-52, 1.000000000000000000 ) ) ;
#13787 = DIRECTION ( 'NONE',  ( 1.000000000000000000, 0.000000000000000000, 0.000000000000000000 ) ) ;
#13788 = DIRECTION ( 'NONE',  ( -0.000000000000000000, -0.000000000000000000, -1.000000000000000000 ) ) ;
#13789 = CARTESIAN_POINT ( 'NONE',  ( -12.00000000000001066, 134.9999999999999432, -186.9999999999999716 ) ) ;
#13790 = VERTEX_POINT ( 'NONE', #10716 ) ;
#13791 = CARTESIAN_POINT ( 'NONE',  ( -12.00000000000001066, 104.9999999999999858, -175.0000000000000284 ) ) ;
#13792 = DIRECTION ( 'NONE',  ( 0.000000000000000000, 0.000000000000000000, -1.000000000000000000 ) ) ;
#13793 = ORIENTED_EDGE ( 'NONE', *, *, #2471, .F. ) ;
#13794 = FACE_OUTER_BOUND ( 'NONE', #19136, .T. ) ;
#13795 = CARTESIAN_POINT ( 'NONE',  ( -45.00000000000000000, 16.36947364650383818, 36.69637551990492597 ) ) ;
#13796 = CARTESIAN_POINT ( 'NONE',  ( 13.32059394339353986, -35.43959265050632013, -36.68877005347593467 ) ) ;
#13797 = CARTESIAN_POINT ( 'NONE',  ( -143.0000000000000568, -173.5121282296299796, -41.09364177412887642 ) ) ;
#13798 = ORIENTED_EDGE ( 'NONE', *, *, #14644, .T. ) ;
#13799 = DIRECTION ( 'NONE',  ( -3.040835319149746090E-31, -1.000000000000000000, 0.000000000000000000 ) ) ;
#13800 = ORIENTED_EDGE ( 'NONE', *, *, #924, .F. ) ;
#13802 = FILL_AREA_STYLE_COLOUR ( '', #21402 ) ;
#13801 = CARTESIAN_POINT ( 'NONE',  ( -442.0000000000000000, 105.0000000000000142, -105.9999999999999574 ) ) ;
#13803 = CARTESIAN_POINT ( 'NONE',  ( 0.7561992172567417736, -24.35691930005274131, 23.60041548268705114 ) ) ;
#13804 = AXIS2_PLACEMENT_3D ( 'NONE', #32234, #18896, #5514 ) ;
#13806 = ORIENTED_EDGE ( 'NONE', *, *, #23258, .F. ) ;
#13805 = AXIS2_PLACEMENT_3D ( 'NONE', #19407, #13887, #29907 ) ;
#13807 = AXIS2_PLACEMENT_3D ( 'NONE', #24420, #18593, #10383 ) ;
#13808 = CARTESIAN_POINT ( 'NONE',  ( 1.040000000000000924, 0.000000000000000000, 0.000000000000000000 ) ) ;
#13809 = PLANE ( 'NONE',  #16593 ) ;
#13810 = ORIENTED_EDGE ( 'NONE', *, *, #6815, .F. ) ;
#13811 = ORIENTED_EDGE ( 'NONE', *, *, #19213, .F. ) ;
#13812 = VERTEX_POINT ( 'NONE', #15710 ) ;
#13813 = CARTESIAN_POINT ( 'NONE',  ( 19.99999999999998224, 144.9999999999999147, 162.9999999999999716 ) ) ;
#13814 = CARTESIAN_POINT ( 'NONE',  ( -418.0000000000000000, 109.0000000000000142, 154.9999999999999716 ) ) ;
#13815 = EDGE_LOOP ( 'NONE', ( #15043, #16771, #7709, #16763 ) ) ;
#13816 = ORIENTED_EDGE ( 'NONE', *, *, #1292, .T. ) ;
#13817 = DIRECTION ( 'NONE',  ( 0.000000000000000000, 0.000000000000000000, 1.000000000000000000 ) ) ;
#13818 = EDGE_CURVE ( 'NONE', #9992, #23016, #29221, .T. ) ;
#13819 = DIRECTION ( 'NONE',  ( 0.000000000000000000, 1.000000000000000000, 0.000000000000000000 ) ) ;
#13820 = EDGE_CURVE ( 'NONE', #22622, #8018, #4542, .T. ) ;
#13821 = AXIS2_PLACEMENT_3D ( 'NONE', #5020, #4658, #23374 ) ;
#13822 = CARTESIAN_POINT ( 'NONE',  ( -119.9999999999997726, 1.224646799147353256E-15, -10.00000000000000000 ) ) ;
#13823 = FACE_OUTER_BOUND ( 'NONE', #15394, .T. ) ;
#13824 = ORIENTED_EDGE ( 'NONE', *, *, #4157, .T. ) ;
#13825 = ORIENTED_EDGE ( 'NONE', *, *, #2533, .F. ) ;
#13826 = LINE ( 'NONE', #826, #4271 ) ;
#13827 = FACE_OUTER_BOUND ( 'NONE', #3984, .T. ) ;
#13828 = ADVANCED_FACE ( 'NONE', ( #1984 ), #7310, .T. ) ;
#13829 = CARTESIAN_POINT ( 'NONE',  ( 187.4264068711928530, -12.50000000000001066, 1.224646799147353217E-14 ) ) ;
#13830 = CARTESIAN_POINT ( 'NONE',  ( -442.0000000000000000, -104.9999999999999858, -159.0000000000000000 ) ) ;
#13831 = AXIS2_PLACEMENT_3D ( 'NONE', #19377, #11363, #30051 ) ;
#13832 = CARTESIAN_POINT ( 'NONE',  ( 8.000000000000000000, 0.000000000000000000, 0.000000000000000000 ) ) ;
#13833 = CIRCLE ( 'NONE', #22926, 7.999999999999979572 ) ;
#13834 = DIRECTION ( 'NONE',  ( 0.000000000000000000, 0.7071067811865489050, 0.7071067811865462405 ) ) ;
#13835 = AXIS2_PLACEMENT_3D ( 'NONE', #22817, #6242, #17144 ) ;
#13836 = DIRECTION ( 'NONE',  ( -0.000000000000000000, -1.836970198721029688E-16, 1.000000000000000000 ) ) ;
#13837 = ORIENTED_EDGE ( 'NONE', *, *, #7817, .T. ) ;
#13838 = CARTESIAN_POINT ( 'NONE',  ( 0.000000000000000000, -33.69708579775584667, 49.43553178847298568 ) ) ;
#13839 = LINE ( 'NONE', #312, #17181 ) ;
#13840 = FACE_OUTER_BOUND ( 'NONE', #2117, .T. ) ;
#13841 = ORIENTED_EDGE ( 'NONE', *, *, #8840, .F. ) ;
#13842 = DIRECTION ( 'NONE',  ( -0.000000000000000000, 0.000000000000000000, 1.000000000000000000 ) ) ;
#13843 = ORIENTED_EDGE ( 'NONE', *, *, #5915, .F. ) ;
#13844 = CARTESIAN_POINT ( 'NONE',  ( 0.000000000000000000, -33.69708579775584667, 49.43553178847298568 ) ) ;
#13845 = CARTESIAN_POINT ( 'NONE',  ( -100.9384238677276358, 3.126956236148901169, -12.10589691785417976 ) ) ;
#13846 = CIRCLE ( 'NONE', #16708, 34.41491905851385269 ) ;
#13847 = ORIENTED_EDGE ( 'NONE', *, *, #25788, .F. ) ;
#13848 = CARTESIAN_POINT ( 'NONE',  ( -499.9999999999999432, 144.9999999999999716, -162.9999999999999716 ) ) ;
#13849 = LINE ( 'NONE', #21676, #31555 ) ;
#13850 = DIRECTION ( 'NONE',  ( 0.000000000000000000, 1.224646799147359124E-16, 1.000000000000000000 ) ) ;
#13851 = ORIENTED_EDGE ( 'NONE', *, *, #5189, .F. ) ;
#13852 = AXIS2_PLACEMENT_3D ( 'NONE', #17955, #20261, #20431 ) ;
#13853 = ORIENTED_EDGE ( 'NONE', *, *, #3591, .F. ) ;
#13854 = VECTOR ( 'NONE', #3285, 1000.000000000000000 ) ;
#13855 = DIRECTION ( 'NONE',  ( 2.631201909438060585E-14, -5.396010391056496978E-16, 1.000000000000000000 ) ) ;
#13856 = AXIS2_PLACEMENT_3D ( 'NONE', #8537, #30252, #5852 ) ;
#13857 = DIRECTION ( 'NONE',  ( 0.000000000000000000, 0.000000000000000000, 1.000000000000000000 ) ) ;
#13858 = EDGE_LOOP ( 'NONE', ( #3121, #11337, #33960, #29738 ) ) ;
#13859 = CARTESIAN_POINT ( 'NONE',  ( -418.0000000000000000, 137.0000000000000000, -155.0000000000000000 ) ) ;
#13860 = ADVANCED_FACE ( 'NONE', ( #15523 ), #31702, .F. ) ;
#13861 = CYLINDRICAL_SURFACE ( 'NONE', #11855, 3.999999999999976019 ) ;
#13862 = LINE ( 'NONE', #24701, #16774 ) ;
#13863 = CARTESIAN_POINT ( 'NONE',  ( -109.8381179908438554, -1.694081942180569733, 7.313267332261218279 ) ) ;
#13864 = ORIENTED_EDGE ( 'NONE', *, *, #442, .T. ) ;
#13865 = ORIENTED_EDGE ( 'NONE', *, *, #6971, .F. ) ;
#13866 = VERTEX_POINT ( 'NONE', #29032 ) ;
#13867 = EDGE_CURVE ( 'NONE', #29138, #5785, #18787, .T. ) ;
#13868 = CARTESIAN_POINT ( 'NONE',  ( 20.62763069236413926, -31.74750072459299588, 68.31122994652405112 ) ) ;
#13869 = EDGE_CURVE ( 'NONE', #890, #1214, #17, .T. ) ;
#13870 = CARTESIAN_POINT ( 'NONE',  ( 2.783107618352422374, 18.40335333576878440, 24.78429060331947298 ) ) ;
#13871 = AXIS2_PLACEMENT_3D ( 'NONE', #24303, #13467, #26989 ) ;
#13872 = CARTESIAN_POINT ( 'NONE',  ( 1.749999999999999778, -24.90160365674886478, 23.75493189058330756 ) ) ;
#13873 = ORIENTED_EDGE ( 'NONE', *, *, #33298, .T. ) ;
#13874 = ORIENTED_EDGE ( 'NONE', *, *, #9780, .T. ) ;
#13875 = EDGE_CURVE ( 'NONE', #19820, #30104, #5112, .T. ) ;
#13876 = ADVANCED_FACE ( 'NONE', ( #4633 ), #2274, .T. ) ;
#13877 = DIRECTION ( 'NONE',  ( -1.000000000000000000, -0.000000000000000000, -0.000000000000000000 ) ) ;
#13878 = ORIENTED_EDGE ( 'NONE', *, *, #435, .T. ) ;
#13879 = PLANE ( 'NONE',  #22087 ) ;
#13880 = EDGE_CURVE ( 'NONE', #32148, #21072, #29573, .T. ) ;
#13881 = CARTESIAN_POINT ( 'NONE',  ( 3.235562306570555532E-30, 1.325223266901699007E-14, -67.50000000000000000 ) ) ;
#13882 = ORIENTED_EDGE ( 'NONE', *, *, #7538, .T. ) ;
#13883 = CYLINDRICAL_SURFACE ( 'NONE', #27584, 3.999999999999976019 ) ;
#13884 = ORIENTED_EDGE ( 'NONE', *, *, #31693, .T. ) ;
#13885 = CARTESIAN_POINT ( 'NONE',  ( 1.999999999999999556, 0.000000000000000000, 0.000000000000000000 ) ) ;
#13886 = CIRCLE ( 'NONE', #33773, 3.999999999999976019 ) ;
#13887 = DIRECTION ( 'NONE',  ( 1.000000000000000000, 0.000000000000000000, 0.000000000000000000 ) ) ;
#13888 = VERTEX_POINT ( 'NONE', #9997 ) ;
#13889 = DIRECTION ( 'NONE',  ( -1.000000000000000000, 0.000000000000000000, -0.000000000000000000 ) ) ;
#13891 = CIRCLE ( 'NONE', #8766, 2.033421858999711951 ) ;
#13890 = CARTESIAN_POINT ( 'NONE',  ( -12.00000000000001066, 144.9999999999999147, 187.0000000000000000 ) ) ;
#13892 = FACE_OUTER_BOUND ( 'NONE', #27711, .T. ) ;
#13893 = DIRECTION ( 'NONE',  ( 1.000000000000000000, 0.000000000000000000, 0.000000000000000000 ) ) ;
#13894 = FACE_OUTER_BOUND ( 'NONE', #20257, .T. ) ;
#13895 = DIRECTION ( 'NONE',  ( -1.000000000000000000, 0.000000000000000000, 0.000000000000000000 ) ) ;
#13896 = CIRCLE ( 'NONE', #6486, 4.750000000000004441 ) ;
#13897 = VERTEX_POINT ( 'NONE', #15354 ) ;
#13898 = LINE ( 'NONE', #21724, #22779 ) ;
#13899 = DIRECTION ( 'NONE',  ( 0.1063910735368947813, -0.9943243633099144718, -3.335902418024520312E-15 ) ) ;
#13900 = ORIENTED_EDGE ( 'NONE', *, *, #20470, .T. ) ;
#13901 = AXIS2_PLACEMENT_3D ( 'NONE', #18097, #2045, #18255 ) ;
#13902 = ORIENTED_EDGE ( 'NONE', *, *, #22751, .F. ) ;
#13903 = ORIENTED_EDGE ( 'NONE', *, *, #20204, .F. ) ;
#13904 = VECTOR ( 'NONE', #4492, 1000.000000000000000 ) ;
#13905 = CARTESIAN_POINT ( 'NONE',  ( 105.3927003681590548, 5.728044018051756225, 4.841538128164400767 ) ) ;
#13906 = PRODUCT_CONTEXT ( 'NONE', #18084, 'mechanical' ) ;
#13907 = AXIS2_PLACEMENT_3D ( 'NONE', #3772, #22479, #19982 ) ;
#13908 = ORIENTED_EDGE ( 'NONE', *, *, #5114, .T. ) ;
#13909 = CARTESIAN_POINT ( 'NONE',  ( 2.789999999999999147, -25.83993731729781729, -18.77381338200996552 ) ) ;
#13910 =( LENGTH_UNIT ( ) NAMED_UNIT ( * ) SI_UNIT ( .MILLI., .METRE. ) );
#13911 = CONICAL_SURFACE ( 'NONE', #11660, 13.50000000000000000, 1.047197551196600296 ) ;
#13913 = CARTESIAN_POINT ( 'NONE',  ( 2.719051662517718793, -18.14830959286877388, -25.98365187356541028 ) ) ;
#13912 = LINE ( 'NONE', #27602, #28102 ) ;
#13914 = ORIENTED_EDGE ( 'NONE', *, *, #14840, .T. ) ;
#13915 = ORIENTED_EDGE ( 'NONE', *, *, #21663, .T. ) ;
#13916 = EDGE_CURVE ( 'NONE', #12316, #3925, #2529, .T. ) ;
#13917 = EDGE_CURVE ( 'NONE', #17462, #7759, #27774, .T. ) ;
#13918 = FACE_OUTER_BOUND ( 'NONE', #21485, .T. ) ;
#13919 = DIRECTION ( 'NONE',  ( 0.000000000000000000, 0.000000000000000000, 1.000000000000000000 ) ) ;
#13920 = DIRECTION ( 'NONE',  ( -0.000000000000000000, -1.836970198721029688E-16, 1.000000000000000000 ) ) ;
#13921 = CARTESIAN_POINT ( 'NONE',  ( 0.000000000000000000, 6.992329373473909019E-15, 49.43553178847298568 ) ) ;
#13922 = DIRECTION ( 'NONE',  ( 0.000000000000000000, 0.5877852522924797984, -0.8090169943749424553 ) ) ;
#13923 = EDGE_LOOP ( 'NONE', ( #8424, #28536 ) ) ;
#13924 = CARTESIAN_POINT ( 'NONE',  ( -20.63749999999999929, 1.224646799147352862E-15, 9.999999999999996447 ) ) ;
#13925 = CARTESIAN_POINT ( 'NONE',  ( 2.630124765083918348, -1.866624223957557893, 5.429999999999999716 ) ) ;
#13926 = VECTOR ( 'NONE', #16282, 1000.000000000000000 ) ;
#13927 = DIRECTION ( 'NONE',  ( 1.000000000000000000, 0.000000000000000000, 0.000000000000000000 ) ) ;
#13928 = B_SPLINE_CURVE_WITH_KNOTS ( 'NONE', 3,
 ( #28988, #9609, #31482, #15481 ),
 .UNSPECIFIED., .F., .F.,
 ( 4, 4 ),
 ( 2.080333525986984783E-07, 0.0006879438135628625824 ),
 .UNSPECIFIED. ) ;
#13929 = VECTOR ( 'NONE', #33606, 1000.000000000000000 ) ;
#13930 = CYLINDRICAL_SURFACE ( 'NONE', #31127, 16.19999999999999574 ) ;
#13931 = LINE ( 'NONE', #19453, #25072 ) ;
#13932 = EDGE_CURVE ( 'NONE', #15331, #15311, #1720, .T. ) ;
#13933 = PRODUCT_DEFINITION_SHAPE ( 'NONE', 'NONE',  #35196 ) ;
#13934 = DIRECTION ( 'NONE',  ( 0.000000000000000000, 0.000000000000000000, -1.000000000000000000 ) ) ;
#13936 = CARTESIAN_POINT ( 'NONE',  ( -5.527271473480783293, -1.747512292859696226, 4.679999999999999716 ) ) ;
#13935 = CARTESIAN_POINT ( 'NONE',  ( -349.0000000000000000, 134.9999999999999716, 109.9999999999999858 ) ) ;
#13937 = CIRCLE ( 'NONE', #12804, 2.000000000000001776 ) ;
#13938 = AXIS2_PLACEMENT_3D ( 'NONE', #12632, #31822, #12290 ) ;
#13939 = DIRECTION ( 'NONE',  ( -0.000000000000000000, -1.000000000000000000, -0.000000000000000000 ) ) ;
#13940 = VERTEX_POINT ( 'NONE', #8551 ) ;
#13941 = DIRECTION ( 'NONE',  ( 0.000000000000000000, 5.053935297177146739E-49, 1.000000000000000000 ) ) ;
#13943 = DIRECTION ( 'NONE',  ( 1.000000000000000000, 0.000000000000000000, -0.000000000000000000 ) ) ;
#13942 = DIRECTION ( 'NONE',  ( 0.000000000000000000, -1.000000000000000000, 6.123233995736766036E-17 ) ) ;
#13944 = AXIS2_PLACEMENT_3D ( 'NONE', #25882, #28894, #17713 ) ;
#13945 = EDGE_CURVE ( 'NONE', #2043, #19944, #19259, .T. ) ;
#13946 = ADVANCED_FACE ( 'NONE', ( #30097 ), #27422, .T. ) ;
#13947 = EDGE_CURVE ( 'NONE', #26182, #13268, #8727, .T. ) ;
#13948 = ORIENTED_EDGE ( 'NONE', *, *, #11262, .T. ) ;
#13949 = EDGE_CURVE ( 'NONE', #1876, #20519, #30268, .T. ) ;
#13950 = ORIENTED_EDGE ( 'NONE', *, *, #25340, .T. ) ;
#13951 = VECTOR ( 'NONE', #30100, 1000.000000000000000 ) ;
#13952 = B_SPLINE_CURVE_WITH_KNOTS ( 'NONE', 3,
 ( #27220, #32210, #10688, #7823 ),
 .UNSPECIFIED., .F., .F.,
 ( 4, 4 ),
 ( 2.013258991796058355E-07, 0.0006879370499044200164 ),
 .UNSPECIFIED. ) ;
#13953 = AXIS2_PLACEMENT_3D ( 'NONE', #4009, #17933, #28759 ) ;
#13954 = EDGE_LOOP ( 'NONE', ( #27650, #15530, #8095, #10601 ) ) ;
#13955 = PLANE ( 'NONE',  #16749 ) ;
#13956 = ORIENTED_EDGE ( 'NONE', *, *, #21511, .F. ) ;
#13957 = EDGE_LOOP ( 'NONE', ( #31535, #7893, #3902, #2695 ) ) ;
#13958 = DIRECTION ( 'NONE',  ( 0.000000000000000000, -1.000000000000000000, -5.145227585319922065E-49 ) ) ;
#13959 = VECTOR ( 'NONE', #27525, 1000.000000000000000 ) ;
#13960 = ORIENTED_EDGE ( 'NONE', *, *, #24814, .F. ) ;
#13961 = DIRECTION ( 'NONE',  ( -1.000000000000000000, -0.000000000000000000, -0.000000000000000000 ) ) ;
#13962 = CARTESIAN_POINT ( 'NONE',  ( -449.9999999999999432, -105.0000000000000142, 162.9999999999999716 ) ) ;
#13963 = ORIENTED_EDGE ( 'NONE', *, *, #20266, .F. ) ;
#13964 = VERTEX_POINT ( 'NONE', #3212 ) ;
#13965 = EDGE_CURVE ( 'NONE', #19763, #5382, #29746, .T. ) ;
#13966 = VECTOR ( 'NONE', #9730, 1000.000000000000000 ) ;
#13967 = CARTESIAN_POINT ( 'NONE',  ( 8.000000000000000000, 1.738998454789241155E-15, 14.19999999999999929 ) ) ;
#13968 = CARTESIAN_POINT ( 'NONE',  ( 8.927936315454015670, -31.29690601358702651, 49.43553178847298568 ) ) ;
#13969 = CIRCLE ( 'NONE', #2035, 32.54542015209055705 ) ;
#13970 = CARTESIAN_POINT ( 'NONE',  ( -45.00000000000000000, -46.95407462254104303, 36.69637551990492597 ) ) ;
#13971 = DIRECTION ( 'NONE',  ( 1.000000000000000000, 0.000000000000000000, 0.000000000000000000 ) ) ;
#13972 = EDGE_LOOP ( 'NONE', ( #33305, #21280, #32342, #31166 ) ) ;
#13973 = LINE ( 'NONE', #3273, #13985 ) ;
#13974 = CARTESIAN_POINT ( 'NONE',  ( -365.0000000000000000, 130.9999999999999716, 126.0000000000000000 ) ) ;
#13975 = ORIENTED_EDGE ( 'NONE', *, *, #19990, .T. ) ;
#13976 = LINE ( 'NONE', #8268, #21978 ) ;
#13977 = CARTESIAN_POINT ( 'NONE',  ( 143.0000000000000568, -12.50000000000001066, 1.224646799147353217E-14 ) ) ;
#13978 = CARTESIAN_POINT ( 'NONE',  ( -414.0000000000000568, -105.0000000000000142, 187.0000000000000000 ) ) ;
#13979 = CARTESIAN_POINT ( 'NONE',  ( 2.719010670248903416, 7.308614668456580254, -30.84037831947987485 ) ) ;
#13980 = ORIENTED_EDGE ( 'NONE', *, *, #7050, .T. ) ;
#13981 = DIRECTION ( 'NONE',  ( 0.000000000000000000, 0.000000000000000000, -1.000000000000000000 ) ) ;
#13982 = EDGE_LOOP ( 'NONE', ( #27604, #5120, #15903, #31644 ) ) ;
#13984 = LINE ( 'NONE', #13454, #31091 ) ;
#13983 = DIRECTION ( 'NONE',  ( 0.000000000000000000, 0.000000000000000000, -1.000000000000000000 ) ) ;
#13985 = VECTOR ( 'NONE', #16835, 1000.000000000000000 ) ;
#13986 = EDGE_CURVE ( 'NONE', #18999, #6917, #3385, .T. ) ;
#13987 = EDGE_CURVE ( 'NONE', #34921, #6854, #26716, .T. ) ;
#13988 = EDGE_LOOP ( 'NONE', ( #9653, #8159, #21922, #20482 ) ) ;
#13989 = CARTESIAN_POINT ( 'NONE',  ( -35.00000000000000000, 42.49491490430484220, 36.69637551990492597 ) ) ;
#13990 = DIRECTION ( 'NONE',  ( 1.000000000000000000, 0.000000000000000000, 0.000000000000000000 ) ) ;
#13991 = VECTOR ( 'NONE', #7834, 1000.000000000000000 ) ;
#13992 = ORIENTED_EDGE ( 'NONE', *, *, #11112, .F. ) ;
#13993 = ORIENTED_EDGE ( 'NONE', *, *, #7009, .F. ) ;
#13994 = DIRECTION ( 'NONE',  ( 0.000000000000000000, 1.131431318426415506E-52, 1.000000000000000000 ) ) ;
#13995 = LINE ( 'NONE', #23013, #34655 ) ;
#13996 = ORIENTED_EDGE ( 'NONE', *, *, #31149, .F. ) ;
#13997 = ORIENTED_EDGE ( 'NONE', *, *, #6734, .F. ) ;
#13998 = FACE_OUTER_BOUND ( 'NONE', #31244, .T. ) ;
#13999 = DIRECTION ( 'NONE',  ( -1.000000000000000000, 0.000000000000000000, 0.000000000000000000 ) ) ;
#14000 = VECTOR ( 'NONE', #16113, 1000.000000000000000 ) ;
#14001 = LINE ( 'NONE', #19699, #31110 ) ;
#14002 = CARTESIAN_POINT ( 'NONE',  ( 23.31255882915078814, -22.70966696615089830, 68.31122994652405112 ) ) ;
#14003 = ORIENTED_EDGE ( 'NONE', *, *, #3359, .F. ) ;
#14004 = ORIENTED_EDGE ( 'NONE', *, *, #11781, .T. ) ;
#14005 = CARTESIAN_POINT ( 'NONE',  ( 0.000000000000000000, -33.69708579775584667, -36.68877005347592757 ) ) ;
#14006 = CARTESIAN_POINT ( 'NONE',  ( -6.500000000000000000, 0.000000000000000000, 3.931000000000000494 ) ) ;
#14007 = CARTESIAN_POINT ( 'NONE',  ( 2.789999999999999147, 0.000000000000000000, 0.000000000000000000 ) ) ;
#14008 = VECTOR ( 'NONE', #16969, 1000.000000000000000 ) ;
#14009 = CARTESIAN_POINT ( 'NONE',  ( 55.00000000000000711, 0.000000000000000000, 0.000000000000000000 ) ) ;
#14010 = CARTESIAN_POINT ( 'NONE',  ( -10.00000000000000000, 0.000000000000000000, 0.000000000000000000 ) ) ;
#14012 = LINE ( 'NONE', #19187, #5510 ) ;
#14011 =( REPRESENTATION_RELATIONSHIP ('NONE','NONE', #23037, #28231 ) REPRESENTATION_RELATIONSHIP_WITH_TRANSFORMATION ( #14270 )SHAPE_REPRESENTATION_RELATIONSHIP( ) );
#14013 = CARTESIAN_POINT ( 'NONE',  ( 0.000000000000000000, 3.524919873834583163E-15, 68.31122994652405112 ) ) ;
#14014 = ORIENTED_EDGE ( 'NONE', *, *, #22595, .F. ) ;
#14015 = EDGE_CURVE ( 'NONE', #33660, #9411, #16505, .T. ) ;
#14016 = AXIS2_PLACEMENT_3D ( 'NONE', #34244, #31398, #9856 ) ;
#14017 = DIRECTION ( 'NONE',  ( -0.000000000000000000, -1.000000000000000000, -0.000000000000000000 ) ) ;
#14018 = CARTESIAN_POINT ( 'NONE',  ( 0.07098925588714952162, -15.78394019282763239, 27.48475859319551873 ) ) ;
#14019 = LINE ( 'NONE', #27706, #33106 ) ;
#14020 = VERTEX_POINT ( 'NONE', #15139 ) ;
#14021 = DIRECTION ( 'NONE',  ( -0.000000000000000000, -0.000000000000000000, 1.000000000000000000 ) ) ;
#14022 = ORIENTED_EDGE ( 'NONE', *, *, #27763, .F. ) ;
#14023 = CARTESIAN_POINT ( 'NONE',  ( -500.0000000000000000, -137.0000000000000000, 194.9999999999999716 ) ) ;
#14024 = CARTESIAN_POINT ( 'NONE',  ( -12.00000000000001066, -109.0000000000000142, 174.9999999999999432 ) ) ;
#14025 = ADVANCED_FACE ( 'NONE', ( #3560 ), #33822, .T. ) ;
#14026 = EDGE_CURVE ( 'NONE', #4606, #20760, #22968, .T. ) ;
#14027 = CIRCLE ( 'NONE', #6026, 7.999999999999979572 ) ;
#14028 = EDGE_CURVE ( 'NONE', #29720, #20094, #25978, .T. ) ;
#14029 = EDGE_LOOP ( 'NONE', ( #33090, #3962, #10533, #16475 ) ) ;
#14030 = LINE ( 'NONE', #3683, #26806 ) ;
#14031 = LINE ( 'NONE', #24867, #2558 ) ;
#14033 = EDGE_CURVE ( 'NONE', #27516, #4507, #25451, .T. ) ;
#14032 = DIRECTION ( 'NONE',  ( 1.000000000000000000, 0.000000000000000000, 0.000000000000000000 ) ) ;
#14034 = VERTEX_POINT ( 'NONE', #12472 ) ;
#14035 = DIRECTION ( 'NONE',  ( 0.1063910735369155841, -0.9943243633099125844, -3.335902418025060287E-15 ) ) ;
#14036 = DIRECTION ( 'NONE',  ( 1.000000000000000000, 0.000000000000000000, 0.000000000000000000 ) ) ;
#14037 = VERTEX_POINT ( 'NONE', #3742 ) ;
#14038 = AXIS2_PLACEMENT_3D ( 'NONE', #13417, #5549, #24250 ) ;
#14039 = CARTESIAN_POINT ( 'NONE',  ( 0.1859802735910837668, -8.821517218319813836, -31.05303142369434966 ) ) ;
#14040 = SURFACE_SIDE_STYLE ('',( #339 ) ) ;
#14041 = DIRECTION ( 'NONE',  ( 1.000000000000000000, 0.000000000000000000, 0.000000000000000000 ) ) ;
#14042 = CARTESIAN_POINT ( 'NONE',  ( -100.8614468863726756, -3.010446655309094499, 6.870869395578496963 ) ) ;
#14043 = ORIENTED_EDGE ( 'NONE', *, *, #16583, .T. ) ;
#14044 = VERTEX_POINT ( 'NONE', #1602 ) ;
#14045 = VERTEX_POINT ( 'NONE', #20128 ) ;
#14046 = PRODUCT ( 'motor shaft', 'motor shaft', '', ( #5868 ) ) ;
#14047 = FILL_AREA_STYLE ('',( #3351 ) ) ;
#14048 = AXIS2_PLACEMENT_3D ( 'NONE', #24982, #32468, #24449 ) ;
#14049 = DIRECTION ( 'NONE',  ( 0.9289767198167914186, -0.3701381553399144542, 0.000000000000000000 ) ) ;
#14050 = CIRCLE ( 'NONE', #27098, 4.750000000000004441 ) ;
#14051 = VECTOR ( 'NONE', #519, 1000.000000000000000 ) ;
#14052 = CARTESIAN_POINT ( 'NONE',  ( -449.9999999999999432, -137.0000000000000000, -155.0000000000000000 ) ) ;
#14053 = ORIENTED_EDGE ( 'NONE', *, *, #28775, .T. ) ;
#14054 = ORIENTED_EDGE ( 'NONE', *, *, #8263, .F. ) ;
#14055 = CARTESIAN_POINT ( 'NONE',  ( -418.0000000000000000, -112.9999999999999858, -155.0000000000000000 ) ) ;
#14056 = ORIENTED_EDGE ( 'NONE', *, *, #27771, .T. ) ;
#14057 = B_SPLINE_CURVE_WITH_KNOTS ( 'NONE', 3,
 ( #7505, #10018, #9839, #28541 ),
 .UNSPECIFIED., .F., .F.,
 ( 4, 4 ),
 ( 2.557638148638405956E-07, 0.0006879919438241684443 ),
 .UNSPECIFIED. ) ;
#14058 = DIRECTION ( 'NONE',  ( 0.000000000000000000, 0.000000000000000000, 1.000000000000000000 ) ) ;
#14059 = DIRECTION ( 'NONE',  ( -0.000000000000000000, -0.000000000000000000, -1.000000000000000000 ) ) ;
#14060 = ORIENTED_EDGE ( 'NONE', *, *, #8464, .F. ) ;
#14061 = ORIENTED_EDGE ( 'NONE', *, *, #31180, .F. ) ;
#14062 = DIRECTION ( 'NONE',  ( 0.000000000000000000, 1.000000000000000000, 0.000000000000000000 ) ) ;
#14063 = EDGE_CURVE ( 'NONE', #15632, #23681, #9451, .T. ) ;
#14064 = CARTESIAN_POINT ( 'NONE',  ( 2.789999999999999147, 28.95078156989571383, -9.502838467757751317 ) ) ;
#14065 = VERTEX_POINT ( 'NONE', #22793 ) ;
#14066 = DIRECTION ( 'NONE',  ( 0.000000000000000000, 1.836970198721029441E-16, -1.000000000000000000 ) ) ;
#14067 = FACE_OUTER_BOUND ( 'NONE', #9102, .T. ) ;
#14068 = EDGE_CURVE ( 'NONE', #7373, #9180, #11947, .T. ) ;
#14069 = DIRECTION ( 'NONE',  ( -0.7621620551276356847, -0.6473862847818285804, -1.189229312204944401E-16 ) ) ;
#14070 = DIRECTION ( 'NONE',  ( 1.000000000000000000, -0.000000000000000000, -0.000000000000000000 ) ) ;
#14071 = AXIS2_PLACEMENT_3D ( 'NONE', #10966, #21813, #11324 ) ;
#14072 = CARTESIAN_POINT ( 'NONE',  ( 0.006871061397808507845, -17.88422427744469090, 25.16112242373430874 ) ) ;
#14073 = PLANE ( 'NONE',  #1981 ) ;
#14075 = EDGE_CURVE ( 'NONE', #26932, #32711, #31159, .T. ) ;
#14074 = DIRECTION ( 'NONE',  ( -1.000000000000000000, 0.000000000000000000, 0.000000000000000000 ) ) ;
#14076 = VECTOR ( 'NONE', #20365, 1000.000000000000000 ) ;
#14077 = VECTOR ( 'NONE', #17141, 1000.000000000000000 ) ;
#14078 = VERTEX_POINT ( 'NONE', #9618 ) ;
#14079 = ADVANCED_FACE ( 'NONE', ( #30801 ), #8909, .T. ) ;
#14080 = CARTESIAN_POINT ( 'NONE',  ( 830.5212630532004141, 1222.560835574797693, 1753.598338701303419 ) ) ;
#14081 = EDGE_LOOP ( 'NONE', ( #21722, #12266, #6978, #5058 ) ) ;
#14082 = VERTEX_POINT ( 'NONE', #19781 ) ;
#14083 = EDGE_CURVE ( 'NONE', #22788, #30647, #12530, .T. ) ;
#14084 = EDGE_CURVE ( 'NONE', #501, #10781, #17817, .T. ) ;
#14085 = AXIS2_PLACEMENT_3D ( 'NONE', #32682, #2428, #2606 ) ;
#14086 = CARTESIAN_POINT ( 'NONE',  ( -70.00000000000000000, 4.559999999999909015, -168.2400000000000091 ) ) ;
#14087 = CARTESIAN_POINT ( 'NONE',  ( 19.99999999999998224, 134.9999999999998863, 162.9999999999999716 ) ) ;
#14088 = SHAPE_DEFINITION_REPRESENTATION ( #17203, #1195 ) ;
#14089 = EDGE_LOOP ( 'NONE', ( #29037, #13950, #1424, #6901, #3520, #22634, #627, #34893, #17127, #5067, #9999, #73, #30364, #22297, #15248, #15888 ) ) ;
#14090 = CARTESIAN_POINT ( 'NONE',  ( -1.030735741678193484, 1.713938105891546826, -0.7500000000000000000 ) ) ;
#14091 = SURFACE_STYLE_USAGE ( .BOTH. , #15899 ) ;
#14092 = ITEM_DEFINED_TRANSFORMATION ( 'NONE', 'NONE', #5874,  #28566 ) ;
#14094 = CARTESIAN_POINT ( 'NONE',  ( -25.07182831876307105, -28.36910952062232738, -36.68877005347593467 ) ) ;
#14093 = LINE ( 'NONE', #6406, #8195 ) ;
#14095 = AXIS2_PLACEMENT_3D ( 'NONE', #23021, #3785, #1475 ) ;
#14096 = ORIENTED_EDGE ( 'NONE', *, *, #21898, .F. ) ;
#14097 = VERTEX_POINT ( 'NONE', #12127 ) ;
#14098 = DIRECTION ( 'NONE',  ( -0.000000000000000000, 1.836970198721029688E-16, -1.000000000000000000 ) ) ;
#14099 = CARTESIAN_POINT ( 'NONE',  ( 0.5288002393074070495, 13.51471344666089003, 30.53246971302650081 ) ) ;
#14100 = FACE_OUTER_BOUND ( 'NONE', #21791, .T. ) ;
#14101 = DIRECTION ( 'NONE',  ( 1.000000000000000000, 0.000000000000000000, 0.000000000000000000 ) ) ;
#14102 = VERTEX_POINT ( 'NONE', #28313 ) ;
#14104 = DIRECTION ( 'NONE',  ( 0.000000000000000000, 0.000000000000000000, -1.000000000000000000 ) ) ;
#14103 = AXIS2_PLACEMENT_3D ( 'NONE', #149, #29700, #7801 ) ;
#14106 = PLANE ( 'NONE',  #28783 ) ;
#14105 = AXIS2_PLACEMENT_3D ( 'NONE', #32914, #19409, #30249 ) ;
#14107 = DIRECTION ( 'NONE',  ( 0.000000000000000000, 1.374038396813312784E-15, -1.000000000000000000 ) ) ;
#14108 = ORIENTED_EDGE ( 'NONE', *, *, #30449, .T. ) ;
#14109 = LINE ( 'NONE', #19108, #30539 ) ;
#14110 = CYLINDRICAL_SURFACE ( 'NONE', #17159, 4.000000000000003553 ) ;
#14111 = DIRECTION ( 'NONE',  ( 0.9476531711828030113, 0.3193015301359780622, -0.000000000000000000 ) ) ;
#14112 = AXIS2_PLACEMENT_3D ( 'NONE', #20009, #9134, #255 ) ;
#14114 = CARTESIAN_POINT ( 'NONE',  ( 0.2222207399958900931, 3.306033584716338236, 13.49999999999999645 ) ) ;
#14113 = DIRECTION ( 'NONE',  ( 0.000000000000000000, -0.000000000000000000, -1.000000000000000000 ) ) ;
#14115 = CARTESIAN_POINT ( 'NONE',  ( -12.00000000000001066, -124.9999999999999432, -158.9999999999999716 ) ) ;
#14116 = ORIENTED_EDGE ( 'NONE', *, *, #22646, .F. ) ;
#14117 = DIRECTION ( 'NONE',  ( 1.000000000000000000, 0.000000000000000000, 0.000000000000000000 ) ) ;
#14118 =( NAMED_UNIT ( * ) PLANE_ANGLE_UNIT ( ) SI_UNIT ( $, .RADIAN. ) );
#14119 = ADVANCED_FACE ( 'NONE', ( #3905 ), #22627, .T. ) ;
#14120 = VECTOR ( 'NONE', #19092, 1000.000000000000000 ) ;
#14121 = ORIENTED_EDGE ( 'NONE', *, *, #9161, .T. ) ;
#14122 = ADVANCED_FACE ( 'NONE', ( #28481 ), #33465, .T. ) ;
#14123 = EDGE_CURVE ( 'NONE', #28125, #30633, #27860, .T. ) ;
#14124 = EDGE_LOOP ( 'NONE', ( #12917, #15797, #4530, #17035 ) ) ;
#14125 = AXIS2_PLACEMENT_3D ( 'NONE', #15669, #2119, #25802 ) ;
#14126 = CIRCLE ( 'NONE', #26061, 30.47050528711511674 ) ;
#14127 = ORIENTED_EDGE ( 'NONE', *, *, #12636, .T. ) ;
#14128 = LINE ( 'NONE', #25318, #17338 ) ;
#14129 = EDGE_LOOP ( 'NONE', ( #9475, #18130, #20241, #10515, #16118, #33243, #10421, #13115 ) ) ;
#14130 = ORIENTED_EDGE ( 'NONE', *, *, #576, .T. ) ;
#14131 = CARTESIAN_POINT ( 'NONE',  ( -19.99999999999998934, 144.9999999999999147, 187.0000000000000000 ) ) ;
#14132 = ADVANCED_FACE ( 'NONE', ( #4256 ), #6252, .T. ) ;
#14133 = AXIS2_PLACEMENT_3D ( 'NONE', #28365, #13569, #15539 ) ;
#14134 = ITEM_DEFINED_TRANSFORMATION ( 'NONE', 'NONE', #12140,  #28566 ) ;
#14135 = EDGE_LOOP ( 'NONE', ( #9793, #9224, #32055, #16010, #4932, #29903 ) ) ;
#14136 = DIRECTION ( 'NONE',  ( 0.000000000000000000, 0.000000000000000000, -1.000000000000000000 ) ) ;
#14137 = DIRECTION ( 'NONE',  ( 0.000000000000000000, 1.000000000000000000, 0.000000000000000000 ) ) ;
#14138 = ORIENTED_EDGE ( 'NONE', *, *, #1938, .T. ) ;
#14139 = EDGE_LOOP ( 'NONE', ( #25207, #20221, #6511, #12589 ) ) ;
#14140 = DIRECTION ( 'NONE',  ( -1.848892746611746419E-32, -6.842277657836020854E-49, 1.000000000000000000 ) ) ;
#14141 = CARTESIAN_POINT ( 'NONE',  ( 1.749999999999999778, -1.891117961019737725, -34.36292081097834483 ) ) ;
#14142 = EDGE_CURVE ( 'NONE', #19207, #1031, #28131, .T. ) ;
#14143 = CARTESIAN_POINT ( 'NONE',  ( 110.5494250287361808, -1.507735446164279125, -12.41434713890700969 ) ) ;
#14144 = CIRCLE ( 'NONE', #20396, 4.000000000000003553 ) ;
#14145 = LINE ( 'NONE', #12772, #17682 ) ;
#14146 = FACE_OUTER_BOUND ( 'NONE', #30566, .T. ) ;
#14147 = ORIENTED_EDGE ( 'NONE', *, *, #1199, .F. ) ;
#14148 = EDGE_CURVE ( 'NONE', #11540, #13159, #1286, .T. ) ;
#14149 = DIRECTION ( 'NONE',  ( -0.000000000000000000, -1.000000000000000000, -0.000000000000000000 ) ) ;
#14150 = VECTOR ( 'NONE', #31369, 1000.000000000000000 ) ;
#14151 = ADVANCED_FACE ( 'NONE', ( #10307, #34884, #18172 ), #26148, .F. ) ;
#14152 = CARTESIAN_POINT ( 'NONE',  ( -70.00000000000000000, 75.55999999999990280, 177.7400000000000091 ) ) ;
#14153 = VERTEX_POINT ( 'NONE', #28824 ) ;
#14154 = CARTESIAN_POINT ( 'NONE',  ( -35.00000000000000000, -46.95407462254104303, 36.69637551990492597 ) ) ;
#14155 = CARTESIAN_POINT ( 'NONE',  ( 0.000000000000000000, -55.00000000000000711, 155.0000000000000000 ) ) ;
#14156 = DIRECTION ( 'NONE',  ( 1.232595164407830946E-32, 3.421138828918010427E-49, -1.000000000000000000 ) ) ;
#14157 = DIRECTION ( 'NONE',  ( -1.000000000000000000, 0.000000000000000000, 0.000000000000000000 ) ) ;
#14158 = FACE_OUTER_BOUND ( 'NONE', #4034, .T. ) ;
#14159 = AXIS2_PLACEMENT_3D ( 'NONE', #33595, #27902, #19561 ) ;
#14160 = DIRECTION ( 'NONE',  ( -0.000000000000000000, 1.000000000000000000, 0.000000000000000000 ) ) ;
#14161 = ORIENTED_EDGE ( 'NONE', *, *, #30668, .T. ) ;
#14162 = B_SPLINE_CURVE_WITH_KNOTS ( 'NONE', 3,
 ( #12515, #4302, #33872, #7498, #31370, #20354 ),
 .UNSPECIFIED., .F., .F.,
 ( 4, 2, 4 ),
 ( 4.404817046682342164E-07, 0.001874269636018126642, 0.003748098790331584954 ),
 .UNSPECIFIED. ) ;
#14164 = CARTESIAN_POINT ( 'NONE',  ( 2.265105744522721398, -28.86920449294081337, -16.75648442687151629 ) ) ;
#14163 = CARTESIAN_POINT ( 'NONE',  ( 5.021133111224162171, -21.54630831098063837, -67.50000000000000000 ) ) ;
#14165 = VECTOR ( 'NONE', #27701, 1000.000000000000000 ) ;
#14166 = EDGE_LOOP ( 'NONE', ( #10385, #13722, #28171, #16844 ) ) ;
#14167 = EDGE_CURVE ( 'NONE', #28571, #18201, #12996, .T. ) ;
#14168 = ADVANCED_FACE ( 'NONE', ( #7098 ), #13167, .T. ) ;
#14169 = DIRECTION ( 'NONE',  ( 0.9941379571543593752, -0.1081190184239433083, -0.000000000000000000 ) ) ;
#14170 = DIRECTION ( 'NONE',  ( -0.000000000000000000, 1.000000000000000000, -0.000000000000000000 ) ) ;
#14171 = ORIENTED_EDGE ( 'NONE', *, *, #11789, .F. ) ;
#14172 = ADVANCED_FACE ( 'NONE', ( #29179 ), #31819, .T. ) ;
#14173 = ORIENTED_EDGE ( 'NONE', *, *, #21552, .F. ) ;
#14174 = AXIS2_PLACEMENT_3D ( 'NONE', #29187, #26510, #4781 ) ;
#14175 = EDGE_LOOP ( 'NONE', ( #23403, #13635, #4138, #6759 ) ) ;
#14176 = CARTESIAN_POINT ( 'NONE',  ( 145.0000000000000568, -97.49999999999998579, 51.88904920397793319 ) ) ;
#14177 = CARTESIAN_POINT ( 'NONE',  ( 2.630124765083918348, -1.866624223957557893, 5.429999999999999716 ) ) ;
#14178 = EDGE_LOOP ( 'NONE', ( #3944, #14462, #5765, #15182 ) ) ;
#14179 = ORIENTED_EDGE ( 'NONE', *, *, #1064, .T. ) ;
#14180 = LINE ( 'NONE', #22355, #3062 ) ;
#14181 = LINE ( 'NONE', #8644, #6762 ) ;
#14182 = VECTOR ( 'NONE', #17038, 1000.000000000000000 ) ;
#14183 = DIRECTION ( 'NONE',  ( -0.000000000000000000, 1.836970198721029688E-16, -1.000000000000000000 ) ) ;
#14184 = CARTESIAN_POINT ( 'NONE',  ( -20.00000000000007461, 108.9999999999999858, 187.0000000000000000 ) ) ;
#14185 = EDGE_LOOP ( 'NONE', ( #4311, #21070, #8093, #3665 ) ) ;
#14186 = ORIENTED_EDGE ( 'NONE', *, *, #4130, .T. ) ;
#14187 = LINE ( 'NONE', #9182, #16245 ) ;
#14188 = LINE ( 'NONE', #25014, #33403 ) ;
#14189 = FACE_OUTER_BOUND ( 'NONE', #19126, .T. ) ;
#14190 = CARTESIAN_POINT ( 'NONE',  ( -5.210000000000000853, 0.000000000000000000, 0.000000000000000000 ) ) ;
#14191 = LINE ( 'NONE', #35026, #6916 ) ;
#14192 = AXIS2_PLACEMENT_3D ( 'NONE', #13613, #19145, #29985 ) ;
#14193 = EDGE_CURVE ( 'NONE', #11373, #8598, #23837, .T. ) ;
#14194 = EDGE_CURVE ( 'NONE', #3925, #12316, #2896, .T. ) ;
#14195 = LINE ( 'NONE', #30193, #11111 ) ;
#14196 = CARTESIAN_POINT ( 'NONE',  ( -19.99999999999998934, 75.55999999999990280, -172.9900000000000091 ) ) ;
#14197 = CARTESIAN_POINT ( 'NONE',  ( -12.00000000000001066, 124.9999999999999716, 155.0000000000000000 ) ) ;
#14198 = ORIENTED_EDGE ( 'NONE', *, *, #6848, .T. ) ;
#14199 = DIRECTION ( 'NONE',  ( 0.000000000000000000, 0.000000000000000000, 1.000000000000000000 ) ) ;
#14200 = EDGE_CURVE ( 'NONE', #549, #17170, #9285, .T. ) ;
#14201 = CARTESIAN_POINT ( 'NONE',  ( 28.23027531293552528, -10.15143121711728469, 20.00000000000000000 ) ) ;
#14202 = DIRECTION ( 'NONE',  ( -1.000000000000000000, 0.000000000000000000, 0.000000000000000000 ) ) ;
#14203 = ORIENTED_EDGE ( 'NONE', *, *, #8142, .F. ) ;
#14204 = CIRCLE ( 'NONE', #26099, 32.54542015209055705 ) ;
#14205 = EDGE_CURVE ( 'NONE', #20230, #22483, #24517, .T. ) ;
#14206 = DIRECTION ( 'NONE',  ( -0.000000000000000000, 0.000000000000000000, 1.000000000000000000 ) ) ;
#14207 = ORIENTED_EDGE ( 'NONE', *, *, #9555, .T. ) ;
#14208 = CARTESIAN_POINT ( 'NONE',  ( -499.9999999999999432, 108.9999999999999858, -162.9999999999999716 ) ) ;
#14209 = CARTESIAN_POINT ( 'NONE',  ( 0.000000000000000000, 0.000000000000000000, 5.429999999999999716 ) ) ;
#14210 = VERTEX_POINT ( 'NONE', #13515 ) ;
#14211 = DIRECTION ( 'NONE',  ( -0.000000000000000000, -1.000000000000000000, -0.000000000000000000 ) ) ;
#14212 = LINE ( 'NONE', #3507, #7691 ) ;
#14213 = DIRECTION ( 'NONE',  ( 0.000000000000000000, -5.145227585319922065E-49, -1.000000000000000000 ) ) ;
#14214 = ORIENTED_EDGE ( 'NONE', *, *, #12944, .F. ) ;
#14215 = CIRCLE ( 'NONE', #15352, 1.999999999999999112 ) ;
#14216 = CARTESIAN_POINT ( 'NONE',  ( 835.3620542627927534, 1177.319101683247709, 1753.598338701303646 ) ) ;
#14217 = CARTESIAN_POINT ( 'NONE',  ( -449.9999999999999432, -104.9999999999999858, -187.0000000000000000 ) ) ;
#14218 = EDGE_CURVE ( 'NONE', #9057, #34809, #8686, .T. ) ;
#14219 = ORIENTED_EDGE ( 'NONE', *, *, #11715, .T. ) ;
#14220 = CARTESIAN_POINT ( 'NONE',  ( 0.07094832863588811100, -8.452579892119532090, -30.54611582031341754 ) ) ;
#14221 = PLANE ( 'NONE',  #26638 ) ;
#14222 = CARTESIAN_POINT ( 'NONE',  ( -410.0000000000000568, 105.0000000000000000, -77.99999999999997158 ) ) ;
#14223 = CARTESIAN_POINT ( 'NONE',  ( 2.783107606170884818, 28.06690468450167586, 12.85275635055316457 ) ) ;
#14224 = CONTEXT_DEPENDENT_SHAPE_REPRESENTATION ( #5099, #4048 ) ;
#14225 = VERTEX_POINT ( 'NONE', #16546 ) ;
#14227 = ORIENTED_EDGE ( 'NONE', *, *, #11704, .T. ) ;
#14226 =( REPRESENTATION_RELATIONSHIP ('NONE','NONE', #23037, #15767 ) REPRESENTATION_RELATIONSHIP_WITH_TRANSFORMATION ( #33425 )SHAPE_REPRESENTATION_RELATIONSHIP( ) );
#14228 = ORIENTED_EDGE ( 'NONE', *, *, #22145, .F. ) ;
#14229 = B_SPLINE_CURVE_WITH_KNOTS ( 'NONE', 3,
 ( #7858, #5877, #391, #2515, #13913, #27603 ),
 .UNSPECIFIED., .F., .F.,
 ( 4, 2, 4 ),
 ( 4.404817033506925723E-07, 0.001874269626248501212, 0.003748098770793652050 ),
 .UNSPECIFIED. ) ;
#14230 =( LENGTH_UNIT ( ) NAMED_UNIT ( * ) SI_UNIT ( .MILLI., .METRE. ) );
#14231 = EDGE_CURVE ( 'NONE', #12281, #29036, #28016, .T. ) ;
#14232 = DIRECTION ( 'NONE',  ( 0.000000000000000000, 0.000000000000000000, 1.000000000000000000 ) ) ;
#14233 = ADVANCED_FACE ( 'NONE', ( #2990 ), #12085, .T. ) ;
#14234 = B_SPLINE_CURVE_WITH_KNOTS ( 'NONE', 3,
 ( #13050, #8213, #3399, #13742 ),
 .UNSPECIFIED., .F., .F.,
 ( 4, 4 ),
 ( 0.005298345749243301393, 0.005985214453301814473 ),
 .UNSPECIFIED. ) ;
#14235 = EDGE_CURVE ( 'NONE', #33527, #5237, #3518, .T. ) ;
#14236 = CARTESIAN_POINT ( 'NONE',  ( 2.789999999999999147, -23.41952779159748133, -19.49300927180569687 ) ) ;
#14237 = EDGE_LOOP ( 'NONE', ( #2401, #25362, #9354, #7923 ) ) ;
#14238 = ORIENTED_EDGE ( 'NONE', *, *, #7420, .F. ) ;
#14239 = CARTESIAN_POINT ( 'NONE',  ( 1.749999999999999778, -30.28730148581173864, 16.34215476954022606 ) ) ;
#14240 = ORIENTED_EDGE ( 'NONE', *, *, #22834, .F. ) ;
#14241 = DIRECTION ( 'NONE',  ( 1.000000000000000000, 0.000000000000000000, -1.232595164407831220E-32 ) ) ;
#14242 = LINE ( 'NONE', #11566, #29086 ) ;
#14243 = ORIENTED_EDGE ( 'NONE', *, *, #32694, .T. ) ;
#14244 = AXIS2_PLACEMENT_3D ( 'NONE', #12862, #28863, #21206 ) ;
#14245 = ORIENTED_EDGE ( 'NONE', *, *, #17849, .T. ) ;
#14246 = CARTESIAN_POINT ( 'NONE',  ( 15.99999999999998579, 75.55999999999990280, 172.9900000000000091 ) ) ;
#14247 = CARTESIAN_POINT ( 'NONE',  ( 129.3530333899765594, -6.000000000000000000, 57.49999999999999289 ) ) ;
#14248 = ORIENTED_EDGE ( 'NONE', *, *, #13222, .T. ) ;
#14249 = DIRECTION ( 'NONE',  ( 0.000000000000000000, 0.000000000000000000, 1.000000000000000000 ) ) ;
#14250 = DIRECTION ( 'NONE',  ( -1.000000000000000000, -0.000000000000000000, -0.000000000000000000 ) ) ;
#14251 = CARTESIAN_POINT ( 'NONE',  ( -499.9999999999999432, 112.9999999999999574, -155.0000000000000000 ) ) ;
#14252 = CARTESIAN_POINT ( 'NONE',  ( -499.9999999999999432, 140.9999999999999716, 162.9999999999999716 ) ) ;
#14253 = CARTESIAN_POINT ( 'NONE',  ( 8.000000000000000000, 0.000000000000000000, 0.000000000000000000 ) ) ;
#14254 = CARTESIAN_POINT ( 'NONE',  ( -12.00000000000001066, -124.9999999999999432, -154.9999999999999716 ) ) ;
#14255 = VERTEX_POINT ( 'NONE', #30756 ) ;
#14256 = EDGE_LOOP ( 'NONE', ( #8070, #18243, #17523, #5806, #5910, #11991, #20319, #10579 ) ) ;
#14257 = DIRECTION ( 'NONE',  ( 2.631201909438060269E-14, -5.396010391056495992E-16, 0.9999999999999998890 ) ) ;
#14258 = VECTOR ( 'NONE', #10458, 1000.000000000000114 ) ;
#14259 = ORIENTED_EDGE ( 'NONE', *, *, #7247, .F. ) ;
#14260 = ORIENTED_EDGE ( 'NONE', *, *, #18902, .T. ) ;
#14261 = CIRCLE ( 'NONE', #26177, 15.00000000000000000 ) ;
#14262 = FACE_OUTER_BOUND ( 'NONE', #16003, .T. ) ;
#14263 = CARTESIAN_POINT ( 'NONE',  ( 102.4121716945766565, 5.134660333356495521, 5.470525374126623319 ) ) ;
#14264 = APPLICATION_PROTOCOL_DEFINITION ( 'draft international standard', 'automotive_design', 1998, #4841 ) ;
#14265 = ADVANCED_FACE ( 'NONE', ( #866 ), #17259, .T. ) ;
#14266 = VERTEX_POINT ( 'NONE', #23113 ) ;
#14267 = LINE ( 'NONE', #24752, #9952 ) ;
#14268 = CARTESIAN_POINT ( 'NONE',  ( -99.88497961182919482, 6.264410040187948829E-16, -12.50000000000000000 ) ) ;
#14269 = ADVANCED_FACE ( 'NONE', ( #28267 ), #12262, .T. ) ;
#14270 = ITEM_DEFINED_TRANSFORMATION ( 'NONE', 'NONE', #1924,  #28566 ) ;
#14271 = EDGE_CURVE ( 'NONE', #701, #1613, #12267, .T. ) ;
#14273 = FACE_OUTER_BOUND ( 'NONE', #9522, .T. ) ;
#14272 = CARTESIAN_POINT ( 'NONE',  ( -34.04247984038124031, 16.56841925338182619, -36.68877005347593467 ) ) ;
#14275 = ORIENTED_EDGE ( 'NONE', *, *, #23740, .F. ) ;
#14274 = AXIS2_PLACEMENT_3D ( 'NONE', #6458, #33522, #33881 ) ;
#14276 = VERTEX_POINT ( 'NONE', #6181 ) ;
#14277 = LINE ( 'NONE', #2864, #3210 ) ;
#14278 = VECTOR ( 'NONE', #2235, 1000.000000000000000 ) ;
#14279 = EDGE_CURVE ( 'NONE', #5820, #35091, #17076, .T. ) ;
#14280 = DIRECTION ( 'NONE',  ( 0.000000000000000000, 0.000000000000000000, 1.000000000000000000 ) ) ;
#14281 = CARTESIAN_POINT ( 'NONE',  ( 0.2989565185775198697, 0.000000000000000000, 0.000000000000000000 ) ) ;
#14282 = PLANE ( 'NONE',  #11594 ) ;
#14283 = VERTEX_POINT ( 'NONE', #11730 ) ;
#14284 = PLANE ( 'NONE',  #29999 ) ;
#14285 = CARTESIAN_POINT ( 'NONE',  ( 11.99999999999999645, 134.9999999999999432, -194.9999999999999432 ) ) ;
#14286 = FACE_OUTER_BOUND ( 'NONE', #7732, .T. ) ;
#14287 = B_SPLINE_CURVE_WITH_KNOTS ( 'NONE', 3,
 ( #22558, #9023, #19891, #30732, #6858, #1185 ),
 .UNSPECIFIED., .F., .F.,
 ( 4, 2, 4 ),
 ( 1.989389909935507169E-07, 0.001873397232195059573, 0.003746595525399125815 ),
 .UNSPECIFIED. ) ;
#14288 = ORIENTED_EDGE ( 'NONE', *, *, #6009, .T. ) ;
#14289 = VECTOR ( 'NONE', #24272, 1000.000000000000000 ) ;
#14290 = LINE ( 'NONE', #21751, #3260 ) ;
#14291 = CYLINDRICAL_SURFACE ( 'NONE', #85, 2.085824230283342740 ) ;
#14292 = EDGE_CURVE ( 'NONE', #19981, #6277, #20091, .T. ) ;
#14293 = DIRECTION ( 'NONE',  ( 0.000000000000000000, 1.836970198721029441E-16, -1.000000000000000000 ) ) ;
#14295 = LINE ( 'NONE', #33666, #9990 ) ;
#14294 = FACE_OUTER_BOUND ( 'NONE', #33235, .T. ) ;
#14296 = UNCERTAINTY_MEASURE_WITH_UNIT (LENGTH_MEASURE( 1.000000000000000082E-05 ), #32654, 'distance_accuracy_value', 'NONE');
#14297 = CARTESIAN_POINT ( 'NONE',  ( -418.0000000000000000, -124.9999999999999858, -69.99999999999998579 ) ) ;
#14298 = ORIENTED_EDGE ( 'NONE', *, *, #33045, .F. ) ;
#14299 = LINE ( 'NONE', #9296, #16770 ) ;
#14300 = CARTESIAN_POINT ( 'NONE',  ( -145.0000000000000568, -78.33668825982579165, -75.00000000000001421 ) ) ;
#14301 = ORIENTED_EDGE ( 'NONE', *, *, #26914, .F. ) ;
#14302 = AXIS2_PLACEMENT_3D ( 'NONE', #18539, #13363, #23847 ) ;
#14303 =( NAMED_UNIT ( * ) SI_UNIT ( $, .STERADIAN. ) SOLID_ANGLE_UNIT ( ) );
#14304 = CIRCLE ( 'NONE', #33618, 5.115020388170798959 ) ;
#14305 = VECTOR ( 'NONE', #1675, 1000.000000000000000 ) ;
#14306 = VECTOR ( 'NONE', #26002, 1000.000000000000000 ) ;
#14307 = ORIENTED_EDGE ( 'NONE', *, *, #9405, .F. ) ;
#14308 = VERTEX_POINT ( 'NONE', #11909 ) ;
#14309 = LINE ( 'NONE', #12645, #25817 ) ;
#14310 = VERTEX_POINT ( 'NONE', #33597 ) ;
#14311 = ORIENTED_EDGE ( 'NONE', *, *, #32890, .T. ) ;
#14312 = FACE_OUTER_BOUND ( 'NONE', #590, .T. ) ;
#14313 = ADVANCED_FACE ( 'NONE', ( #17775 ), #19951, .T. ) ;
#14314 = CIRCLE ( 'NONE', #17166, 7.999999999999979572 ) ;
#14315 = CONTEXT_DEPENDENT_SHAPE_REPRESENTATION ( #29914, #24373 ) ;
#14316 = ORIENTED_EDGE ( 'NONE', *, *, #34113, .T. ) ;
#14317 = DIRECTION ( 'NONE',  ( -0.4684084406997904848, 0.8835120444460226041, -0.000000000000000000 ) ) ;
#14318 = CARTESIAN_POINT ( 'NONE',  ( 5.021133111224576062, 18.16264470403145026, -67.50000000000000000 ) ) ;
#14319 = ORIENTED_EDGE ( 'NONE', *, *, #16950, .F. ) ;
#14320 = ORIENTED_EDGE ( 'NONE', *, *, #20259, .F. ) ;
#14321 = LINE ( 'NONE', #30142, #23649 ) ;
#14322 = DIRECTION ( 'NONE',  ( 0.000000000000000000, 0.000000000000000000, -1.000000000000000000 ) ) ;
#14323 = ADVANCED_FACE ( 'NONE', ( #31283 ), #27904, .T. ) ;
#14324 = ADVANCED_FACE ( 'NONE', ( #4033 ), #30936, .F. ) ;
#14325 = CARTESIAN_POINT ( 'NONE',  ( 108.7902275512028751, -4.324042002361276005, -11.73155476838175204 ) ) ;
#14326 = DIRECTION ( 'NONE',  ( 1.000000000000000000, 0.000000000000000000, 0.000000000000000000 ) ) ;
#14327 = LINE ( 'NONE', #27655, #27345 ) ;
#14328 = ORIENTED_EDGE ( 'NONE', *, *, #2430, .F. ) ;
#14329 = VECTOR ( 'NONE', #14825, 1000.000000000000000 ) ;
#14330 = CARTESIAN_POINT ( 'NONE',  ( 0.000000000000000000, 14.59907093257252164, -26.74544485249453274 ) ) ;
#14331 = VECTOR ( 'NONE', #17054, 1000.000000000000000 ) ;
#14332 = EDGE_CURVE ( 'NONE', #7246, #11377, #28455, .T. ) ;
#14333 = EDGE_CURVE ( 'NONE', #15331, #6935, #3866, .T. ) ;
#14334 = DIRECTION ( 'NONE',  ( -0.9766205557100864354, 0.2149704402110247659, -0.000000000000000000 ) ) ;
#14335 = ORIENTED_EDGE ( 'NONE', *, *, #2326, .F. ) ;
#14336 = AXIS2_PLACEMENT_3D ( 'NONE', #19030, #24686, #27020 ) ;
#14337 = VECTOR ( 'NONE', #7773, 1000.000000000000000 ) ;
#14338 = AXIS2_PLACEMENT_3D ( 'NONE', #22426, #27934, #30962 ) ;
#14339 = LINE ( 'NONE', #19317, #23055 ) ;
#14340 = LINE ( 'NONE', #9512, #24595 ) ;
#14341 = CARTESIAN_POINT ( 'NONE',  ( 103.4594491513664849, 5.530628908288163004, -5.066456342206738128 ) ) ;
#14342 =( NAMED_UNIT ( * ) SI_UNIT ( $, .STERADIAN. ) SOLID_ANGLE_UNIT ( ) );
#14343 = DIRECTION ( 'NONE',  ( 1.000000000000000000, -0.000000000000000000, -0.000000000000000000 ) ) ;
#14344 = ORIENTED_EDGE ( 'NONE', *, *, #13945, .F. ) ;
#14345 = CYLINDRICAL_SURFACE ( 'NONE', #25223, 1.999999999999999556 ) ;
#14347 = CARTESIAN_POINT ( 'NONE',  ( 2.765921099433444663, 29.44518845714764765, 9.980709654879525772 ) ) ;
#14346 = DIRECTION ( 'NONE',  ( 0.000000000000000000, 1.000000000000000000, 0.000000000000000000 ) ) ;
#14348 = EDGE_CURVE ( 'NONE', #33511, #28747, #17611, .T. ) ;
#14349 = AXIS2_PLACEMENT_3D ( 'NONE', #2784, #18828, #13479 ) ;
#14350 = EDGE_LOOP ( 'NONE', ( #17029, #29000, #4273, #31292 ) ) ;
#14351 = CARTESIAN_POINT ( 'NONE',  ( -32.32899628990712415, -3.747048406849351032, -15.81122994652406355 ) ) ;
#14352 = PRODUCT_DEFINITION_SHAPE ( 'NONE', 'NONE',  #35101 ) ;
#14353 = CARTESIAN_POINT ( 'NONE',  ( 1.040000000000000924, 0.000000000000000000, 0.000000000000000000 ) ) ;
#14354 = ORIENTED_EDGE ( 'NONE', *, *, #32891, .F. ) ;
#14355 = CIRCLE ( 'NONE', #30231, 3.999999999999976019 ) ;
#14356 = VECTOR ( 'NONE', #17709, 1000.000000000000000 ) ;
#14357 = TOROIDAL_SURFACE ( 'NONE', #3532, 30.47050528711511674, 8.000000000000000000 ) ;
#14358 = EDGE_LOOP ( 'NONE', ( #17648, #28040, #11682, #3368, #30721, #28579, #24619, #944 ) ) ;
#14359 = DIRECTION ( 'NONE',  ( -0.9868265225415262520, 0.1617819965527638459, 2.971887063570155659E-17 ) ) ;
#14360 = EDGE_LOOP ( 'NONE', ( #8618, #8519, #16762, #10067 ) ) ;
#14361 = VERTEX_POINT ( 'NONE', #14929 ) ;
#14362 = DIRECTION ( 'NONE',  ( -1.000000000000000000, -0.000000000000000000, -0.000000000000000000 ) ) ;
#14363 = DIRECTION ( 'NONE',  ( -1.000000000000000000, 0.000000000000000000, 0.000000000000000000 ) ) ;
#14364 = DIRECTION ( 'NONE',  ( -1.000000000000000000, 0.000000000000000000, 0.000000000000000000 ) ) ;
#14365 = CARTESIAN_POINT ( 'NONE',  ( -361.0000000000000000, -125.0000000000000284, 185.0000000000000000 ) ) ;
#14366 = ORIENTED_EDGE ( 'NONE', *, *, #32891, .T. ) ;
#14367 = ORIENTED_EDGE ( 'NONE', *, *, #14858, .F. ) ;
#14368 = DIRECTION ( 'NONE',  ( 3.697785493223492838E-32, 1.934419779023891545E-16, -1.000000000000000000 ) ) ;
#14369 = CARTESIAN_POINT ( 'NONE',  ( 2.261199760692593319, 13.51471344666133412, -30.53246971302630541 ) ) ;
#14370 = CARTESIAN_POINT ( 'NONE',  ( 3.235562306570555532E-30, -15.68591377522703745, -67.50000000000000000 ) ) ;
#14371 = LINE ( 'NONE', #2475, #19284 ) ;
#14372 = CARTESIAN_POINT ( 'NONE',  ( 10.00000000000000000, -1.505030548027689319, 0.000000000000000000 ) ) ;
#14373 = DIRECTION ( 'NONE',  ( -1.000000000000000000, -0.000000000000000000, -0.000000000000000000 ) ) ;
#14374 = ADVANCED_FACE ( 'NONE', ( #25764 ), #14408, .T. ) ;
#14375 = EDGE_CURVE ( 'NONE', #22709, #24311, #34699, .T. ) ;
#14376 = CARTESIAN_POINT ( 'NONE',  ( 145.0000000000000568, -189.5512933739568666, -180.0000000000000284 ) ) ;
#14377 = VERTEX_POINT ( 'NONE', #29132 ) ;
#14378 = DIRECTION ( 'NONE',  ( -0.000000000000000000, -1.000000000000000000, -0.000000000000000000 ) ) ;
#14379 = DIRECTION ( 'NONE',  ( -0.8276889981568902321, -0.5611870653623829419, 0.000000000000000000 ) ) ;
#14380 = AXIS2_PLACEMENT_3D ( 'NONE', #34602, #31909, #9396 ) ;
#14381 = CARTESIAN_POINT ( 'NONE',  ( -445.9999999999999432, 105.0000000000000000, 132.0000000000000000 ) ) ;
#14382 = ORIENTED_EDGE ( 'NONE', *, *, #32847, .F. ) ;
#14383 = CIRCLE ( 'NONE', #154, 30.47050528711511674 ) ;
#14384 = CIRCLE ( 'NONE', #5803, 3.999999999999976019 ) ;
#14385 = CIRCLE ( 'NONE', #26857, 34.41491905851385269 ) ;
#14386 = PLANE ( 'NONE',  #29731 ) ;
#14387 = ORIENTED_EDGE ( 'NONE', *, *, #22301, .F. ) ;
#14388 = B_SPLINE_CURVE_WITH_KNOTS ( 'NONE', 3,
 ( #9433, #31477, #10118, #12458 ),
 .UNSPECIFIED., .F., .F.,
 ( 4, 4 ),
 ( 2.010610498844539582E-07, 0.0006879367828357083612 ),
 .UNSPECIFIED. ) ;
#14389 = DIRECTION ( 'NONE',  ( 0.000000000000000000, -6.123233995736766036E-17, -1.000000000000000000 ) ) ;
#14390 = CARTESIAN_POINT ( 'NONE',  ( -100.1515056346334944, 1.663653002832651495, 12.39274845084345422 ) ) ;
#14391 = EDGE_CURVE ( 'NONE', #27733, #30526, #7233, .T. ) ;
#14392 = ORIENTED_EDGE ( 'NONE', *, *, #25648, .F. ) ;
#14393 = DIRECTION ( 'NONE',  ( -1.000000000000000000, 0.000000000000000000, 0.000000000000000000 ) ) ;
#14394 = CARTESIAN_POINT ( 'NONE',  ( -143.0000000000000568, 85.49999999999998579, -63.00000000000000000 ) ) ;
#14395 = LINE ( 'NONE', #16363, #6343 ) ;
#14396 = ADVANCED_FACE ( 'NONE', ( #23958 ), #18136, .T. ) ;
#14397 = ORIENTED_EDGE ( 'NONE', *, *, #21753, .T. ) ;
#14398 = EDGE_CURVE ( 'NONE', #22483, #23546, #25414, .T. ) ;
#14399 = ADVANCED_FACE ( 'NONE', ( #32155 ), #4553, .T. ) ;
#14400 = DIRECTION ( 'NONE',  ( 0.1063910735369155841, -0.9943243633099125844, -3.335902418025060287E-15 ) ) ;
#14401 = CARTESIAN_POINT ( 'NONE',  ( 29.83064097883987742, 23.32756518004832813, 68.31122994652405112 ) ) ;
#14402 = EDGE_LOOP ( 'NONE', ( #9232, #19740, #32688, #20649, #17512, #9647, #5293, #31679 ) ) ;
#14403 = DIRECTION ( 'NONE',  ( 0.000000000000000000, 1.000000000000000000, 0.000000000000000000 ) ) ;
#14404 = EDGE_CURVE ( 'NONE', #19234, #17537, #26640, .T. ) ;
#14405 = AXIS2_PLACEMENT_3D ( 'NONE', #15135, #25797, #9442 ) ;
#14406 = DIRECTION ( 'NONE',  ( 0.000000000000000000, 0.000000000000000000, -1.000000000000000000 ) ) ;
#14407 = CARTESIAN_POINT ( 'NONE',  ( -31.68358972719163091, 7.440061483287530919, 68.31122994652405112 ) ) ;
#14408 = CYLINDRICAL_SURFACE ( 'NONE', #29025, 16.19999999999999574 ) ;
#14409 = ITEM_DEFINED_TRANSFORMATION ( 'NONE', 'NONE', #17834,  #28566 ) ;
#14410 = VERTEX_POINT ( 'NONE', #25945 ) ;
#14411 = ORIENTED_EDGE ( 'NONE', *, *, #10117, .F. ) ;
#14412 = CIRCLE ( 'NONE', #14963, 4.000000000000003553 ) ;
#14413 = ORIENTED_EDGE ( 'NONE', *, *, #33568, .F. ) ;
#14414 = DIRECTION ( 'NONE',  ( 0.000000000000000000, 0.000000000000000000, -1.000000000000000000 ) ) ;
#14415 = DIRECTION ( 'NONE',  ( 1.000000000000000000, 0.000000000000000000, 0.000000000000000000 ) ) ;
#14416 = LINE ( 'NONE', #25239, #11986 ) ;
#14417 = VERTEX_POINT ( 'NONE', #7581 ) ;
#14418 = EDGE_LOOP ( 'NONE', ( #33599, #19755, #27532, #31839 ) ) ;
#14419 = CARTESIAN_POINT ( 'NONE',  ( -35.00000000000000000, 0.5883377166429051286, 15.81122994652406355 ) ) ;
#14420 = VERTEX_POINT ( 'NONE', #18302 ) ;
#14421 = CARTESIAN_POINT ( 'NONE',  ( -361.0000000000000000, -135.0000000000000000, 126.0000000000000000 ) ) ;
#14422 = CARTESIAN_POINT ( 'NONE',  ( 110.6997470373906225, 0.7624844131070430686, 12.48227001241056833 ) ) ;
#14423 = ORIENTED_EDGE ( 'NONE', *, *, #23237, .T. ) ;
#14424 = ORIENTED_EDGE ( 'NONE', *, *, #5213, .T. ) ;
#14425 = CARTESIAN_POINT ( 'NONE',  ( 5.021133111224265200, -13.65249191622732816, -67.50000000000000000 ) ) ;
#14426 = DIRECTION ( 'NONE',  ( -0.6473862847818281363, -0.7621620551276360178, -1.400068981865441644E-16 ) ) ;
#14427 = ORIENTED_EDGE ( 'NONE', *, *, #34210, .T. ) ;
#14428 = DIRECTION ( 'NONE',  ( 0.9941379571543594862, 0.1081190184239433083, -0.000000000000000000 ) ) ;
#14429 = CARTESIAN_POINT ( 'NONE',  ( -500.0000000000000000, 144.9999999999999716, -155.0000000000000000 ) ) ;
#14430 = LINE ( 'NONE', #1069, #9305 ) ;
#14432 = LINE ( 'NONE', #31265, #23658 ) ;
#14431 = AXIS2_PLACEMENT_3D ( 'NONE', #30972, #25973, #1764 ) ;
#14433 = CIRCLE ( 'NONE', #31453, 7.999999999999979572 ) ;
#14434 = AXIS2_PLACEMENT_3D ( 'NONE', #27230, #24204, #4978 ) ;
#14435 = CARTESIAN_POINT ( 'NONE',  ( -101.8747319636630522, -4.062792622693891076, 11.82295934283893324 ) ) ;
#14436 = FACE_OUTER_BOUND ( 'NONE', #7182, .T. ) ;
#14437 = LINE ( 'NONE', #19418, #6420 ) ;
#14438 = ORIENTED_EDGE ( 'NONE', *, *, #2668, .T. ) ;
#14439 = ADVANCED_FACE ( 'NONE', ( #9921 ), #2253, .T. ) ;
#14440 = ADVANCED_FACE ( 'NONE', ( #23627 ), #4215, .T. ) ;
#14441 = ORIENTED_EDGE ( 'NONE', *, *, #34524, .T. ) ;
#14442 = DIRECTION ( 'NONE',  ( 2.628272706976453364E-14, -1.521162981095489272E-15, 0.9999999999999998890 ) ) ;
#14443 =( REPRESENTATION_RELATIONSHIP ('NONE','NONE', #23037, #15767 ) REPRESENTATION_RELATIONSHIP_WITH_TRANSFORMATION ( #18695 )SHAPE_REPRESENTATION_RELATIONSHIP( ) );
#14444 = ORIENTED_EDGE ( 'NONE', *, *, #26049, .T. ) ;
#14445 = ORIENTED_EDGE ( 'NONE', *, *, #6165, .T. ) ;
#14446 = DIRECTION ( 'NONE',  ( -3.469446951953832974E-18, -1.000000000000000000, -7.888609052210116302E-31 ) ) ;
#14447 = VECTOR ( 'NONE', #5476, 1000.000000000000000 ) ;
#14448 = DIRECTION ( 'NONE',  ( 0.000000000000000000, 0.000000000000000000, 1.000000000000000000 ) ) ;
#14449 = VERTEX_POINT ( 'NONE', #4911 ) ;
#14450 = CARTESIAN_POINT ( 'NONE',  ( -5.781867695661277118, -1.866624223957557893, -0.7500000000000000000 ) ) ;
#14451 = AXIS2_PLACEMENT_3D ( 'NONE', #3860, #23104, #25938 ) ;
#14453 = CARTESIAN_POINT ( 'NONE',  ( 1.155000000000000027, 1.414467053015192904E-16, -0.7500000000000000000 ) ) ;
#14452 = CARTESIAN_POINT ( 'NONE',  ( 11.99999999999995559, -134.9999999999999716, -162.9999999999999432 ) ) ;
#14454 = AXIS2_PLACEMENT_3D ( 'NONE', #14821, #9473, #11809 ) ;
#14455 = ORIENTED_EDGE ( 'NONE', *, *, #4986, .T. ) ;
#14456 = ORIENTED_EDGE ( 'NONE', *, *, #11954, .T. ) ;
#14457 = VECTOR ( 'NONE', #6478, 1000.000000000000000 ) ;
#14458 = CARTESIAN_POINT ( 'NONE',  ( -45.00000000000000000, -46.95407462254104303, 36.69637551990492597 ) ) ;
#14459 = CARTESIAN_POINT ( 'NONE',  ( 22.89764159710613001, 6.310691531022070144, -77.50000000000000000 ) ) ;
#14460 = DIRECTION ( 'NONE',  ( -0.000000000000000000, 2.465190328815661892E-32, 1.000000000000000000 ) ) ;
#14461 = DIRECTION ( 'NONE',  ( 0.000000000000000000, 1.000000000000000000, 5.145227585319922065E-49 ) ) ;
#14462 = ORIENTED_EDGE ( 'NONE', *, *, #33877, .T. ) ;
#14463 = CARTESIAN_POINT ( 'NONE',  ( 0.5288002500384482163, -23.80541455566215348, -23.41327456068897206 ) ) ;
#14464 = DIRECTION ( 'NONE',  ( -0.000000000000000000, -0.000000000000000000, -1.000000000000000000 ) ) ;
#14465 = ORIENTED_EDGE ( 'NONE', *, *, #30216, .T. ) ;
#14466 = DIRECTION ( 'NONE',  ( 0.000000000000000000, -0.000000000000000000, 1.000000000000000000 ) ) ;
#14467 = DIRECTION ( 'NONE',  ( -3.040835319149746528E-31, -1.000000000000000000, 0.000000000000000000 ) ) ;
#14468 = CARTESIAN_POINT ( 'NONE',  ( 7.700000000000000178, 0.000000000000000000, -15.69999999999999929 ) ) ;
#14470 = DIRECTION ( 'NONE',  ( -0.000000000000000000, -0.000000000000000000, 1.000000000000000000 ) ) ;
#14469 = LINE ( 'NONE', #22472, #16180 ) ;
#14471 = VECTOR ( 'NONE', #28437, 1000.000000000000000 ) ;
#14472 = CARTESIAN_POINT ( 'NONE',  ( 8.000000000000003553, 0.000000000000000000, -10.30000000000000071 ) ) ;
#14473 = DIRECTION ( 'NONE',  ( -1.000000000000000000, 0.000000000000000000, 0.000000000000000000 ) ) ;
#14474 = ORIENTED_EDGE ( 'NONE', *, *, #30089, .T. ) ;
#14475 = CARTESIAN_POINT ( 'NONE',  ( 2.765921099433440666, -8.112136323388726922, -30.01377904834218668 ) ) ;
#14476 = DIRECTION ( 'NONE',  ( -1.000000000000000000, -0.000000000000000000, 0.000000000000000000 ) ) ;
#14477 = CIRCLE ( 'NONE', #21840, 1.999999999999999112 ) ;
#14478 = EDGE_CURVE ( 'NONE', #32274, #12335, #34137, .T. ) ;
#14479 = ORIENTED_EDGE ( 'NONE', *, *, #12404, .T. ) ;
#14480 = EDGE_CURVE ( 'NONE', #14078, #5880, #21306, .T. ) ;
#14482 = VERTEX_POINT ( 'NONE', #28616 ) ;
#14481 = VECTOR ( 'NONE', #31392, 1000.000000000000000 ) ;
#14483 = AXIS2_PLACEMENT_3D ( 'NONE', #31857, #23178, #1975 ) ;
#14484 = EDGE_CURVE ( 'NONE', #10828, #8663, #12437, .T. ) ;
#14485 = CIRCLE ( 'NONE', #2511, 32.54542015209056416 ) ;
#14486 = VERTEX_POINT ( 'NONE', #9744 ) ;
#14487 = ORIENTED_EDGE ( 'NONE', *, *, #22748, .F. ) ;
#14488 = CARTESIAN_POINT ( 'NONE',  ( -5.021133111225196011, -23.57973016998034765, -67.50000000000000000 ) ) ;
#14489 = ORIENTED_EDGE ( 'NONE', *, *, #11869, .T. ) ;
#14490 = ORIENTED_EDGE ( 'NONE', *, *, #15158, .F. ) ;
#14491 = CARTESIAN_POINT ( 'NONE',  ( -499.9999999999999432, -113.0000000000000000, -187.0000000000000000 ) ) ;
#14492 = ITEM_DEFINED_TRANSFORMATION ( 'NONE', 'NONE', #32003,  #28566 ) ;
#14493 = VECTOR ( 'NONE', #5914, 1000.000000000000000 ) ;
#14494 = ORIENTED_EDGE ( 'NONE', *, *, #6508, .F. ) ;
#14495 = CARTESIAN_POINT ( 'NONE',  ( 2.789999999999999147, 2.005524111408653720, -31.87689292423236154 ) ) ;
#14496 = FACE_OUTER_BOUND ( 'NONE', #11150, .T. ) ;
#14497 = ORIENTED_EDGE ( 'NONE', *, *, #16050, .T. ) ;
#14498 = EDGE_LOOP ( 'NONE', ( #6392, #7063 ) ) ;
#14499 = CARTESIAN_POINT ( 'NONE',  ( -5.021133111224989953, -3.725253662474303784, -67.50000000000000000 ) ) ;
#14500 = DIRECTION ( 'NONE',  ( -1.000000000000000000, 0.000000000000000000, 0.000000000000000000 ) ) ;
#14501 = FACE_OUTER_BOUND ( 'NONE', #12386, .T. ) ;
#14502 = DIRECTION ( 'NONE',  ( -1.000000000000000000, 0.000000000000000000, 0.000000000000000000 ) ) ;
#14503 = CARTESIAN_POINT ( 'NONE',  ( -355.0000000000000000, -119.0000000000000000, 113.9999999999999858 ) ) ;
#14504 = EDGE_LOOP ( 'NONE', ( #3438, #12424, #31068, #16510 ) ) ;
#14505 = DIRECTION ( 'NONE',  ( -1.000000000000000000, -0.000000000000000000, 0.000000000000000000 ) ) ;
#14506 = CARTESIAN_POINT ( 'NONE',  ( -5.021133111224886036, 8.235406450278427215, -67.50000000000000000 ) ) ;
#14507 = VECTOR ( 'NONE', #497, 1000.000000000000000 ) ;
#14508 = VECTOR ( 'NONE', #17806, 1000.000000000000000 ) ;
#14509 = FACE_OUTER_BOUND ( 'NONE', #30095, .T. ) ;
#14510 = ORIENTED_EDGE ( 'NONE', *, *, #26034, .F. ) ;
#14511 = PRODUCT_DEFINITION_SHAPE ( 'NONE', 'NONE',  #35225 ) ;
#14512 = CARTESIAN_POINT ( 'NONE',  ( -18.45373714011839539, 26.80790850550480542, 68.31122994652405112 ) ) ;
#14513 = DIRECTION ( 'NONE',  ( 0.000000000000000000, 0.000000000000000000, -1.000000000000000000 ) ) ;
#14514 = CARTESIAN_POINT ( 'NONE',  ( 1.394999999999999574, -24.90160365674851661, -23.75493189058366994 ) ) ;
#14515 = DIRECTION ( 'NONE',  ( 1.000000000000000000, 3.469446951953834515E-18, 0.000000000000000000 ) ) ;
#14516 = DIRECTION ( 'NONE',  ( 0.000000000000000000, 0.000000000000000000, -1.000000000000000000 ) ) ;
#14517 = CARTESIAN_POINT ( 'NONE',  ( 0.000000000000000000, 3.524919873834583163E-15, 68.31122994652405112 ) ) ;
#14518 = ORIENTED_EDGE ( 'NONE', *, *, #323, .F. ) ;
#14519 = CARTESIAN_POINT ( 'NONE',  ( -449.9999999999999432, -105.0000000000000142, 162.9999999999999716 ) ) ;
#14521 = DIRECTION ( 'NONE',  ( 1.000000000000000000, -0.000000000000000000, -0.000000000000000000 ) ) ;
#14520 = DIRECTION ( 'NONE',  ( -1.000000000000000000, 0.000000000000000000, 0.000000000000000000 ) ) ;
#14522 = EDGE_CURVE ( 'NONE', #6804, #28125, #3990, .T. ) ;
#14523 = CIRCLE ( 'NONE', #34961, 7.999999999999952038 ) ;
#14524 = ORIENTED_EDGE ( 'NONE', *, *, #32480, .T. ) ;
#14525 = CIRCLE ( 'NONE', #23676, 1.999999999999999112 ) ;
#14526 = DIRECTION ( 'NONE',  ( -0.000000000000000000, 1.000000000000000000, -0.000000000000000000 ) ) ;
#14527 = EDGE_CURVE ( 'NONE', #802, #27628, #28787, .T. ) ;
#14528 = TOROIDAL_SURFACE ( 'NONE', #24734, 30.47050528711511674, 8.000000000000000000 ) ;
#14529 = ORIENTED_EDGE ( 'NONE', *, *, #23966, .F. ) ;
#14530 = ORIENTED_EDGE ( 'NONE', *, *, #7983, .F. ) ;
#14531 = B_SPLINE_CURVE_WITH_KNOTS ( 'NONE', 3,
 ( #5719, #18763, #227, #8229 ),
 .UNSPECIFIED., .F., .F.,
 ( 4, 4 ),
 ( 1.991136383990097483E-07, 0.0006879348191047804937 ),
 .UNSPECIFIED. ) ;
#14532 = EDGE_CURVE ( 'NONE', #17865, #30730, #33579, .T. ) ;
#14533 = VECTOR ( 'NONE', #10830, 1000.000000000000000 ) ;
#14534 = ORIENTED_EDGE ( 'NONE', *, *, #6812, .T. ) ;
#14535 = DIRECTION ( 'NONE',  ( 0.000000000000000000, 1.000000000000000000, 1.224646799147353207E-16 ) ) ;
#14536 = VERTEX_POINT ( 'NONE', #1901 ) ;
#14537 = ORIENTED_EDGE ( 'NONE', *, *, #23306, .F. ) ;
#14538 = DIRECTION ( 'NONE',  ( -0.9052067871510964814, -0.3606673485459944151, -0.2247659586956878841 ) ) ;
#14539 = AXIS2_PLACEMENT_3D ( 'NONE', #24282, #19634, #5585 ) ;
#14540 = ADVANCED_FACE ( 'NONE', ( #20781 ), #20954, .F. ) ;
#14541 = CARTESIAN_POINT ( 'NONE',  ( 2.789999999999999147, -17.83604598421683107, 24.70480026434158916 ) ) ;
#14542 = DIRECTION ( 'NONE',  ( 0.000000000000000000, 0.000000000000000000, 1.000000000000000000 ) ) ;
#14543 = CARTESIAN_POINT ( 'NONE',  ( 1.040000000000001146, 34.10861917999622506, -4.581348211831715034 ) ) ;
#14544 = ORIENTED_EDGE ( 'NONE', *, *, #18175, .F. ) ;
#14545 = VERTEX_POINT ( 'NONE', #27161 ) ;
#14546 = LINE ( 'NONE', #9013, #1443 ) ;
#14547 = LINE ( 'NONE', #17923, #31145 ) ;
#14548 = DIRECTION ( 'NONE',  ( 0.000000000000000000, 2.309213040847544338E-50, 1.000000000000000000 ) ) ;
#14549 = CARTESIAN_POINT ( 'NONE',  ( -361.0000000000000000, -125.0000000000000284, 183.0000000000000000 ) ) ;
#14550 = DIRECTION ( 'NONE',  ( 0.000000000000000000, -1.000000000000000000, 3.374343856708137958E-53 ) ) ;
#14551 = AXIS2_PLACEMENT_3D ( 'NONE', #11164, #17223, #25372 ) ;
#14552 = CARTESIAN_POINT ( 'NONE',  ( 2.765921099433440666, -8.112136323388726922, -30.01377904834218668 ) ) ;
#14553 = DIRECTION ( 'NONE',  ( -1.000000000000000000, -0.000000000000000000, -0.000000000000000000 ) ) ;
#14554 = EDGE_LOOP ( 'NONE', ( #33413, #18696, #7348, #19012 ) ) ;
#14555 = CIRCLE ( 'NONE', #8862, 11.99999999999999645 ) ;
#14556 = CARTESIAN_POINT ( 'NONE',  ( -418.0000000000000000, -137.0000000000000000, -175.0000000000000000 ) ) ;
#14557 = DIRECTION ( 'NONE',  ( 0.000000000000000000, 1.000000000000000000, 1.224646799147353207E-16 ) ) ;
#14558 = CARTESIAN_POINT ( 'NONE',  ( 8.000000000000000000, 1.941065176648554701E-15, 15.69999999999999929 ) ) ;
#14559 = ORIENTED_EDGE ( 'NONE', *, *, #9714, .F. ) ;
#14560 = FACE_OUTER_BOUND ( 'NONE', #1285, .T. ) ;
#14561 = VERTEX_POINT ( 'NONE', #10802 ) ;
#14562 =( LENGTH_UNIT ( ) NAMED_UNIT ( * ) SI_UNIT ( .MILLI., .METRE. ) );
#14564 = VECTOR ( 'NONE', #579, 1000.000000000000000 ) ;
#14563 = CARTESIAN_POINT ( 'NONE',  ( -30.91434716440808472, 10.17386417614053151, 68.31122994652405112 ) ) ;
#14565 = AXIS2_PLACEMENT_3D ( 'NONE', #6496, #3994, #12042 ) ;
#14566 = EDGE_LOOP ( 'NONE', ( #293, #17264, #7118, #30593, #4694, #9381 ) ) ;
#14567 = CARTESIAN_POINT ( 'NONE',  ( 2.765921099433441110, 14.63235270440936731, 27.43224275967444470 ) ) ;
#14568 = CARTESIAN_POINT ( 'NONE',  ( -418.0000000000000000, -141.0000000000000000, 154.9999999999999716 ) ) ;
#14569 = FACE_OUTER_BOUND ( 'NONE', #7449, .T. ) ;
#14570 = ADVANCED_FACE ( 'NONE', ( #27332 ), #26995, .F. ) ;
#14571 = ORIENTED_EDGE ( 'NONE', *, *, #9971, .T. ) ;
#14572 = VECTOR ( 'NONE', #20567, 1000.000000000000000 ) ;
#14573 = ADVANCED_FACE ( 'NONE', ( #18820 ), #24308, .T. ) ;
#14574 = EDGE_CURVE ( 'NONE', #30622, #31862, #21053, .T. ) ;
#14575 = DIRECTION ( 'NONE',  ( -7.893605728314051750E-14, 1.618803117314786530E-15, 1.000000000000000000 ) ) ;
#14576 = FACE_OUTER_BOUND ( 'NONE', #15124, .T. ) ;
#14577 = VERTEX_POINT ( 'NONE', #473 ) ;
#14578 = VECTOR ( 'NONE', #29945, 1000.000000000000000 ) ;
#14579 = FACE_OUTER_BOUND ( 'NONE', #14402, .T. ) ;
#14580 = DIRECTION ( 'NONE',  ( -0.000000000000000000, -0.000000000000000000, -1.000000000000000000 ) ) ;
#14581 = DIRECTION ( 'NONE',  ( 0.4198891015602640997, 0.9075754196709573396, -0.000000000000000000 ) ) ;
#14582 = CARTESIAN_POINT ( 'NONE',  ( -349.0000000000000000, -125.0000000000000284, 128.0000000000000000 ) ) ;
#14583 = CONTEXT_DEPENDENT_SHAPE_REPRESENTATION ( #24639, #6898 ) ;
#14584 = VERTEX_POINT ( 'NONE', #3130 ) ;
#14585 = ORIENTED_EDGE ( 'NONE', *, *, #8101, .T. ) ;
#14586 = VERTEX_POINT ( 'NONE', #27515 ) ;
#14587 = LINE ( 'NONE', #28273, #14051 ) ;
#14588 = VECTOR ( 'NONE', #18888, 1000.000000000000000 ) ;
#14589 = EDGE_CURVE ( 'NONE', #10753, #31620, #23343, .T. ) ;
#14590 = DIRECTION ( 'NONE',  ( 1.000000000000000000, 0.000000000000000000, 0.000000000000000000 ) ) ;
#14591 = VECTOR ( 'NONE', #17570, 1000.000000000000000 ) ;
#14592 = DIRECTION ( 'NONE',  ( -1.000000000000000000, -3.040835319149746528E-31, -1.232595164407830946E-32 ) ) ;
#14593 = CARTESIAN_POINT ( 'NONE',  ( 1.040000000000000924, 0.000000000000000000, 0.000000000000000000 ) ) ;
#14594 = VERTEX_POINT ( 'NONE', #8117 ) ;
#14595 = CARTESIAN_POINT ( 'NONE',  ( -0.7181323043387224381, -1.866624223957557671, 0.000000000000000000 ) ) ;
#14596 = DIRECTION ( 'NONE',  ( 0.000000000000000000, 0.000000000000000000, -1.000000000000000000 ) ) ;
#14597 = EDGE_LOOP ( 'NONE', ( #13727, #13800, #17251, #4219 ) ) ;
#14598 = PRODUCT_DEFINITION_SHAPE ( 'NONE', 'NONE',  #35186 ) ;
#14599 = ADVANCED_FACE ( 'NONE', ( #16508 ), #18250, .T. ) ;
#14600 = LINE ( 'NONE', #3535, #7878 ) ;
#14601 = CARTESIAN_POINT ( 'NONE',  ( 108.5051184359966214, 4.558408617645862471, 11.64136836827557886 ) ) ;
#14602 = ORIENTED_EDGE ( 'NONE', *, *, #3446, .T. ) ;
#14604 = EDGE_CURVE ( 'NONE', #26369, #22562, #29841, .T. ) ;
#14603 = ORIENTED_EDGE ( 'NONE', *, *, #12592, .T. ) ;
#14605 = VECTOR ( 'NONE', #27962, 1000.000000000000000 ) ;
#14606 = LINE ( 'NONE', #8532, #23147 ) ;
#14607 = EDGE_CURVE ( 'NONE', #1041, #8787, #5090, .T. ) ;
#14608 = DIRECTION ( 'NONE',  ( 0.000000000000000000, 1.000000000000000000, 0.000000000000000000 ) ) ;
#14609 = ORIENTED_EDGE ( 'NONE', *, *, #26828, .F. ) ;
#14610 = VECTOR ( 'NONE', #19849, 1000.000000000000114 ) ;
#14611 = CARTESIAN_POINT ( 'NONE',  ( -7.654999999999999361, 1.414467053015192657E-16, -0.7520000000000001128 ) ) ;
#14612 = EDGE_CURVE ( 'NONE', #18684, #11385, #297, .T. ) ;
#14613 = CARTESIAN_POINT ( 'NONE',  ( 15.99999999999998579, -124.9999999999999432, -186.9999999999999716 ) ) ;
#14614 = DIRECTION ( 'NONE',  ( 0.000000000000000000, -2.309213040847544338E-50, -1.000000000000000000 ) ) ;
#14615 = CARTESIAN_POINT ( 'NONE',  ( 15.99999999999998579, 112.9999999999999574, 155.0000000000000000 ) ) ;
#14616 =( NAMED_UNIT ( * ) SI_UNIT ( $, .STERADIAN. ) SOLID_ANGLE_UNIT ( ) );
#14617 = CIRCLE ( 'NONE', #30500, 2.524999999999999911 ) ;
#14618 = ORIENTED_EDGE ( 'NONE', *, *, #27911, .F. ) ;
#14619 = ORIENTED_EDGE ( 'NONE', *, *, #15807, .F. ) ;
#14620 = EDGE_CURVE ( 'NONE', #9042, #3150, #5784, .T. ) ;
#14621 = EDGE_CURVE ( 'NONE', #17657, #25488, #11335, .T. ) ;
#14622 = DIRECTION ( 'NONE',  ( 2.631201909438060269E-14, -5.396010391056495992E-16, 0.9999999999999998890 ) ) ;
#14623 = ORIENTED_EDGE ( 'NONE', *, *, #12742, .T. ) ;
#14624 = ORIENTED_EDGE ( 'NONE', *, *, #19419, .T. ) ;
#14625 = AXIS2_PLACEMENT_3D ( 'NONE', #4970, #32554, #21370 ) ;
#14626 = LINE ( 'NONE', #14086, #11281 ) ;
#14627 = VECTOR ( 'NONE', #1740, 1000.000000000000000 ) ;
#14628 = CARTESIAN_POINT ( 'NONE',  ( 19.99999999999998934, 124.9999999999999716, 162.9999999999999716 ) ) ;
#14629 = CONTEXT_DEPENDENT_SHAPE_REPRESENTATION ( #32138, #19741 ) ;
#14630 = ORIENTED_EDGE ( 'NONE', *, *, #12555, .T. ) ;
#14631 = DIRECTION ( 'NONE',  ( 0.000000000000000000, 1.836970198721029934E-16, -1.000000000000000000 ) ) ;
#14632 = SURFACE_STYLE_FILL_AREA ( #28485 ) ;
#14634 = CARTESIAN_POINT ( 'NONE',  ( -35.00000000000000000, -4.831299144296466785, -15.81122994652406355 ) ) ;
#14633 = DIRECTION ( 'NONE',  ( -1.000000000000000000, -0.000000000000000000, -0.000000000000000000 ) ) ;
#14635 = VERTEX_POINT ( 'NONE', #11161 ) ;
#14636 = ORIENTED_EDGE ( 'NONE', *, *, #9360, .F. ) ;
#14637 = CARTESIAN_POINT ( 'NONE',  ( -1.307386931792819285, 37.83772838912472025, -36.68877005347593467 ) ) ;
#14638 = LINE ( 'NONE', #17132, #34588 ) ;
#14639 = FACE_BOUND ( 'NONE', #19295, .T. ) ;
#14640 = DIRECTION ( 'NONE',  ( 0.000000000000000000, -1.000000000000000000, 0.000000000000000000 ) ) ;
#14641 = ORIENTED_EDGE ( 'NONE', *, *, #5856, .T. ) ;
#14642 = EDGE_CURVE ( 'NONE', #26390, #32063, #14261, .T. ) ;
#14643 = DIRECTION ( 'NONE',  ( 0.000000000000000000, 0.000000000000000000, -1.000000000000000000 ) ) ;
#14644 = EDGE_CURVE ( 'NONE', #23263, #5461, #22182, .T. ) ;
#14645 = FACE_OUTER_BOUND ( 'NONE', #17979, .T. ) ;
#14646 = ORIENTED_EDGE ( 'NONE', *, *, #1082, .F. ) ;
#14647 = DIRECTION ( 'NONE',  ( 1.000000000000000000, 0.000000000000000000, -0.000000000000000000 ) ) ;
#14648 = CIRCLE ( 'NONE', #5509, 4.750000000000004441 ) ;
#14649 = CARTESIAN_POINT ( 'NONE',  ( 28.23027531293552528, -10.15143121711728469, 20.00000000000000000 ) ) ;
#14650 = CARTESIAN_POINT ( 'NONE',  ( 2.789999999999999147, -31.68806325674604452, -4.003133335385915537 ) ) ;
#14652 = LINE ( 'NONE', #30657, #23639 ) ;
#14651 = DIRECTION ( 'NONE',  ( -1.300283923313630633E-47, 0.000000000000000000, -1.000000000000000000 ) ) ;
#14653 = CIRCLE ( 'NONE', #20329, 2.524999999999999911 ) ;
#14654 = AXIS2_PLACEMENT_3D ( 'NONE', #31726, #26739, #7334 ) ;
#14656 = ADVANCED_FACE ( 'NONE', ( #29664 ), #32677, .T. ) ;
#14655 = DIRECTION ( 'NONE',  ( -0.000000000000000000, 1.836970198721029688E-16, -1.000000000000000000 ) ) ;
#14657 = DIRECTION ( 'NONE',  ( -0.000000000000000000, -0.000000000000000000, 1.000000000000000000 ) ) ;
#14658 = ORIENTED_EDGE ( 'NONE', *, *, #557, .T. ) ;
#14659 = DIRECTION ( 'NONE',  ( -0.000000000000000000, 1.836970198721029934E-16, -1.000000000000000000 ) ) ;
#14660 = DIRECTION ( 'NONE',  ( -0.9818488882034280829, -0.1609659548241205163, 0.1003131203843820873 ) ) ;
#14661 = TOROIDAL_SURFACE ( 'NONE', #12389, 30.47050528711511674, 8.000000000000000000 ) ;
#14662 = ORIENTED_EDGE ( 'NONE', *, *, #7050, .F. ) ;
#14663 =( LENGTH_UNIT ( ) NAMED_UNIT ( * ) SI_UNIT ( .MILLI., .METRE. ) );
#14664 = ORIENTED_EDGE ( 'NONE', *, *, #2951, .T. ) ;
#14665 = CIRCLE ( 'NONE', #16931, 2.525000000000000799 ) ;
#14666 = ORIENTED_EDGE ( 'NONE', *, *, #16264, .T. ) ;
#14667 = CARTESIAN_POINT ( 'NONE',  ( -20.00000000000007461, 136.9999999999999432, 187.0000000000000000 ) ) ;
#14668 = ORIENTED_EDGE ( 'NONE', *, *, #21846, .T. ) ;
#14669 = EDGE_LOOP ( 'NONE', ( #7907, #28039, #16853, #31698 ) ) ;
#14670 = ADVANCED_FACE ( 'NONE', ( #13823 ), #21482, .T. ) ;
#14671 = DIRECTION ( 'NONE',  ( 0.000000000000000000, 1.836970198721029441E-16, -1.000000000000000000 ) ) ;
#14672 = CONTEXT_DEPENDENT_SHAPE_REPRESENTATION ( #28561, #20957 ) ;
#14673 = AXIS2_PLACEMENT_3D ( 'NONE', #21930, #8567, #30285 ) ;
#14674 = VECTOR ( 'NONE', #712, 1000.000000000000000 ) ;
#14675 = VERTEX_POINT ( 'NONE', #8475 ) ;
#14676 = LINE ( 'NONE', #22842, #22633 ) ;
#14677 = DIRECTION ( 'NONE',  ( 0.1617819965527648451, -0.9868265225415261410, -1.812770913216290044E-16 ) ) ;
#14678 = EDGE_LOOP ( 'NONE', ( #21999, #450, #20457, #7631 ) ) ;
#14679 = ORIENTED_EDGE ( 'NONE', *, *, #9331, .T. ) ;
#14680 = CARTESIAN_POINT ( 'NONE',  ( 1.040000000000000924, 0.000000000000000000, 0.000000000000000000 ) ) ;
#14681 = DIRECTION ( 'NONE',  ( -1.000000000000000000, 0.000000000000000000, 0.000000000000000000 ) ) ;
#14682 = EDGE_CURVE ( 'NONE', #18383, #24429, #20502, .T. ) ;
#14683 = CARTESIAN_POINT ( 'NONE',  ( 0.000000000000000000, 17.98401995359670025, -24.59729088254937324 ) ) ;
#14684 = CARTESIAN_POINT ( 'NONE',  ( 0.000000000000000000, 27.60935207499554522, 12.89090262359660422 ) ) ;
#14685 = CARTESIAN_POINT ( 'NONE',  ( 2.790000000000083080, 29.09328061627297757, 9.684256520155898329 ) ) ;
#14686 = ORIENTED_EDGE ( 'NONE', *, *, #14644, .F. ) ;
#14687 = ADVANCED_FACE ( 'NONE', ( #24135 ), #22359, .T. ) ;
#14688 = FACE_OUTER_BOUND ( 'NONE', #34977, .T. ) ;
#14689 = EDGE_CURVE ( 'NONE', #23884, #31849, #22540, .T. ) ;
#14690 = LINE ( 'NONE', #30689, #5063 ) ;
#14691 = ORIENTED_EDGE ( 'NONE', *, *, #12426, .F. ) ;
#14692 = CARTESIAN_POINT ( 'NONE',  ( -15.99999999999998579, 144.9999999999999716, -162.9999999999999147 ) ) ;
#14693 = FACE_OUTER_BOUND ( 'NONE', #25617, .T. ) ;
#14694 = LINE ( 'NONE', #25697, #21789 ) ;
#14695 = CARTESIAN_POINT ( 'NONE',  ( 99.88047028666090910, 2.618976401886136340, -7.037310091161540271 ) ) ;
#14697 = CYLINDRICAL_SURFACE ( 'NONE', #7665, 14.77500000000000036 ) ;
#14696 = CARTESIAN_POINT ( 'NONE',  ( 11.99999999999999645, 144.9999999999999716, -194.9999999999999432 ) ) ;
#14698 = AXIS2_PLACEMENT_3D ( 'NONE', #3083, #13961, #24796 ) ;
#14699 = DIRECTION ( 'NONE',  ( 1.000000000000000000, 0.000000000000000000, -1.848892746611746966E-32 ) ) ;
#14700 = ORIENTED_EDGE ( 'NONE', *, *, #670, .F. ) ;
#14702 = CARTESIAN_POINT ( 'NONE',  ( -8.304372355306091180E-14, 20.82920972943067284, -22.50217193233280000 ) ) ;
#14701 = B_SPLINE_CURVE_WITH_KNOTS ( 'NONE', 3,
 ( #32140, #24291, #12943, #32311, #26978, #19162 ),
 .UNSPECIFIED., .F., .F.,
 ( 4, 2, 4 ),
 ( 4.404817164018835850E-07, 0.001874269726455596438, 0.003748098971194791310 ),
 .UNSPECIFIED. ) ;
#14704 = LINE ( 'NONE', #17719, #3201 ) ;
#14703 = LINE ( 'NONE', #30873, #15421 ) ;
#14705 = COLOUR_RGB ( '',0.7921568627450980005, 0.8196078431372548767, 0.9333333333333333481 ) ;
#14706 = VERTEX_POINT ( 'NONE', #6315 ) ;
#14707 =( REPRESENTATION_RELATIONSHIP ('NONE','NONE', #23037, #28231 ) REPRESENTATION_RELATIONSHIP_WITH_TRANSFORMATION ( #10185 )SHAPE_REPRESENTATION_RELATIONSHIP( ) );
#14708 = AXIS2_PLACEMENT_3D ( 'NONE', #28092, #11557, #8692 ) ;
#14709 = CARTESIAN_POINT ( 'NONE',  ( 1.040000000000000924, 0.000000000000000000, 0.000000000000000000 ) ) ;
#14710 = ORIENTED_EDGE ( 'NONE', *, *, #28453, .F. ) ;
#14711 = VECTOR ( 'NONE', #18748, 1000.000000000000000 ) ;
#14712 = ORIENTED_EDGE ( 'NONE', *, *, #13182, .T. ) ;
#14713 = CARTESIAN_POINT ( 'NONE',  ( 106.9079130804741595, -5.424061631995436450, -5.183681401394261812 ) ) ;
#14714 = VERTEX_POINT ( 'NONE', #17041 ) ;
#14715 = ORIENTED_EDGE ( 'NONE', *, *, #681, .F. ) ;
#14716 = CARTESIAN_POINT ( 'NONE',  ( -12.00000000000001066, 144.9999999999999716, 162.9999999999999716 ) ) ;
#14717 = VECTOR ( 'NONE', #27785, 1000.000000000000000 ) ;
#14718 = CARTESIAN_POINT ( 'NONE',  ( 0.07094834062134731945, -11.11627562454433082, 29.68062877649318665 ) ) ;
#14719 = CARTESIAN_POINT ( 'NONE',  ( -11.99999999999998224, -145.0000000000000000, 162.9999999999999716 ) ) ;
#14720 = CARTESIAN_POINT ( 'NONE',  ( 11.99999999999999645, -124.9999999999999432, -162.9999999999999432 ) ) ;
#14721 = VERTEX_POINT ( 'NONE', #17220 ) ;
#14722 = ORIENTED_EDGE ( 'NONE', *, *, #22508, .T. ) ;
#14723 = EDGE_CURVE ( 'NONE', #16741, #24257, #19523, .T. ) ;
#14724 = CARTESIAN_POINT ( 'NONE',  ( 1.040000000000001368, 6.714005886385424837, -33.75364837705166110 ) ) ;
#14725 = DIRECTION ( 'NONE',  ( 0.9635499925192230197, 0.2675283385292205329, 0.000000000000000000 ) ) ;
#14726 = CYLINDRICAL_SURFACE ( 'NONE', #7813, 14.20000000000000107 ) ;
#14727 = EDGE_CURVE ( 'NONE', #1001, #14361, #19700, .T. ) ;
#14728 = CARTESIAN_POINT ( 'NONE',  ( 2.789999999999999147, -30.41598411195409923, 1.821977758773558165 ) ) ;
#14729 = CARTESIAN_POINT ( 'NONE',  ( -363.0000000000000000, -125.0000000000000284, 168.9999999999999716 ) ) ;
#14730 = DIRECTION ( 'NONE',  ( 0.000000000000000000, 1.000000000000000000, 0.000000000000000000 ) ) ;
#14731 = ADVANCED_FACE ( 'NONE', ( #30895 ), #28228, .F. ) ;
#14732 = DIRECTION ( 'NONE',  ( 1.000000000000000000, -0.000000000000000000, -0.000000000000000000 ) ) ;
#14733 = ORIENTED_EDGE ( 'NONE', *, *, #5837, .T. ) ;
#14734 = ADVANCED_FACE ( 'NONE', ( #3825 ), #1171, .T. ) ;
#14735 = LINE ( 'NONE', #7205, #8328 ) ;
#14736 = CARTESIAN_POINT ( 'NONE',  ( -418.0000000000000000, -105.0000000000000142, -69.99999999999998579 ) ) ;
#14737 = CIRCLE ( 'NONE', #34605, 15.69999999999999929 ) ;
#14738 = CARTESIAN_POINT ( 'NONE',  ( -499.9999999999999432, 112.9999999999999574, 190.9999999999999716 ) ) ;
#14739 = VERTEX_POINT ( 'NONE', #25545 ) ;
#14740 = DIRECTION ( 'NONE',  ( 0.000000000000000000, 1.000000000000000000, 5.053935297177146739E-49 ) ) ;
#14741 = ORIENTED_EDGE ( 'NONE', *, *, #17734, .T. ) ;
#14742 = CARTESIAN_POINT ( 'NONE',  ( -103.3401862807116629, 4.841160850826510043, 11.52458411820204276 ) ) ;
#14743 = ADVANCED_FACE ( 'NONE', ( #12044 ), #5965, .F. ) ;
#14744 = CIRCLE ( 'NONE', #26659, 13.50000000000000178 ) ;
#14745 = ORIENTED_EDGE ( 'NONE', *, *, #28297, .F. ) ;
#14746 = CARTESIAN_POINT ( 'NONE',  ( 2.604019706987809712, 14.82665350068097254, 28.67542985682328549 ) ) ;
#14747 = DIRECTION ( 'NONE',  ( 0.9868265225415260300, 0.1617819965527650394, -0.000000000000000000 ) ) ;
#14748 = DIRECTION ( 'NONE',  ( 1.000000000000000000, 0.000000000000000000, 0.000000000000000000 ) ) ;
#14749 = ORIENTED_EDGE ( 'NONE', *, *, #34974, .T. ) ;
#14750 = CIRCLE ( 'NONE', #9065, 8.000000000000007105 ) ;
#14751 = CARTESIAN_POINT ( 'NONE',  ( 792.6528868835252979, 1003.674412348182386, 1753.598338701303419 ) ) ;
#14752 = DIRECTION ( 'NONE',  ( -0.000000000000000000, 1.836970198721029934E-16, -1.000000000000000000 ) ) ;
#14753 = ORIENTED_EDGE ( 'NONE', *, *, #14235, .F. ) ;
#14754 = LINE ( 'NONE', #31114, #14471 ) ;
#14755 = VECTOR ( 'NONE', #21447, 1000.000000000000000 ) ;
#14756 = CARTESIAN_POINT ( 'NONE',  ( -12.00000000000001066, -145.0000000000000000, 190.9999999999999716 ) ) ;
#14757 = DIRECTION ( 'NONE',  ( -3.040835319149746090E-31, -1.000000000000000000, 0.000000000000000000 ) ) ;
#14758 = CARTESIAN_POINT ( 'NONE',  ( -418.0000000000000000, -125.0000000000000000, 100.0000000000000000 ) ) ;
#14759 = ORIENTED_EDGE ( 'NONE', *, *, #7401, .T. ) ;
#14760 = VERTEX_POINT ( 'NONE', #14184 ) ;
#14761 = ORIENTED_EDGE ( 'NONE', *, *, #3010, .F. ) ;
#14762 = SURFACE_STYLE_FILL_AREA ( #14047 ) ;
#14763 = CARTESIAN_POINT ( 'NONE',  ( 0.000000000000000000, 30.93646776788807173, -7.943134866715984899 ) ) ;
#14764 = DIRECTION ( 'NONE',  ( 0.000000000000000000, 1.310824597558155437E-49, 1.000000000000000000 ) ) ;
#14765 = AXIS2_PLACEMENT_3D ( 'NONE', #9135, #20010, #30855 ) ;
#14766 = CARTESIAN_POINT ( 'NONE',  ( 19.99999999999990763, -134.9999999999999716, -186.9999999999999716 ) ) ;
#14767 = ORIENTED_EDGE ( 'NONE', *, *, #7701, .F. ) ;
#14768 = CYLINDRICAL_SURFACE ( 'NONE', #21418, 7.999999999999979572 ) ;
#14769 = CARTESIAN_POINT ( 'NONE',  ( -442.0000000000000000, 113.0000000000000000, -155.0000000000000000 ) ) ;
#14770 = ORIENTED_EDGE ( 'NONE', *, *, #5835, .T. ) ;
#14771 = EDGE_CURVE ( 'NONE', #23775, #15441, #33736, .T. ) ;
#14772 = DIRECTION ( 'NONE',  ( -1.000000000000000000, 6.792721752314501023E-48, -3.697785493223492838E-32 ) ) ;
#14773 = EDGE_CURVE ( 'NONE', #5171, #26118, #13143, .T. ) ;
#14774 = CARTESIAN_POINT ( 'NONE',  ( 104.8142247405124152, 5.738231822805250459, 11.10507521702373879 ) ) ;
#14775 = ORIENTED_EDGE ( 'NONE', *, *, #6964, .F. ) ;
#14776 = CARTESIAN_POINT ( 'NONE',  ( 2.719051671364112632, -8.452579892119949534, 30.54611582031328609 ) ) ;
#14777 = EDGE_CURVE ( 'NONE', #10245, #30258, #30763, .T. ) ;
#14778 = EDGE_CURVE ( 'NONE', #29101, #11797, #17130, .T. ) ;
#14779 = DIRECTION ( 'NONE',  ( -1.000000000000000000, 6.792721752314501023E-48, -3.697785493223492838E-32 ) ) ;
#14780 = VERTEX_POINT ( 'NONE', #14365 ) ;
#14781 = CARTESIAN_POINT ( 'NONE',  ( 2.789999999999999147, -11.13185981125856827, -28.36429779836962339 ) ) ;
#14782 = SURFACE_STYLE_USAGE ( .BOTH. , #6032 ) ;
#14783 = PLANE ( 'NONE',  #210 ) ;
#14784 = AXIS2_PLACEMENT_3D ( 'NONE', #14177, #12508, #33198 ) ;
#14785 = LINE ( 'NONE', #1240, #32463 ) ;
#14786 = CARTESIAN_POINT ( 'NONE',  ( 22.89764159710611224, 15.60017778382161424, -87.50000000000000000 ) ) ;
#14787 = CARTESIAN_POINT ( 'NONE',  ( 1.040000000000000702, 22.14447232807505728, 26.34405054495564968 ) ) ;
#14789 = ADVANCED_FACE ( 'NONE', ( #11506 ), #11872, .F. ) ;
#14788 = VERTEX_POINT ( 'NONE', #3476 ) ;
#14790 = VECTOR ( 'NONE', #33836, 1000.000000000000000 ) ;
#14791 = ORIENTED_EDGE ( 'NONE', *, *, #21057, .F. ) ;
#14792 = DIRECTION ( 'NONE',  ( -7.893605728314050488E-14, 1.618803117314786135E-15, 0.9999999999999998890 ) ) ;
#14793 = ORIENTED_EDGE ( 'NONE', *, *, #22851, .F. ) ;
#14794 = FACE_BOUND ( 'NONE', #27925, .T. ) ;
#14795 = EDGE_CURVE ( 'NONE', #26863, #11290, #15875, .T. ) ;
#14796 = EDGE_CURVE ( 'NONE', #9427, #5512, #9167, .T. ) ;
#14797 = DIRECTION ( 'NONE',  ( 0.000000000000000000, 2.309213040847544338E-50, 1.000000000000000000 ) ) ;
#14798 = ORIENTED_EDGE ( 'NONE', *, *, #19174, .T. ) ;
#14799 = DIRECTION ( 'NONE',  ( 1.000000000000000000, 0.000000000000000000, 0.000000000000000000 ) ) ;
#14800 = CARTESIAN_POINT ( 'NONE',  ( -109.0561609099978142, -3.120668149329707042, -12.10491939767606873 ) ) ;
#14802 = DIRECTION ( 'NONE',  ( 0.000000000000000000, 1.131431318426415506E-52, 1.000000000000000000 ) ) ;
#14801 = CARTESIAN_POINT ( 'NONE',  ( -12.00000000000001066, 124.9999999999999716, 155.0000000000000000 ) ) ;
#14803 = ORIENTED_EDGE ( 'NONE', *, *, #28290, .F. ) ;
#14804 = ORIENTED_EDGE ( 'NONE', *, *, #33054, .T. ) ;
#14805 = DIRECTION ( 'NONE',  ( 0.000000000000000000, 0.000000000000000000, 1.000000000000000000 ) ) ;
#14806 = DIRECTION ( 'NONE',  ( 0.000000000000000000, 1.131431318426415506E-52, 1.000000000000000000 ) ) ;
#14807 = DIRECTION ( 'NONE',  ( 0.000000000000000000, -1.000000000000000000, -1.836970198721029934E-16 ) ) ;
#14808 = ORIENTED_EDGE ( 'NONE', *, *, #28887, .F. ) ;
#14809 = LINE ( 'NONE', #22462, #18568 ) ;
#14810 = DIRECTION ( 'NONE',  ( -1.300283923313630633E-47, 0.000000000000000000, -1.000000000000000000 ) ) ;
#14811 = EDGE_CURVE ( 'NONE', #16642, #11839, #1000, .T. ) ;
#14812 = DIRECTION ( 'NONE',  ( 1.000000000000000000, 0.000000000000000000, 0.000000000000000000 ) ) ;
#14813 = EDGE_CURVE ( 'NONE', #10508, #22962, #20527, .T. ) ;
#14814 = EDGE_LOOP ( 'NONE', ( #11326, #21262, #27490, #32789 ) ) ;
#14815 = LINE ( 'NONE', #9287, #8374 ) ;
#14816 = CARTESIAN_POINT ( 'NONE',  ( -37.85301660235036536, 0.7430237821112573027, 68.31122994652405112 ) ) ;
#14817 = EDGE_CURVE ( 'NONE', #916, #33934, #24345, .T. ) ;
#14818 = FACE_OUTER_BOUND ( 'NONE', #8947, .T. ) ;
#14820 = CARTESIAN_POINT ( 'NONE',  ( -11.83261234297099662, -30.31820670846266097, -36.68877005347593467 ) ) ;
#14819 = PLANE ( 'NONE',  #20166 ) ;
#14821 = CARTESIAN_POINT ( 'NONE',  ( -418.0000000000000000, -141.0000000000000000, -175.0000000000000000 ) ) ;
#14822 = CYLINDRICAL_SURFACE ( 'NONE', #19963, 4.682234377621698584 ) ;
#14823 = ORIENTED_EDGE ( 'NONE', *, *, #20624, .F. ) ;
#14824 = CARTESIAN_POINT ( 'NONE',  ( 19.99999999999998934, -32.99999999999997158, 155.0000000000000000 ) ) ;
#14825 = DIRECTION ( 'NONE',  ( 0.000000000000000000, 1.000000000000000000, 0.000000000000000000 ) ) ;
#14826 = VECTOR ( 'NONE', #30362, 1000.000000000000114 ) ;
#14827 = ORIENTED_EDGE ( 'NONE', *, *, #27651, .F. ) ;
#14828 = ORIENTED_EDGE ( 'NONE', *, *, #34559, .F. ) ;
#14830 = VERTEX_POINT ( 'NONE', #20908 ) ;
#14829 = EDGE_CURVE ( 'NONE', #15936, #11473, #31753, .T. ) ;
#14831 = EDGE_CURVE ( 'NONE', #17516, #731, #26073, .T. ) ;
#14832 = ADVANCED_FACE ( 'NONE', ( #7191 ), #28745, .F. ) ;
#14833 = VECTOR ( 'NONE', #15910, 1000.000000000000000 ) ;
#14834 = CARTESIAN_POINT ( 'NONE',  ( 22.50000000000000355, 2.755455298081545172E-15, 20.00000000000000000 ) ) ;
#14835 = VECTOR ( 'NONE', #6785, 1000.000000000000000 ) ;
#14836 = VERTEX_POINT ( 'NONE', #10054 ) ;
#14837 = ORIENTED_EDGE ( 'NONE', *, *, #11869, .F. ) ;
#14838 = ORIENTED_EDGE ( 'NONE', *, *, #20666, .F. ) ;
#14839 = CARTESIAN_POINT ( 'NONE',  ( -361.0000000000000000, -125.0000000000000284, 113.9999999999999858 ) ) ;
#14840 = EDGE_CURVE ( 'NONE', #8592, #8166, #14855, .T. ) ;
#14841 = ITEM_DEFINED_TRANSFORMATION ( 'NONE', 'NONE', #19530,  #28566 ) ;
#14842 = EDGE_CURVE ( 'NONE', #25806, #15766, #23401, .T. ) ;
#14843 = ORIENTED_EDGE ( 'NONE', *, *, #28523, .F. ) ;
#14844 = LINE ( 'NONE', #15014, #24870 ) ;
#14845 = DIRECTION ( 'NONE',  ( -1.000000000000000000, 0.000000000000000000, 0.000000000000000000 ) ) ;
#14846 = ORIENTED_EDGE ( 'NONE', *, *, #21804, .F. ) ;
#14847 = ORIENTED_EDGE ( 'NONE', *, *, #9121, .T. ) ;
#14848 = LINE ( 'NONE', #32415, #19697 ) ;
#14850 = FACE_OUTER_BOUND ( 'NONE', #11861, .T. ) ;
#14849 = AXIS2_PLACEMENT_3D ( 'NONE', #31087, #25732, #1358 ) ;
#14851 = CARTESIAN_POINT ( 'NONE',  ( -500.0000000000000000, 144.9999999999999716, 155.0000000000000000 ) ) ;
#14852 = CARTESIAN_POINT ( 'NONE',  ( -410.0000000000000568, -137.0000000000000000, -175.0000000000000000 ) ) ;
#14853 = DIRECTION ( 'NONE',  ( -1.000000000000000000, 0.000000000000000000, 0.000000000000000000 ) ) ;
#14854 = VERTEX_POINT ( 'NONE', #20741 ) ;
#14855 = CIRCLE ( 'NONE', #4018, 3.999999999999982681 ) ;
#14856 = FACE_OUTER_BOUND ( 'NONE', #8103, .T. ) ;
#14857 = CARTESIAN_POINT ( 'NONE',  ( 0.000000000000000000, 3.172845296185191895E-14, -85.22165320886810491 ) ) ;
#14858 = EDGE_CURVE ( 'NONE', #6669, #6498, #16554, .T. ) ;
#14859 = CARTESIAN_POINT ( 'NONE',  ( -3.250000000000000000, -5.838643359331793015, 5.429999999999999716 ) ) ;
#14860 = VERTEX_POINT ( 'NONE', #31243 ) ;
#14861 = CARTESIAN_POINT ( 'NONE',  ( 0.2204769333330968695, 13.33789614101571885, 3.898086217683919941 ) ) ;
#14862 = CARTESIAN_POINT ( 'NONE',  ( -15.00000000000000000, 0.000000000000000000, 20.00000000000000000 ) ) ;
#14863 = CARTESIAN_POINT ( 'NONE',  ( 10.00000000000000000, -1.505030548027689319, 0.000000000000000000 ) ) ;
#14864 = CARTESIAN_POINT ( 'NONE',  ( 100.7130364623890131, 3.831042253767035444, -6.454752727393734624 ) ) ;
#14866 = FILL_AREA_STYLE ('',( #6473 ) ) ;
#14865 = CARTESIAN_POINT ( 'NONE',  ( 1.205771365940050854, -7.794228634059966687, -13.49999999999999822 ) ) ;
#14867 = VECTOR ( 'NONE', #34195, 1000.000000000000000 ) ;
#14868 = LINE ( 'NONE', #25701, #25199 ) ;
#14870 = VERTEX_POINT ( 'NONE', #1525 ) ;
#14869 = VECTOR ( 'NONE', #18524, 1000.000000000000000 ) ;
#14871 = FACE_OUTER_BOUND ( 'NONE', #15956, .T. ) ;
#14873 = CARTESIAN_POINT ( 'NONE',  ( -12.00000000000001066, -56.99999999999997868, -154.9999999999999716 ) ) ;
#14872 = CARTESIAN_POINT ( 'NONE',  ( 1.749999999999999778, 0.000000000000000000, 0.000000000000000000 ) ) ;
#14874 = ORIENTED_EDGE ( 'NONE', *, *, #5386, .T. ) ;
#14875 = CARTESIAN_POINT ( 'NONE',  ( -12.00000000000001066, 134.9999999999999432, -162.9999999999999432 ) ) ;
#14876 = AXIS2_PLACEMENT_3D ( 'NONE', #10555, #26733, #11079 ) ;
#14877 = ORIENTED_EDGE ( 'NONE', *, *, #27509, .F. ) ;
#14878 = AXIS2_PLACEMENT_3D ( 'NONE', #12270, #14590, #28093 ) ;
#14879 = EDGE_CURVE ( 'NONE', #16498, #842, #7537, .T. ) ;
#14880 = ADVANCED_FACE ( 'NONE', ( #26241 ), #34259, .F. ) ;
#14881 = VERTEX_POINT ( 'NONE', #9539 ) ;
#14882 = CARTESIAN_POINT ( 'NONE',  ( 105.7869846758901815, -5.687305096039679597, -4.889329717555864541 ) ) ;
#14883 = VERTEX_POINT ( 'NONE', #20400 ) ;
#14884 = ORIENTED_EDGE ( 'NONE', *, *, #31414, .T. ) ;
#14885 = DIRECTION ( 'NONE',  ( 0.000000000000000000, 1.000000000000000000, 1.934419779023891545E-16 ) ) ;
#14886 = PRODUCT_DEFINITION_SHAPE ( 'NONE', 'NONE',  #35172 ) ;
#14887 = LINE ( 'NONE', #12220, #22698 ) ;
#14888 = CARTESIAN_POINT ( 'NONE',  ( -12.00000000000006573, -145.0000000000000000, -186.9999999999999716 ) ) ;
#14889 = VECTOR ( 'NONE', #16920, 1000.000000000000000 ) ;
#14890 = DIRECTION ( 'NONE',  ( -1.000000000000000000, 0.000000000000000000, 0.000000000000000000 ) ) ;
#14891 = ORIENTED_EDGE ( 'NONE', *, *, #114, .T. ) ;
#14892 = ORIENTED_EDGE ( 'NONE', *, *, #7487, .F. ) ;
#14893 = VECTOR ( 'NONE', #19903, 1000.000000000000000 ) ;
#14894 = DIRECTION ( 'NONE',  ( 0.000000000000000000, 0.000000000000000000, 1.000000000000000000 ) ) ;
#14895 = LINE ( 'NONE', #12049, #9521 ) ;
#14896 = VECTOR ( 'NONE', #6831, 1000.000000000000000 ) ;
#14897 = CARTESIAN_POINT ( 'NONE',  ( 32.05156013847309993, -20.15193397489277771, 68.31122994652405112 ) ) ;
#14898 = DIRECTION ( 'NONE',  ( 0.000000000000000000, 0.000000000000000000, 1.000000000000000000 ) ) ;
#14899 = LINE ( 'NONE', #14372, #9133 ) ;
#14900 = DIRECTION ( 'NONE',  ( 0.7621620551276356847, -0.6473862847818285804, -1.189229312204944401E-16 ) ) ;
#14901 = DIRECTION ( 'NONE',  ( 0.000000000000000000, 1.000000000000000000, 0.000000000000000000 ) ) ;
#14902 = VERTEX_POINT ( 'NONE', #6841 ) ;
#14903 = FACE_OUTER_BOUND ( 'NONE', #22837, .T. ) ;
#14904 = CARTESIAN_POINT ( 'NONE',  ( 2.789999999999999591, -11.08319859408639374, 28.58839307351509618 ) ) ;
#14905 = FACE_OUTER_BOUND ( 'NONE', #7500, .T. ) ;
#14906 = ORIENTED_EDGE ( 'NONE', *, *, #5193, .F. ) ;
#14907 =( REPRESENTATION_RELATIONSHIP ('NONE','NONE', #23037, #15767 ) REPRESENTATION_RELATIONSHIP_WITH_TRANSFORMATION ( #7448 )SHAPE_REPRESENTATION_RELATIONSHIP( ) );
#14908 = DIRECTION ( 'NONE',  ( 1.000000000000000000, 0.000000000000000000, 0.000000000000000000 ) ) ;
#14909 = EDGE_LOOP ( 'NONE', ( #13736, #14530, #29265, #5929, #6794 ) ) ;
#14910 = DIRECTION ( 'NONE',  ( -0.4684084406997904848, -0.8835120444460226041, -0.000000000000000000 ) ) ;
#14911 = LINE ( 'NONE', #10077, #33590 ) ;
#14912 = VECTOR ( 'NONE', #7262, 1000.000000000000000 ) ;
#14914 = EDGE_LOOP ( 'NONE', ( #1111, #17602, #9069, #6959 ) ) ;
#14913 = AXIS2_PLACEMENT_3D ( 'NONE', #5459, #21664, #10988 ) ;
#14915 = AXIS2_PLACEMENT_3D ( 'NONE', #26657, #23815, #7252 ) ;
#14916 = DIRECTION ( 'NONE',  ( -0.000000000000000000, -0.000000000000000000, -1.000000000000000000 ) ) ;
#14917 = CARTESIAN_POINT ( 'NONE',  ( 0.02407890056655695096, 20.99477179376825120, 22.93149026599753526 ) ) ;
#14918 = AXIS2_PLACEMENT_3D ( 'NONE', #24330, #9358, #4939 ) ;
#14919 = EDGE_CURVE ( 'NONE', #34651, #19524, #26205, .T. ) ;
#14920 = VERTEX_POINT ( 'NONE', #34438 ) ;
#14921 = ADVANCED_FACE ( 'NONE', ( #12735 ), #12916, .F. ) ;
#14922 = DIRECTION ( 'NONE',  ( 0.1063910735369155841, -0.9943243633099125844, -3.335902418025060287E-15 ) ) ;
#14923 = CARTESIAN_POINT ( 'NONE',  ( -10.00000000000000000, 0.000000000000000000, 0.000000000000000000 ) ) ;
#14924 = ADVANCED_FACE ( 'NONE', ( #15577 ), #15063, .T. ) ;
#14925 = ORIENTED_EDGE ( 'NONE', *, *, #963, .F. ) ;
#14926 = CARTESIAN_POINT ( 'NONE',  ( -363.0000000000000000, 124.9999999999999432, 181.0000000000000000 ) ) ;
#14927 = CARTESIAN_POINT ( 'NONE',  ( 0.000000000000000000, 2.281310696040539424E-14, -36.68877005347592757 ) ) ;
#14928 = LINE ( 'NONE', #34120, #17925 ) ;
#14929 = CARTESIAN_POINT ( 'NONE',  ( -430.0000000000000000, 130.9999999999999716, 111.9999999999999858 ) ) ;
#14930 = VERTEX_POINT ( 'NONE', #2041 ) ;
#14931 = ORIENTED_EDGE ( 'NONE', *, *, #20714, .F. ) ;
#14932 = ORIENTED_EDGE ( 'NONE', *, *, #16893, .F. ) ;
#14933 = PRODUCT_DEFINITION_SHAPE ( 'NONE', 'NONE',  #21422 ) ;
#14934 = CLOSED_SHELL ( 'NONE', ( #459, #18211, #34663, #24891, #18979, #33868, #14233, #10043, #22463, #16450, #21768, #21738, #33073, #14968, #14731, #6704, #34226, #24929 ) ) ;
#14935 = CARTESIAN_POINT ( 'NONE',  ( 0.7561992069920354664, 27.74641878906462722, 19.50321439924967848 ) ) ;
#14936 = DIRECTION ( 'NONE',  ( -1.000000000000000000, -0.000000000000000000, -0.000000000000000000 ) ) ;
#14937 = CARTESIAN_POINT ( 'NONE',  ( -349.0000000000000000, 134.9999999999999716, 113.9999999999999858 ) ) ;
#14938 = CARTESIAN_POINT ( 'NONE',  ( 0.7181323043387224381, -1.866624223957557671, 0.000000000000000000 ) ) ;
#14939 = VECTOR ( 'NONE', #19149, 1000.000000000000114 ) ;
#14940 = AXIS2_PLACEMENT_3D ( 'NONE', #12374, #31567, #34421 ) ;
#14941 = CARTESIAN_POINT ( 'NONE',  ( 0.07094832566281392139, 19.10378521888243597, 25.28945800968172009 ) ) ;
#14942 = VECTOR ( 'NONE', #26259, 1000.000000000000000 ) ;
#14943 = CARTESIAN_POINT ( 'NONE',  ( -3.250000000000000000, 5.404196845913421754, 3.930000000000000160 ) ) ;
#14944 = EDGE_LOOP ( 'NONE', ( #29611, #32309, #34531, #27783 ) ) ;
#14945 = CARTESIAN_POINT ( 'NONE',  ( 101.4934480377529979, 4.557154561855115027, 11.64184170122662287 ) ) ;
#14946 = EDGE_LOOP ( 'NONE', ( #34225, #32974, #6907, #1682 ) ) ;
#14947 = CARTESIAN_POINT ( 'NONE',  ( 2.765921099433442887, -8.112136323389137260, 30.01377904834206589 ) ) ;
#14948 = LINE ( 'NONE', #28460, #723 ) ;
#14949 = VERTEX_POINT ( 'NONE', #23758 ) ;
#14950 = LINE ( 'NONE', #22953, #32273 ) ;
#14951 = CARTESIAN_POINT ( 'NONE',  ( -442.0000000000000000, -125.0000000000000000, 155.0000000000000000 ) ) ;
#14952 = DIRECTION ( 'NONE',  ( 0.000000000000000000, 0.000000000000000000, 1.000000000000000000 ) ) ;
#14953 = CARTESIAN_POINT ( 'NONE',  ( 0.1835381641992968882, -0.8174345826532598558, 32.26081300283360065 ) ) ;
#14954 = UNCERTAINTY_MEASURE_WITH_UNIT (LENGTH_MEASURE( 1.000000000000000082E-05 ), #11939, 'distance_accuracy_value', 'NONE');
#14955 = CARTESIAN_POINT ( 'NONE',  ( 143.0000000000000568, -78.33668825982579165, -63.00000000000000000 ) ) ;
#14956 = DIRECTION ( 'NONE',  ( -0.000000000000000000, 1.000000000000000000, -0.000000000000000000 ) ) ;
#14957 = ADVANCED_FACE ( 'NONE', ( #34615 ), #10225, .F. ) ;
#14958 = ORIENTED_EDGE ( 'NONE', *, *, #3698, .T. ) ;
#14959 = VERTEX_POINT ( 'NONE', #8251 ) ;
#14960 = CIRCLE ( 'NONE', #2988, 7.999999999999979572 ) ;
#14961 = AXIS2_PLACEMENT_3D ( 'NONE', #13548, #35087, #19075 ) ;
#14962 = DIRECTION ( 'NONE',  ( -7.893605728314050488E-14, 1.618803117314786135E-15, 0.9999999999999998890 ) ) ;
#14963 = AXIS2_PLACEMENT_3D ( 'NONE', #5022, #25880, #23730 ) ;
#14964 = ADVANCED_FACE ( 'NONE', ( #10762 ), #29971, .T. ) ;
#14965 = ORIENTED_EDGE ( 'NONE', *, *, #7247, .T. ) ;
#14966 = EDGE_CURVE ( 'NONE', #9840, #13324, #7769, .T. ) ;
#14967 = CARTESIAN_POINT ( 'NONE',  ( 27.64943126350854286, -17.16721653852534146, 68.31122994652405112 ) ) ;
#14968 = ADVANCED_FACE ( 'NONE', ( #18607 ), #29452, .T. ) ;
#14969 = DIRECTION ( 'NONE',  ( 0.1452892791026232089, 0.5232846903699686081, 0.8396809859716046764 ) ) ;
#14970 = ADVANCED_FACE ( 'NONE', ( #21437 ), #13782, .F. ) ;
#14971 = CONTEXT_DEPENDENT_SHAPE_REPRESENTATION ( #24183, #6659 ) ;
#14972 = VERTEX_POINT ( 'NONE', #21779 ) ;
#14973 = PLANE ( 'NONE',  #33250 ) ;
#14974 = FACE_OUTER_BOUND ( 'NONE', #12346, .T. ) ;
#14975 = ADVANCED_FACE ( 'NONE', ( #32280 ), #23913, .F. ) ;
#14976 =( GEOMETRIC_REPRESENTATION_CONTEXT ( 3 ) GLOBAL_UNCERTAINTY_ASSIGNED_CONTEXT ( ( #17148 ) ) GLOBAL_UNIT_ASSIGNED_CONTEXT ( ( #21935, #30293, #5894 ) ) REPRESENTATION_CONTEXT ( 'NONE', 'WORKASPACE' ) );
#14978 = LINE ( 'NONE', #561, #22088 ) ;
#14977 = DIRECTION ( 'NONE',  ( 1.000000000000000000, 0.000000000000000000, 0.000000000000000000 ) ) ;
#14979 = EDGE_LOOP ( 'NONE', ( #14537, #6623, #5546, #10724, #13900, #27893 ) ) ;
#14980 = ORIENTED_EDGE ( 'NONE', *, *, #9768, .T. ) ;
#14981 = DIRECTION ( 'NONE',  ( 1.000000000000000000, 0.000000000000000000, 0.000000000000000000 ) ) ;
#14982 = CARTESIAN_POINT ( 'NONE',  ( 12.00000000000001066, -32.99999999999997158, -175.0000000000000000 ) ) ;
#14983 = ORIENTED_EDGE ( 'NONE', *, *, #10937, .F. ) ;
#14984 = AXIS2_PLACEMENT_3D ( 'NONE', #17813, #33990, #26321 ) ;
#14985 = CARTESIAN_POINT ( 'NONE',  ( 2.789999999999999591, -21.14855567236443434, -22.20072382163073854 ) ) ;
#14986 = AXIS2_PLACEMENT_3D ( 'NONE', #22199, #25027, #10821 ) ;
#14987 = AXIS2_PLACEMENT_3D ( 'NONE', #12493, #2310, #21892 ) ;
#14988 = ORIENTED_EDGE ( 'NONE', *, *, #31444, .F. ) ;
#14989 = CARTESIAN_POINT ( 'NONE',  ( 22.89764159710613001, 4.274639749586560455, -77.50000000000000000 ) ) ;
#14990 = CARTESIAN_POINT ( 'NONE',  ( 12.00000000000003908, -60.99999999999996447, -154.9999999999999716 ) ) ;
#14991 = CYLINDRICAL_SURFACE ( 'NONE', #9860, 2.524999999999999467 ) ;
#14993 = CARTESIAN_POINT ( 'NONE',  ( 143.0000000000000568, -45.49999999999999289, 65.00000000000000000 ) ) ;
#14992 = CARTESIAN_POINT ( 'NONE',  ( -144.4704739938196099, -45.49999999999999289, 63.00000000000000000 ) ) ;
#14994 = LINE ( 'NONE', #22296, #20686 ) ;
#14995 = DIRECTION ( 'NONE',  ( 0.000000000000000000, 0.000000000000000000, 1.000000000000000000 ) ) ;
#14996 = ORIENTED_EDGE ( 'NONE', *, *, #29727, .F. ) ;
#14997 = CARTESIAN_POINT ( 'NONE',  ( 2.033800785921083154, -9.974544214302445866, -32.41523709743442083 ) ) ;
#14998 = CARTESIAN_POINT ( 'NONE',  ( 0.02407890056655695096, -26.45933846664182099, -16.32596387352474565 ) ) ;
#14999 = ORIENTED_EDGE ( 'NONE', *, *, #6923, .F. ) ;
#15000 = ORIENTED_EDGE ( 'NONE', *, *, #15125, .F. ) ;
#15001 = ORIENTED_EDGE ( 'NONE', *, *, #8238, .T. ) ;
#15002 = ADVANCED_FACE ( 'NONE', ( #2555 ), #30139, .F. ) ;
#15003 = AXIS2_PLACEMENT_3D ( 'NONE', #26454, #15620, #29313 ) ;
#15004 = VECTOR ( 'NONE', #14343, 1000.000000000000000 ) ;
#15005 = EDGE_CURVE ( 'NONE', #8559, #3111, #11431, .T. ) ;
#15006 = DIRECTION ( 'NONE',  ( -0.000000000000000000, -0.000000000000000000, -1.000000000000000000 ) ) ;
#15007 = ADVANCED_FACE ( 'NONE', ( #29794 ), #5046, .T. ) ;
#15008 = AXIS2_PLACEMENT_3D ( 'NONE', #1105, #23687, #15338 ) ;
#15009 = EDGE_LOOP ( 'NONE', ( #722, #8253, #1591, #20967 ) ) ;
#15010 = ORIENTED_EDGE ( 'NONE', *, *, #30694, .T. ) ;
#15011 = VERTEX_POINT ( 'NONE', #5399 ) ;
#15012 = CARTESIAN_POINT ( 'NONE',  ( -20.00000000000004619, -105.0000000000000000, -162.9999999999999716 ) ) ;
#15013 = ORIENTED_EDGE ( 'NONE', *, *, #8634, .T. ) ;
#15014 = CARTESIAN_POINT ( 'NONE',  ( -430.0000000000000000, -131.0000000000000000, 128.0000000000000000 ) ) ;
#15015 = CARTESIAN_POINT ( 'NONE',  ( -410.0000000000000568, -105.0000000000000142, 107.9999999999999574 ) ) ;
#15016 = ORIENTED_EDGE ( 'NONE', *, *, #30130, .F. ) ;
#15017 = ORIENTED_EDGE ( 'NONE', *, *, #11136, .F. ) ;
#15018 = CARTESIAN_POINT ( 'NONE',  ( 12.46788440507149787, 30.06253867087536946, 49.43553178847298568 ) ) ;
#15019 = CARTESIAN_POINT ( 'NONE',  ( -0.9727285265192158192, -1.747512292859697114, 4.679999999999999716 ) ) ;
#15020 = LINE ( 'NONE', #14851, #34642 ) ;
#15022 = EDGE_CURVE ( 'NONE', #8951, #19693, #32806, .T. ) ;
#15021 = LINE ( 'NONE', #28190, #32436 ) ;
#15023 = CARTESIAN_POINT ( 'NONE',  ( -418.0000000000000000, 137.0000000000000000, 154.9999999999999716 ) ) ;
#15024 = ORIENTED_EDGE ( 'NONE', *, *, #4157, .F. ) ;
#15025 = DIRECTION ( 'NONE',  ( 1.000000000000000000, 0.000000000000000000, 0.000000000000000000 ) ) ;
#15026 = CARTESIAN_POINT ( 'NONE',  ( -499.9999999999999432, 112.9999999999999574, 159.0000000000000000 ) ) ;
#15027 = VECTOR ( 'NONE', #30545, 1000.000000000000000 ) ;
#15028 = DIRECTION ( 'NONE',  ( 0.000000000000000000, 1.000000000000000000, 0.000000000000000000 ) ) ;
#15029 = ORIENTED_EDGE ( 'NONE', *, *, #6086, .F. ) ;
#15030 = VECTOR ( 'NONE', #30809, 1000.000000000000000 ) ;
#15031 = CARTESIAN_POINT ( 'NONE',  ( 0.7561992264529545649, -32.71371797491577382, 8.947166372574571369 ) ) ;
#15033 = EDGE_CURVE ( 'NONE', #7332, #27667, #10284, .T. ) ;
#15032 = CARTESIAN_POINT ( 'NONE',  ( 0.000000000000000000, 2.281450406192313828E-14, -36.69637551990492597 ) ) ;
#15034 = PLANE ( 'NONE',  #13270 ) ;
#15035 = ADVANCED_FACE ( 'NONE', ( #27119, #2734 ), #24432, .T. ) ;
#15036 = DIRECTION ( 'NONE',  ( 0.000000000000000000, 1.310824597558155437E-49, 1.000000000000000000 ) ) ;
#15037 = CARTESIAN_POINT ( 'NONE',  ( -349.0000000000000000, -125.0000000000000284, 164.9999999999999716 ) ) ;
#15039 = CARTESIAN_POINT ( 'NONE',  ( -105.8665330455879143, 5.043966910541457516, -5.550724164612919509 ) ) ;
#15038 = LINE ( 'NONE', #1836, #8199 ) ;
#15040 = EDGE_CURVE ( 'NONE', #30310, #10803, #5737, .T. ) ;
#15041 = AXIS2_PLACEMENT_3D ( 'NONE', #4062, #15653, #20459 ) ;
#15042 = DIRECTION ( 'NONE',  ( 1.000000000000000000, 0.000000000000000000, 0.000000000000000000 ) ) ;
#15043 = ORIENTED_EDGE ( 'NONE', *, *, #817, .F. ) ;
#15044 = DIRECTION ( 'NONE',  ( -1.000000000000000000, 0.000000000000000000, 0.000000000000000000 ) ) ;
#15046 = CARTESIAN_POINT ( 'NONE',  ( 0.1859802928572567293, -3.229344000442754048, 32.11979559073828483 ) ) ;
#15045 = LINE ( 'NONE', #4666, #25715 ) ;
#15047 = VECTOR ( 'NONE', #20992, 1000.000000000000000 ) ;
#15048 = EDGE_CURVE ( 'NONE', #34687, #9057, #34160, .T. ) ;
#15049 = EDGE_LOOP ( 'NONE', ( #26845, #16334, #1948, #24745 ) ) ;
#15050 = DIRECTION ( 'NONE',  ( -0.000000000000000000, -0.000000000000000000, -1.000000000000000000 ) ) ;
#15051 = ORIENTED_EDGE ( 'NONE', *, *, #34559, .T. ) ;
#15052 = VECTOR ( 'NONE', #29966, 1000.000000000000000 ) ;
#15053 = EDGE_CURVE ( 'NONE', #21780, #12730, #3464, .T. ) ;
#15054 = VERTEX_POINT ( 'NONE', #34973 ) ;
#15055 = CARTESIAN_POINT ( 'NONE',  ( 103.4525503535520414, -5.538930788889586232, -5.058095442343715220 ) ) ;
#15056 = VERTEX_POINT ( 'NONE', #10590 ) ;
#15057 = ORIENTED_EDGE ( 'NONE', *, *, #4882, .T. ) ;
#15058 = CARTESIAN_POINT ( 'NONE',  ( 1.749999999999999778, 0.000000000000000000, 0.000000000000000000 ) ) ;
#15059 = AXIS2_PLACEMENT_3D ( 'NONE', #24357, #13004, #21694 ) ;
#15060 = CARTESIAN_POINT ( 'NONE',  ( -430.0000000000000000, 130.9999999999999716, 113.9999999999999858 ) ) ;
#15061 = AXIS2_PLACEMENT_3D ( 'NONE', #26051, #18234, #1665 ) ;
#15062 = CARTESIAN_POINT ( 'NONE',  ( -20.63749999999999574, 1.809415645740214338E-15, 14.77500000000000036 ) ) ;
#15063 = PLANE ( 'NONE',  #9725 ) ;
#15064 = EDGE_LOOP ( 'NONE', ( #24218, #33058, #24887, #1577 ) ) ;
#15065 = ORIENTED_EDGE ( 'NONE', *, *, #28202, .T. ) ;
#15066 = VECTOR ( 'NONE', #17676, 1000.000000000000114 ) ;
#15067 = CARTESIAN_POINT ( 'NONE',  ( 2.789999999999999147, 27.98916443103621177, -12.86217335695007868 ) ) ;
#15068 = CARTESIAN_POINT ( 'NONE',  ( -35.55956070192387841, -17.65143121711728469, 10.00000000000000000 ) ) ;
#15069 = PLANE ( 'NONE',  #13522 ) ;
#15070 = CARTESIAN_POINT ( 'NONE',  ( 19.99999999999998934, -55.00000000000000711, 162.9999999999999716 ) ) ;
#15071 = CARTESIAN_POINT ( 'NONE',  ( 1.039999999999999591, 31.89769921722987434, 12.91988538846969803 ) ) ;
#15072 = ORIENTED_EDGE ( 'NONE', *, *, #12125, .F. ) ;
#15073 = LINE ( 'NONE', #12926, #9044 ) ;
#15074 = VERTEX_POINT ( 'NONE', #8777 ) ;
#15075 = CARTESIAN_POINT ( 'NONE',  ( 0.5288002586553935958, 33.02096244749627374, 4.949265406682166635 ) ) ;
#15076 = LINE ( 'NONE', #28243, #9205 ) ;
#15077 = EDGE_CURVE ( 'NONE', #3477, #28571, #25144, .T. ) ;
#15078 = DIRECTION ( 'NONE',  ( 0.000000000000000000, 0.000000000000000000, 1.000000000000000000 ) ) ;
#15079 = ORIENTED_EDGE ( 'NONE', *, *, #15807, .T. ) ;
#15080 = EDGE_CURVE ( 'NONE', #1337, #17462, #12006, .T. ) ;
#15081 = AXIS2_PLACEMENT_3D ( 'NONE', #15142, #33645, #3563 ) ;
#15082 = DIRECTION ( 'NONE',  ( -0.000000000000000000, 1.000000000000000000, -0.000000000000000000 ) ) ;
#15083 = ORIENTED_EDGE ( 'NONE', *, *, #20395, .F. ) ;
#15085 = DIRECTION ( 'NONE',  ( 0.000000000000000000, 2.309213040847544338E-50, 1.000000000000000000 ) ) ;
#15084 = FACE_OUTER_BOUND ( 'NONE', #14979, .T. ) ;
#15086 = AXIS2_PLACEMENT_3D ( 'NONE', #14937, #25771, #9229 ) ;
#15087 = CARTESIAN_POINT ( 'NONE',  ( -109.9476871814112684, 1.341502966352549508, 12.43231302123709625 ) ) ;
#15088 = AXIS2_PLACEMENT_3D ( 'NONE', #21190, #23688, #26527 ) ;
#15089 = VERTEX_POINT ( 'NONE', #30678 ) ;
#15090 = AXIS2_PLACEMENT_3D ( 'NONE', #10869, #13547, #16407 ) ;
#15091 = DIRECTION ( 'NONE',  ( 0.000000000000000000, -1.000000000000000000, 0.000000000000000000 ) ) ;
#15092 = DIRECTION ( 'NONE',  ( 0.000000000000000000, -0.000000000000000000, 1.000000000000000000 ) ) ;
#15093 = ORIENTED_EDGE ( 'NONE', *, *, #18470, .F. ) ;
#15094 = DIRECTION ( 'NONE',  ( -0.1063910735369225230, 0.9943243633099118073, -1.000770725407345128E-14 ) ) ;
#15095 = CARTESIAN_POINT ( 'NONE',  ( 100.8159517847998075, -3.931125184197652445, 11.86656790805995243 ) ) ;
#15096 = ORIENTED_EDGE ( 'NONE', *, *, #6338, .T. ) ;
#15097 = CARTESIAN_POINT ( 'NONE',  ( -414.0000000000000568, -112.9999999999999858, 155.0000000000000000 ) ) ;
#15098 = CARTESIAN_POINT ( 'NONE',  ( -11.99999999999998224, -134.9999999999999716, 162.9999999999999716 ) ) ;
#15099 = CIRCLE ( 'NONE', #29319, 3.999999999999976019 ) ;
#15100 = B_SPLINE_CURVE_WITH_KNOTS ( 'NONE', 3,
 ( #7918, #2572, #21793, #8270 ),
 .UNSPECIFIED., .F., .F.,
 ( 4, 4 ),
 ( 0.005298352430873754307, 0.005985221104152186646 ),
 .UNSPECIFIED. ) ;
#15101 = CARTESIAN_POINT ( 'NONE',  ( 1.039999999999999813, -30.02688531850407117, 16.81585001935569323 ) ) ;
#15102 = CARTESIAN_POINT ( 'NONE',  ( 19.99999999999998224, 134.9999999999998863, 187.0000000000000000 ) ) ;
#15103 = VERTEX_POINT ( 'NONE', #16824 ) ;
#15104 = EDGE_LOOP ( 'NONE', ( #14307, #23131, #14245, #27576 ) ) ;
#15105 = EDGE_LOOP ( 'NONE', ( #16076, #8245, #6526, #11588, #13884, #967, #18844, #26370 ) ) ;
#15106 = VECTOR ( 'NONE', #33707, 1000.000000000000000 ) ;
#15107 = EDGE_CURVE ( 'NONE', #12737, #22067, #3429, .T. ) ;
#15108 = DIRECTION ( 'NONE',  ( 0.000000000000000000, 1.836970198721029441E-16, -1.000000000000000000 ) ) ;
#15109 = CIRCLE ( 'NONE', #5979, 7.999999999999979572 ) ;
#15110 = CARTESIAN_POINT ( 'NONE',  ( -349.0000000000000000, -135.0000000000000000, 130.0000000000000000 ) ) ;
#15111 = DIRECTION ( 'NONE',  ( -0.05413890858541543089, -0.9985334138511240409, -0.000000000000000000 ) ) ;
#15112 = CARTESIAN_POINT ( 'NONE',  ( -20.00000000000007461, 112.9999999999999574, 187.0000000000000000 ) ) ;
#15114 = FACE_OUTER_BOUND ( 'NONE', #29294, .T. ) ;
#15113 =( REPRESENTATION_RELATIONSHIP ('NONE','NONE', #23037, #30518 ) REPRESENTATION_RELATIONSHIP_WITH_TRANSFORMATION ( #25805 )SHAPE_REPRESENTATION_RELATIONSHIP( ) );
#15115 = DIRECTION ( 'NONE',  ( -1.000000000000000000, -0.000000000000000000, -0.000000000000000000 ) ) ;
#15116 = ORIENTED_EDGE ( 'NONE', *, *, #20040, .F. ) ;
#15117 = VECTOR ( 'NONE', #6781, 1000.000000000000000 ) ;
#15118 = ADVANCED_FACE ( 'NONE', ( #6629, #17529, #31032 ), #430, .F. ) ;
#15119 = DIRECTION ( 'NONE',  ( -1.000000000000000000, -0.000000000000000000, -0.000000000000000000 ) ) ;
#15120 = EDGE_CURVE ( 'NONE', #12035, #2425, #15432, .T. ) ;
#15121 = VERTEX_POINT ( 'NONE', #28361 ) ;
#15122 = EDGE_CURVE ( 'NONE', #29489, #11417, #6449, .T. ) ;
#15123 = CARTESIAN_POINT ( 'NONE',  ( -418.0000000000000000, -105.0000000000000142, -101.9999999999999858 ) ) ;
#15124 = EDGE_LOOP ( 'NONE', ( #33335, #15349, #24122, #6485 ) ) ;
#15125 = EDGE_CURVE ( 'NONE', #29665, #22708, #8574, .T. ) ;
#15126 = PLANE ( 'NONE',  #21150 ) ;
#15127 = CARTESIAN_POINT ( 'NONE',  ( -45.05956070192387841, -20.15143121711730245, 20.00000000000000000 ) ) ;
#15128 = CIRCLE ( 'NONE', #32737, 2.033421858999710619 ) ;
#15129 = CARTESIAN_POINT ( 'NONE',  ( 0.006892386950099134262, -26.23471115434894685, 16.26912442529598835 ) ) ;
#15130 = DIRECTION ( 'NONE',  ( -0.000000000000000000, 1.000000000000000000, -0.000000000000000000 ) ) ;
#15131 = FILL_AREA_STYLE_COLOUR ( '', #4624 ) ;
#15132 = VECTOR ( 'NONE', #28544, 1000.000000000000000 ) ;
#15133 = ORIENTED_EDGE ( 'NONE', *, *, #24986, .T. ) ;
#15134 = VERTEX_POINT ( 'NONE', #19660 ) ;
#15135 = CARTESIAN_POINT ( 'NONE',  ( 808.9261511794453554, 963.3580553244713656, 1753.598338701302509 ) ) ;
#15136 = ORIENTED_EDGE ( 'NONE', *, *, #19165, .T. ) ;
#15137 = CIRCLE ( 'NONE', #28771, 2.525000000000001688 ) ;
#15138 = CARTESIAN_POINT ( 'NONE',  ( 1.532562817202168137, 37.83772838912469894, 68.31122994652405112 ) ) ;
#15139 = CARTESIAN_POINT ( 'NONE',  ( 2.765921099433441555, 24.20451283648857554, -19.51346322004903300 ) ) ;
#15140 = CONTEXT_DEPENDENT_SHAPE_REPRESENTATION ( #31006, #12378 ) ;
#15141 = VERTEX_POINT ( 'NONE', #8600 ) ;
#15142 = CARTESIAN_POINT ( 'NONE',  ( 11.99999999999999645, 124.9999999999999716, 190.9999999999999716 ) ) ;
#15143 = DIRECTION ( 'NONE',  ( -1.000000000000000000, -0.000000000000000000, -0.000000000000000000 ) ) ;
#15144 = ITEM_DEFINED_TRANSFORMATION ( 'NONE', 'NONE', #31478,  #28566 ) ;
#15145 = CIRCLE ( 'NONE', #16863, 2.033421858999711951 ) ;
#15147 = DIRECTION ( 'NONE',  ( 1.000000000000000000, 0.000000000000000000, 1.300283923313630633E-47 ) ) ;
#15146 = CARTESIAN_POINT ( 'NONE',  ( -499.9999999999999432, -113.0000000000000000, -190.9999999999999716 ) ) ;
#15148 = VERTEX_POINT ( 'NONE', #13962 ) ;
#15149 = EDGE_LOOP ( 'NONE', ( #31945, #30896, #8639, #10064 ) ) ;
#15150 = DIRECTION ( 'NONE',  ( 1.000000000000000000, 0.000000000000000000, 0.000000000000000000 ) ) ;
#15151 = ADVANCED_FACE ( 'NONE', ( #3263 ), #28182, .F. ) ;
#15152 = AXIS2_PLACEMENT_3D ( 'NONE', #33128, #22284, #8568 ) ;
#15153 = EDGE_CURVE ( 'NONE', #11831, #15331, #24968, .T. ) ;
#15154 = DIRECTION ( 'NONE',  ( 1.000000000000000000, 0.000000000000000000, 0.000000000000000000 ) ) ;
#15155 = PLANE ( 'NONE',  #3475 ) ;
#15156 = VERTEX_POINT ( 'NONE', #14318 ) ;
#15157 = LINE ( 'NONE', #12661, #7188 ) ;
#15158 = EDGE_CURVE ( 'NONE', #34740, #4151, #596, .T. ) ;
#15159 = B_SPLINE_CURVE_WITH_KNOTS ( 'NONE', 3,
 ( #20790, #7244, #31984, #15459 ),
 .UNSPECIFIED., .F., .F.,
 ( 4, 4 ),
 ( 2.876507994514687179E-07, 0.0006880240977454715181 ),
 .UNSPECIFIED. ) ;
#15160 = ORIENTED_EDGE ( 'NONE', *, *, #27574, .F. ) ;
#15161 = EDGE_CURVE ( 'NONE', #763, #25411, #33513, .T. ) ;
#15162 = AXIS2_PLACEMENT_3D ( 'NONE', #32267, #21761, #3066 ) ;
#15163 = LINE ( 'NONE', #27972, #428 ) ;
#15164 = LINE ( 'NONE', #12845, #14306 ) ;
#15165 = DIRECTION ( 'NONE',  ( 0.000000000000000000, -1.000000000000000000, 0.000000000000000000 ) ) ;
#15167 = DIRECTION ( 'NONE',  ( -1.000000000000000000, 0.000000000000000000, 0.000000000000000000 ) ) ;
#15166 = LINE ( 'NONE', #20327, #848 ) ;
#15168 = CARTESIAN_POINT ( 'NONE',  ( 2.789999999999999147, -25.77598557799237255, -16.24962337825830616 ) ) ;
#15169 = CARTESIAN_POINT ( 'NONE',  ( 143.0000000000000568, -78.33668825982579165, -75.00000000000001421 ) ) ;
#15170 = LINE ( 'NONE', #7129, #33210 ) ;
#15171 = DIRECTION ( 'NONE',  ( 1.000000000000000000, 0.000000000000000000, 0.000000000000000000 ) ) ;
#15172 = PRODUCT_DEFINITION_SHAPE ( 'NONE', 'NONE',  #35161 ) ;
#15173 = AXIS2_PLACEMENT_3D ( 'NONE', #25470, #19449, #27792 ) ;
#15174 = EDGE_CURVE ( 'NONE', #18838, #14780, #17351, .T. ) ;
#15175 = ADVANCED_FACE ( 'NONE', ( #8963 ), #6268, .T. ) ;
#15176 = VECTOR ( 'NONE', #7456, 1000.000000000000000 ) ;
#15177 = ORIENTED_EDGE ( 'NONE', *, *, #29976, .T. ) ;
#15178 = ORIENTED_EDGE ( 'NONE', *, *, #12306, .T. ) ;
#15179 = ORIENTED_EDGE ( 'NONE', *, *, #679, .F. ) ;
#15180 = CARTESIAN_POINT ( 'NONE',  ( 2.765921099433441999, -21.56796757982826307, 22.39322359481599278 ) ) ;
#15181 = EDGE_LOOP ( 'NONE', ( #11171, #10677, #27068, #2424 ) ) ;
#15182 = ORIENTED_EDGE ( 'NONE', *, *, #15886, .T. ) ;
#15183 = ORIENTED_EDGE ( 'NONE', *, *, #2757, .T. ) ;
#15184 = DIRECTION ( 'NONE',  ( 0.000000000000000000, 0.000000000000000000, -1.000000000000000000 ) ) ;
#15185 = ORIENTED_EDGE ( 'NONE', *, *, #1439, .T. ) ;
#15186 = CARTESIAN_POINT ( 'NONE',  ( -442.0000000000000000, -105.0000000000000142, -101.9999999999999858 ) ) ;
#15187 = LINE ( 'NONE', #31877, #16017 ) ;
#15188 = ORIENTED_EDGE ( 'NONE', *, *, #27429, .T. ) ;
#15189 = ORIENTED_EDGE ( 'NONE', *, *, #17735, .F. ) ;
#15190 = DIRECTION ( 'NONE',  ( 0.000000000000000000, -1.000000000000000000, 0.000000000000000000 ) ) ;
#15191 = DIRECTION ( 'NONE',  ( 0.000000000000000000, 0.000000000000000000, 1.000000000000000000 ) ) ;
#15192 = CIRCLE ( 'NONE', #10643, 1.999999999999999556 ) ;
#15193 = CARTESIAN_POINT ( 'NONE',  ( -445.9999999999999432, 137.0000000000000000, 154.9999999999999716 ) ) ;
#15194 = DIRECTION ( 'NONE',  ( -0.000000000000000000, -0.000000000000000000, -1.000000000000000000 ) ) ;
#15195 = FACE_OUTER_BOUND ( 'NONE', #12620, .T. ) ;
#15196 = ORIENTED_EDGE ( 'NONE', *, *, #8382, .F. ) ;
#15198 = DIRECTION ( 'NONE',  ( -1.000000000000000000, -0.000000000000000000, -0.000000000000000000 ) ) ;
#15197 = VECTOR ( 'NONE', #2006, 1000.000000000000000 ) ;
#15199 = FACE_OUTER_BOUND ( 'NONE', #10019, .T. ) ;
#15200 = CARTESIAN_POINT ( 'NONE',  ( -449.9999999999999432, 124.9999999999999432, -162.9999999999999716 ) ) ;
#15201 = ORIENTED_EDGE ( 'NONE', *, *, #657, .T. ) ;
#15202 = CARTESIAN_POINT ( 'NONE',  ( 36.86854689046325717, 8.645963718612074800, 68.31122994652405112 ) ) ;
#15203 = DIRECTION ( 'NONE',  ( -1.000000000000000000, -0.000000000000000000, -0.000000000000000000 ) ) ;
#15204 = CARTESIAN_POINT ( 'NONE',  ( -430.0000000000000000, 118.9999999999999858, 128.0000000000000000 ) ) ;
#15205 = ADVANCED_FACE ( 'NONE', ( #14496 ), #3786, .F. ) ;
#15206 = DIRECTION ( 'NONE',  ( 0.000000000000000000, 0.000000000000000000, 1.000000000000000000 ) ) ;
#15207 = VECTOR ( 'NONE', #30725, 1000.000000000000000 ) ;
#15209 = CARTESIAN_POINT ( 'NONE',  ( -102.8541734989807424, 4.646131333787439921, -5.888157618374222579 ) ) ;
#15208 = CARTESIAN_POINT ( 'NONE',  ( -1.120881116509116332E-15, 14.57887998322625300, 26.97387222978633403 ) ) ;
#15210 = ADVANCED_BREP_SHAPE_REPRESENTATION ( '', ( #33646, #28566 ), #29141 ) ;
#15211 = EDGE_CURVE ( 'NONE', #5830, #10504, #23470, .T. ) ;
#15212 = ADVANCED_FACE ( 'NONE', ( #9129 ), #23710, .T. ) ;
#15213 = AXIS2_PLACEMENT_3D ( 'NONE', #22181, #296, #19522 ) ;
#15214 = CARTESIAN_POINT ( 'NONE',  ( -499.9999999999999432, 108.9999999999999858, 162.9999999999999716 ) ) ;
#15215 = ORIENTED_EDGE ( 'NONE', *, *, #11720, .F. ) ;
#15216 = CARTESIAN_POINT ( 'NONE',  ( 101.4948815640033928, 4.558408617645864247, -11.64136836827557708 ) ) ;
#15218 = DIRECTION ( 'NONE',  ( 0.000000000000000000, 0.000000000000000000, -1.000000000000000000 ) ) ;
#15217 = DIRECTION ( 'NONE',  ( 0.000000000000000000, 0.000000000000000000, -1.000000000000000000 ) ) ;
#15219 = VECTOR ( 'NONE', #15240, 1000.000000000000114 ) ;
#15220 = ORIENTED_EDGE ( 'NONE', *, *, #6212, .F. ) ;
#15221 = PRODUCT_DEFINITION_SHAPE ( 'NONE', 'NONE',  #35118 ) ;
#15222 = DIRECTION ( 'NONE',  ( -2.154935995002245207E-17, -0.000000000000000000, -1.000000000000000000 ) ) ;
#15223 = ORIENTED_EDGE ( 'NONE', *, *, #10888, .F. ) ;
#15224 = EDGE_CURVE ( 'NONE', #32413, #1937, #26194, .T. ) ;
#15225 = VECTOR ( 'NONE', #25109, 1000.000000000000114 ) ;
#15226 = VECTOR ( 'NONE', #22776, 1000.000000000000000 ) ;
#15227 = ORIENTED_EDGE ( 'NONE', *, *, #963, .T. ) ;
#15228 = DIRECTION ( 'NONE',  ( -1.000000000000000000, -0.000000000000000000, -0.000000000000000000 ) ) ;
#15229 = ORIENTED_EDGE ( 'NONE', *, *, #23966, .T. ) ;
#15230 = ORIENTED_EDGE ( 'NONE', *, *, #31529, .F. ) ;
#15231 = CARTESIAN_POINT ( 'NONE',  ( 1.532562817202168137, 37.83772838912472025, -36.68877005347593467 ) ) ;
#15232 = AXIS2_PLACEMENT_3D ( 'NONE', #22144, #19308, #13787 ) ;
#15233 = EDGE_CURVE ( 'NONE', #33936, #17530, #3493, .T. ) ;
#15235 = EDGE_CURVE ( 'NONE', #23630, #5569, #15187, .T. ) ;
#15234 = LINE ( 'NONE', #32279, #23615 ) ;
#15236 = DIRECTION ( 'NONE',  ( 0.6051742151937656855, -0.7960930657056433102, -1.462399237109729307E-16 ) ) ;
#15237 = ORIENTED_EDGE ( 'NONE', *, *, #12805, .T. ) ;
#15238 = ORIENTED_EDGE ( 'NONE', *, *, #18413, .F. ) ;
#15239 = DIRECTION ( 'NONE',  ( 1.000000000000000000, 0.000000000000000000, 0.000000000000000000 ) ) ;
#15240 = DIRECTION ( 'NONE',  ( 0.1617819965527638459, 0.9868265225415262520, -0.000000000000000000 ) ) ;
#15241 = DIRECTION ( 'NONE',  ( -0.000000000000000000, -1.000000000000000000, -0.000000000000000000 ) ) ;
#15242 = DIRECTION ( 'NONE',  ( -0.000000000000000000, -1.000000000000000000, -0.000000000000000000 ) ) ;
#15243 = DIRECTION ( 'NONE',  ( -0.000000000000000000, -5.053935297177146739E-49, -1.000000000000000000 ) ) ;
#15244 = ORIENTED_EDGE ( 'NONE', *, *, #29080, .F. ) ;
#15245 = CARTESIAN_POINT ( 'NONE',  ( -45.05956070192387841, -32.65143121711728469, 20.00000000000000000 ) ) ;
#15246 = AXIS2_PLACEMENT_3D ( 'NONE', #34744, #10355, #1995 ) ;
#15247 = CARTESIAN_POINT ( 'NONE',  ( -21.17270648470164218, -7.613573412837966181, 20.00000000000000000 ) ) ;
#15248 = ORIENTED_EDGE ( 'NONE', *, *, #4516, .T. ) ;
#15249 = CARTESIAN_POINT ( 'NONE',  ( -349.0000000000000000, 134.9999999999999716, 126.0000000000000000 ) ) ;
#15250 = CARTESIAN_POINT ( 'NONE',  ( -12.00000000000001066, -32.99999999999997158, 154.9999999999999716 ) ) ;
#15251 = CARTESIAN_POINT ( 'NONE',  ( -0.9727285265192158192, -1.747512292859697114, 3.930000000000000160 ) ) ;
#15252 = ORIENTED_EDGE ( 'NONE', *, *, #17596, .T. ) ;
#15253 = CIRCLE ( 'NONE', #18658, 4.750000000000004441 ) ;
#15254 = VECTOR ( 'NONE', #550, 1000.000000000000000 ) ;
#15255 = EDGE_CURVE ( 'NONE', #7431, #30469, #15363, .T. ) ;
#15256 = EDGE_CURVE ( 'NONE', #28359, #29908, #14162, .T. ) ;
#15257 = CARTESIAN_POINT ( 'NONE',  ( 23.93847777447632552, 22.04889236939138897, 68.31122994652405112 ) ) ;
#15258 = ORIENTED_EDGE ( 'NONE', *, *, #7445, .T. ) ;
#15260 = DIRECTION ( 'NONE',  ( 0.000000000000000000, 1.000000000000000000, 0.000000000000000000 ) ) ;
#15259 = DIRECTION ( 'NONE',  ( 1.000000000000000000, 0.000000000000000000, -0.000000000000000000 ) ) ;
#15261 = CARTESIAN_POINT ( 'NONE',  ( -109.3398582488967890, 2.712336548677834802, 12.20300697856196059 ) ) ;
#15262 = ADVANCED_FACE ( 'NONE', ( #28701, #9494 ), #20865, .T. ) ;
#15263 = AXIS2_PLACEMENT_3D ( 'NONE', #9235, #6377, #212 ) ;
#15264 = ORIENTED_EDGE ( 'NONE', *, *, #13623, .T. ) ;
#15265 = CARTESIAN_POINT ( 'NONE',  ( -25.63124651156763179, 20.05601094782695526, -36.68877005347593467 ) ) ;
#15266 = CARTESIAN_POINT ( 'NONE',  ( 15.99999999999998579, -32.99999999999997158, 154.9999999999999716 ) ) ;
#15267 = ORIENTED_EDGE ( 'NONE', *, *, #2834, .F. ) ;
#15268 = AXIS2_PLACEMENT_3D ( 'NONE', #1434, #31668, #23159 ) ;
#15269 = DIRECTION ( 'NONE',  ( 1.577811242015195894E-14, -3.106538118691702481E-14, 1.000000000000000000 ) ) ;
#15270 = ORIENTED_EDGE ( 'NONE', *, *, #21845, .T. ) ;
#15271 = CARTESIAN_POINT ( 'NONE',  ( 102.1097078945684444, -4.970825052104117070, 11.47130252761374614 ) ) ;
#15272 = ORIENTED_EDGE ( 'NONE', *, *, #13144, .F. ) ;
#15273 = CARTESIAN_POINT ( 'NONE',  ( -34.66645501699844090, -15.21971901163155216, 68.31122994652405112 ) ) ;
#15274 = ADVANCED_FACE ( 'NONE', ( #29042, #23357, #18389 ), #3953, .F. ) ;
#15275 = CARTESIAN_POINT ( 'NONE',  ( 129.3530333899765594, -6.000000000000000000, 57.49999999999999289 ) ) ;
#15277 = ADVANCED_FACE ( 'NONE', ( #20517 ), #20697, .T. ) ;
#15276 = B_SPLINE_CURVE_WITH_KNOTS ( 'NONE', 3,
 ( #9989, #31012, #23515, #9477, #31350, #14998 ),
 .UNSPECIFIED., .F., .F.,
 ( 4, 2, 4 ),
 ( 4.404817019028824490E-07, 0.001874269618538360743, 0.003748098755374818306 ),
 .UNSPECIFIED. ) ;
#15278 = CARTESIAN_POINT ( 'NONE',  ( 0.07098932382052611234, -27.07245655034587628, 16.48110659958382129 ) ) ;
#15279 = DIRECTION ( 'NONE',  ( 0.000000000000000000, -1.310824597558155437E-49, -1.000000000000000000 ) ) ;
#15280 = CONTEXT_DEPENDENT_SHAPE_REPRESENTATION ( #1479, #17455 ) ;
#15281 = ORIENTED_EDGE ( 'NONE', *, *, #11001, .F. ) ;
#15282 = ORIENTED_EDGE ( 'NONE', *, *, #3948, .T. ) ;
#15283 = VECTOR ( 'NONE', #20476, 1000.000000000000000 ) ;
#15284 = PRODUCT_DEFINITION_SHAPE ( 'NONE', 'NONE',  #35244 ) ;
#15285 = ORIENTED_EDGE ( 'NONE', *, *, #33301, .T. ) ;
#15286 = CARTESIAN_POINT ( 'NONE',  ( 8.000000000000000000, 0.000000000000000000, 0.000000000000000000 ) ) ;
#15287 = EDGE_CURVE ( 'NONE', #22184, #4601, #10899, .T. ) ;
#15288 = DIRECTION ( 'NONE',  ( 3.697785493223492838E-32, 1.934419779023891545E-16, -1.000000000000000000 ) ) ;
#15290 = ADVANCED_FACE ( 'NONE', ( #31202 ), #12695, .T. ) ;
#15289 = CARTESIAN_POINT ( 'NONE',  ( 2.765921099433444219, 31.00221527374952046, 2.344426712874309260 ) ) ;
#15291 = LINE ( 'NONE', #4560, #34202 ) ;
#15292 = B_SPLINE_CURVE_WITH_KNOTS ( 'NONE', 3,
 ( #8892, #30785, #17630, #14781 ),
 .UNSPECIFIED., .F., .F.,
 ( 4, 4 ),
 ( 1.979774382698227165E-07, 0.0006879336733830483793 ),
 .UNSPECIFIED. ) ;
#15293 = CARTESIAN_POINT ( 'NONE',  ( 145.0000000000000568, -87.50000000000000000, 51.88904920397797582 ) ) ;
#15294 = ORIENTED_EDGE ( 'NONE', *, *, #11270, .T. ) ;
#15295 = EDGE_CURVE ( 'NONE', #16028, #29353, #31888, .T. ) ;
#15296 = DIRECTION ( 'NONE',  ( 1.000000000000000000, 0.000000000000000000, -0.000000000000000000 ) ) ;
#15297 = VERTEX_POINT ( 'NONE', #23022 ) ;
#15298 = VECTOR ( 'NONE', #33923, 1000.000000000000000 ) ;
#15299 = CARTESIAN_POINT ( 'NONE',  ( 1.749999999999999778, -25.27164158951585549, 23.36088151536907631 ) ) ;
#15300 = ORIENTED_EDGE ( 'NONE', *, *, #22301, .T. ) ;
#15301 = CARTESIAN_POINT ( 'NONE',  ( -35.00000000000000000, 16.36947364650383818, -36.69637551990492597 ) ) ;
#15302 = CARTESIAN_POINT ( 'NONE',  ( -143.0000000000000568, -12.50000000000000888, -14.99999999999998757 ) ) ;
#15303 =( GEOMETRIC_REPRESENTATION_CONTEXT ( 3 ) GLOBAL_UNCERTAINTY_ASSIGNED_CONTEXT ( ( #7370 ) ) GLOBAL_UNIT_ASSIGNED_CONTEXT ( ( #24179, #32011, #7803 ) ) REPRESENTATION_CONTEXT ( 'NONE', 'WORKASPACE' ) );
#15304 = FACE_OUTER_BOUND ( 'NONE', #25134, .T. ) ;
#15305 = DIRECTION ( 'NONE',  ( 0.000000000000000000, -1.000000000000000000, -2.465190328815662439E-32 ) ) ;
#15306 = EDGE_CURVE ( 'NONE', #10280, #10318, #7469, .T. ) ;
#15307 = VERTEX_POINT ( 'NONE', #28534 ) ;
#15308 = AXIS2_PLACEMENT_3D ( 'NONE', #20621, #15115, #29149 ) ;
#15309 = ORIENTED_EDGE ( 'NONE', *, *, #19299, .F. ) ;
#15310 = CARTESIAN_POINT ( 'NONE',  ( 834.0028434499799914, 960.2916524184458922, 1753.598338701302964 ) ) ;
#15311 = VERTEX_POINT ( 'NONE', #15015 ) ;
#15312 = EDGE_CURVE ( 'NONE', #16142, #29708, #12344, .T. ) ;
#15313 = EDGE_CURVE ( 'NONE', #34550, #1890, #22256, .T. ) ;
#15314 = DIRECTION ( 'NONE',  ( 0.000000000000000000, 0.000000000000000000, 1.000000000000000000 ) ) ;
#15315 = EDGE_CURVE ( 'NONE', #6398, #14065, #10752, .T. ) ;
#15316 = AXIS2_PLACEMENT_3D ( 'NONE', #12182, #20523, #6808 ) ;
#15317 = DIRECTION ( 'NONE',  ( 0.000000000000000000, 1.836970198721029688E-16, -1.000000000000000000 ) ) ;
#15318 = CARTESIAN_POINT ( 'NONE',  ( 99.26191511054629757, -0.1972643383979439669, 7.500000000000013323 ) ) ;
#15319 = ITEM_DEFINED_TRANSFORMATION ( 'NONE', 'NONE', #5268,  #28566 ) ;
#15320 = ORIENTED_EDGE ( 'NONE', *, *, #508, .T. ) ;
#15321 = CARTESIAN_POINT ( 'NONE',  ( -414.0000000000000568, -137.0000000000000000, -175.0000000000000000 ) ) ;
#15322 = CIRCLE ( 'NONE', #27223, 22.50000000000000355 ) ;
#15324 = CARTESIAN_POINT ( 'NONE',  ( 1.749999999999999778, -2.430610048906265419, 34.32897884578299852 ) ) ;
#15323 = CARTESIAN_POINT ( 'NONE',  ( -110.1150203881707910, 3.166944581793445397E-20, 12.50000000000000000 ) ) ;
#15325 = ORIENTED_EDGE ( 'NONE', *, *, #9605, .F. ) ;
#15326 = ORIENTED_EDGE ( 'NONE', *, *, #2275, .F. ) ;
#15327 = DIRECTION ( 'NONE',  ( -1.000000000000000000, 0.000000000000000000, 0.000000000000000000 ) ) ;
#15328 = EDGE_LOOP ( 'NONE', ( #5345, #12864, #160, #16732 ) ) ;
#15329 = DIRECTION ( 'NONE',  ( 1.000000000000000000, 0.000000000000000000, 1.300283923313630633E-47 ) ) ;
#15330 = FACE_OUTER_BOUND ( 'NONE', #13262, .T. ) ;
#15331 = VERTEX_POINT ( 'NONE', #5488 ) ;
#15332 = AXIS2_PLACEMENT_3D ( 'NONE', #15951, #24276, #13792 ) ;
#15333 = CARTESIAN_POINT ( 'NONE',  ( -12.00000000000001066, 124.9999999999999716, 155.0000000000000000 ) ) ;
#15334 = B_SPLINE_CURVE_WITH_KNOTS ( 'NONE', 3,
 ( #24991, #16486, #18468, #3109 ),
 .UNSPECIFIED., .F., .F.,
 ( 4, 4 ),
 ( 0.002009632881715329999, 0.003746595525399130586 ),
 .UNSPECIFIED. ) ;
#15335 = ORIENTED_EDGE ( 'NONE', *, *, #2533, .T. ) ;
#15336 = CARTESIAN_POINT ( 'NONE',  ( 5.021133111224473033, 6.201984591278717041, -67.50000000000000000 ) ) ;
#15337 = SURFACE_STYLE_USAGE ( .BOTH. , #1619 ) ;
#15338 = DIRECTION ( 'NONE',  ( 0.000000000000000000, 0.000000000000000000, -1.000000000000000000 ) ) ;
#15340 = CARTESIAN_POINT ( 'NONE',  ( -19.99999999999998934, 112.9999999999999574, -175.0000000000000284 ) ) ;
#15339 = DIRECTION ( 'NONE',  ( -1.000000000000000000, -0.000000000000000000, -0.000000000000000000 ) ) ;
#15341 = AXIS2_PLACEMENT_3D ( 'NONE', #9628, #28324, #17494 ) ;
#15342 = CARTESIAN_POINT ( 'NONE',  ( 19.99999999999998934, -115.0000000000000000, 154.9999999999999716 ) ) ;
#15343 = DIRECTION ( 'NONE',  ( 0.000000000000000000, 0.000000000000000000, -1.000000000000000000 ) ) ;
#15344 = CARTESIAN_POINT ( 'NONE',  ( 0.006915246992955798207, 27.98916443103565399, -12.86217335695007868 ) ) ;
#15345 = CARTESIAN_POINT ( 'NONE',  ( 1.205771365940061957, -15.58845726811992449, 7.826847450972439323E-16 ) ) ;
#15346 = ORIENTED_EDGE ( 'NONE', *, *, #16350, .F. ) ;
#15347 = B_SPLINE_CURVE_WITH_KNOTS ( 'NONE', 3,
 ( #24586, #27794, #21934, #32950, #8751, #16794 ),
 .UNSPECIFIED., .F., .F.,
 ( 4, 2, 4 ),
 ( 2.126639591840295689E-07, 0.001873410972133593942, 0.003746609280308003942 ),
 .UNSPECIFIED. ) ;
#15348 =( NAMED_UNIT ( * ) SI_UNIT ( $, .STERADIAN. ) SOLID_ANGLE_UNIT ( ) );
#15349 = ORIENTED_EDGE ( 'NONE', *, *, #14333, .T. ) ;
#15350 = ORIENTED_EDGE ( 'NONE', *, *, #4198, .F. ) ;
#15351 = EDGE_CURVE ( 'NONE', #32651, #32967, #5184, .T. ) ;
#15352 = AXIS2_PLACEMENT_3D ( 'NONE', #12256, #9573, #34116 ) ;
#15353 = EDGE_CURVE ( 'NONE', #14577, #10753, #26552, .T. ) ;
#15354 = CARTESIAN_POINT ( 'NONE',  ( -19.99999999999998934, -112.9999999999999858, -155.0000000000000284 ) ) ;
#15355 = DIRECTION ( 'NONE',  ( -4.452700119515301548E-14, 4.992247762083357576E-14, 1.000000000000000000 ) ) ;
#15356 = EDGE_LOOP ( 'NONE', ( #3051, #15841, #10321, #34386 ) ) ;
#15357 = EDGE_LOOP ( 'NONE', ( #12584, #8209, #4270, #23675 ) ) ;
#15358 = VERTEX_POINT ( 'NONE', #10356 ) ;
#15359 = EDGE_CURVE ( 'NONE', #1031, #19038, #14314, .T. ) ;
#15360 = FACE_OUTER_BOUND ( 'NONE', #12342, .T. ) ;
#15361 = EDGE_LOOP ( 'NONE', ( #31637, #6135, #15564, #24418 ) ) ;
#15362 = CARTESIAN_POINT ( 'NONE',  ( 1.749999999999999778, -30.02688531850407472, 16.81585001935568613 ) ) ;
#15363 = LINE ( 'NONE', #1816, #9195 ) ;
#15364 = ORIENTED_EDGE ( 'NONE', *, *, #33541, .T. ) ;
#15365 = ORIENTED_EDGE ( 'NONE', *, *, #18428, .T. ) ;
#15366 =( REPRESENTATION_RELATIONSHIP ('NONE','NONE', #23037, #28231 ) REPRESENTATION_RELATIONSHIP_WITH_TRANSFORMATION ( #3391 )SHAPE_REPRESENTATION_RELATIONSHIP( ) );
#15367 = CARTESIAN_POINT ( 'NONE',  ( -6.500000000000000000, 0.000000000000000000, -0.7520000000000004459 ) ) ;
#15368 = LINE ( 'NONE', #17698, #10133 ) ;
#15369 = ADVANCED_FACE ( 'NONE', ( #696 ), #30067, .T. ) ;
#15370 = DIRECTION ( 'NONE',  ( 0.000000000000000000, 0.000000000000000000, -1.000000000000000000 ) ) ;
#15371 = CARTESIAN_POINT ( 'NONE',  ( -45.00000000000000000, 3.353962854566122864, -15.81122994652406355 ) ) ;
#15372 = DIRECTION ( 'NONE',  ( 0.000000000000000000, 0.000000000000000000, 1.000000000000000000 ) ) ;
#15373 = VERTEX_POINT ( 'NONE', #3352 ) ;
#15374 = CARTESIAN_POINT ( 'NONE',  ( 3.985664461616347742E-15, 32.54542015209057126, 76.74945698428001606 ) ) ;
#15375 = DIRECTION ( 'NONE',  ( 1.000000000000000000, 0.000000000000000000, 0.000000000000000000 ) ) ;
#15376 = FACE_OUTER_BOUND ( 'NONE', #12865, .T. ) ;
#15377 = EDGE_LOOP ( 'NONE', ( #22640, #17518, #27219, #21030 ) ) ;
#15378 = DIRECTION ( 'NONE',  ( -1.000000000000000000, -0.000000000000000000, -0.000000000000000000 ) ) ;
#15379 = DIRECTION ( 'NONE',  ( 0.8854131517428557308, -0.2458337514780907229, 0.3944734685057935120 ) ) ;
#15380 = AXIS2_PLACEMENT_3D ( 'NONE', #24392, #3033, #19608 ) ;
#15381 = CARTESIAN_POINT ( 'NONE',  ( 106.3573986772276498, 5.578557642680240569, -5.013303406467239931 ) ) ;
#15383 = CARTESIAN_POINT ( 'NONE',  ( 0.000000000000000000, -55.00000000000000711, 0.000000000000000000 ) ) ;
#15382 = DIRECTION ( 'NONE',  ( -1.000000000000000000, -0.000000000000000000, -0.000000000000000000 ) ) ;
#15384 = LINE ( 'NONE', #13065, #20139 ) ;
#15385 = ORIENTED_EDGE ( 'NONE', *, *, #21259, .T. ) ;
#15386 = LINE ( 'NONE', #18410, #8738 ) ;
#15388 = CARTESIAN_POINT ( 'NONE',  ( 0.5355294694855705639, 9.071383756617057870, -11.28790243858421327 ) ) ;
#15387 = PRESENTATION_STYLE_ASSIGNMENT (( #15560 ) ) ;
#15389 = ORIENTED_EDGE ( 'NONE', *, *, #6463, .F. ) ;
#15390 = AXIS2_PLACEMENT_3D ( 'NONE', #29144, #12611, #10105 ) ;
#15391 = DIRECTION ( 'NONE',  ( 0.000000000000000000, 0.000000000000000000, -1.000000000000000000 ) ) ;
#15392 = EDGE_LOOP ( 'NONE', ( #18687, #20356, #25768, #8900 ) ) ;
#15393 = EDGE_CURVE ( 'NONE', #19998, #9840, #29846, .T. ) ;
#15394 = EDGE_LOOP ( 'NONE', ( #19316, #2382, #10435, #9131 ) ) ;
#15395 = DIRECTION ( 'NONE',  ( 0.000000000000000000, -0.000000000000000000, 1.000000000000000000 ) ) ;
#15396 = EDGE_LOOP ( 'NONE', ( #28573, #31485, #22169, #20732 ) ) ;
#15397 = ORIENTED_EDGE ( 'NONE', *, *, #29850, .F. ) ;
#15398 = ADVANCED_FACE ( 'NONE', ( #19224 ), #27563, .T. ) ;
#15399 = CARTESIAN_POINT ( 'NONE',  ( -442.0000000000000000, -124.9999999999999716, 139.9999999999999716 ) ) ;
#15400 = EDGE_CURVE ( 'NONE', #22677, #16274, #22229, .T. ) ;
#15401 = VECTOR ( 'NONE', #24473, 1000.000000000000000 ) ;
#15402 = DIRECTION ( 'NONE',  ( -1.000000000000000000, -0.000000000000000000, -0.000000000000000000 ) ) ;
#15403 = DIRECTION ( 'NONE',  ( 0.000000000000000000, 0.000000000000000000, 1.000000000000000000 ) ) ;
#15404 = EDGE_CURVE ( 'NONE', #34690, #7524, #5658, .T. ) ;
#15405 = VERTEX_POINT ( 'NONE', #19568 ) ;
#15406 = ADVANCED_FACE ( 'NONE', ( #5834 ), #20553, .T. ) ;
#15407 = ORIENTED_EDGE ( 'NONE', *, *, #30261, .F. ) ;
#15408 = CARTESIAN_POINT ( 'NONE',  ( 2.789999999999999147, 2.005524111408194088, 31.87689292423238996 ) ) ;
#15409 = CARTESIAN_POINT ( 'NONE',  ( -8.000000000000000000, 0.000000000000000000, -11.79999999999999893 ) ) ;
#15410 = FACE_OUTER_BOUND ( 'NONE', #2796, .T. ) ;
#15411 = ADVANCED_FACE ( 'NONE', ( #25054 ), #3179, .T. ) ;
#15412 = DIRECTION ( 'NONE',  ( 1.000000000000000000, 0.000000000000000000, 0.000000000000000000 ) ) ;
#15413 = CARTESIAN_POINT ( 'NONE',  ( 11.99999999999999822, -64.99999999999997158, 154.9999999999999716 ) ) ;
#15414 = ORIENTED_EDGE ( 'NONE', *, *, #8140, .T. ) ;
#15415 = ORIENTED_EDGE ( 'NONE', *, *, #24814, .T. ) ;
#15416 = CARTESIAN_POINT ( 'NONE',  ( 30.45781707305797070, -22.50252913745434924, 68.31122994652405112 ) ) ;
#15417 = AXIS2_PLACEMENT_3D ( 'NONE', #1822, #20524, #28540 ) ;
#15418 = DIRECTION ( 'NONE',  ( 0.000000000000000000, 0.000000000000000000, 1.000000000000000000 ) ) ;
#15419 = ORIENTED_EDGE ( 'NONE', *, *, #15905, .F. ) ;
#15420 = CIRCLE ( 'NONE', #11987, 4.306175033202026547 ) ;
#15421 = VECTOR ( 'NONE', #30160, 1000.000000000000000 ) ;
#15422 = CARTESIAN_POINT ( 'NONE',  ( 2.261199740906818079, -11.04911166161924285, -31.50867056184630854 ) ) ;
#15423 = PLANE ( 'NONE',  #20043 ) ;
#15424 = CARTESIAN_POINT ( 'NONE',  ( 19.99999999999998934, -124.9999999999999432, -154.9999999999999716 ) ) ;
#15425 = ORIENTED_EDGE ( 'NONE', *, *, #20034, .F. ) ;
#15426 = CARTESIAN_POINT ( 'NONE',  ( 11.99999999999999645, 144.9999999999999716, 194.9999999999999716 ) ) ;
#15427 = ORIENTED_EDGE ( 'NONE', *, *, #16093, .T. ) ;
#15428 = VECTOR ( 'NONE', #12883, 1000.000000000000000 ) ;
#15430 = DIRECTION ( 'NONE',  ( 0.000000000000000000, 0.000000000000000000, 1.000000000000000000 ) ) ;
#15429 = DIRECTION ( 'NONE',  ( 0.000000000000000000, 0.000000000000000000, 1.000000000000000000 ) ) ;
#15431 = CARTESIAN_POINT ( 'NONE',  ( 0.000000000000000000, -29.00730259674847034, 9.328884633908835156 ) ) ;
#15432 = CIRCLE ( 'NONE', #67, 2.033421858999711507 ) ;
#15433 = ORIENTED_EDGE ( 'NONE', *, *, #9121, .F. ) ;
#15434 = FACE_OUTER_BOUND ( 'NONE', #9201, .T. ) ;
#15435 = CARTESIAN_POINT ( 'NONE',  ( -21.41424479178918361, -24.50784553716280101, 68.31122994652405112 ) ) ;
#15436 = ORIENTED_EDGE ( 'NONE', *, *, #27651, .T. ) ;
#15437 = AXIS2_PLACEMENT_3D ( 'NONE', #25640, #6595, #17495 ) ;
#15438 = DIRECTION ( 'NONE',  ( -0.1063910735369225230, 0.9943243633099118073, -1.000770725407345128E-14 ) ) ;
#15439 = VECTOR ( 'NONE', #29691, 1000.000000000000000 ) ;
#15441 = VERTEX_POINT ( 'NONE', #30414 ) ;
#15440 = AXIS2_PLACEMENT_3D ( 'NONE', #31401, #33904, #4989 ) ;
#15442 = CARTESIAN_POINT ( 'NONE',  ( 107.8890288426244410, -4.971563738489883200, 11.47098163371368251 ) ) ;
#15443 = ORIENTED_EDGE ( 'NONE', *, *, #16299, .T. ) ;
#15444 = VECTOR ( 'NONE', #8933, 1000.000000000000000 ) ;
#15445 = DIRECTION ( 'NONE',  ( 0.000000000000000000, 0.000000000000000000, -1.000000000000000000 ) ) ;
#15446 = CARTESIAN_POINT ( 'NONE',  ( -145.0000000000000568, 87.50000000000000000, -65.00000000000000000 ) ) ;
#15447 = CARTESIAN_POINT ( 'NONE',  ( -500.0000000000000000, -113.0000000000000000, 159.0000000000000000 ) ) ;
#15448 = CARTESIAN_POINT ( 'NONE',  ( -499.9999999999999432, 112.9999999999999574, -187.0000000000000000 ) ) ;
#15449 = EDGE_CURVE ( 'NONE', #31622, #34030, #7315, .T. ) ;
#15450 = ORIENTED_EDGE ( 'NONE', *, *, #32176, .F. ) ;
#15451 = EDGE_CURVE ( 'NONE', #27734, #30712, #22056, .T. ) ;
#15452 = VERTEX_POINT ( 'NONE', #8521 ) ;
#15453 = ORIENTED_EDGE ( 'NONE', *, *, #26320, .F. ) ;
#15454 = CARTESIAN_POINT ( 'NONE',  ( 2.790000000000080860, 23.76564585743019720, -19.37518496788493039 ) ) ;
#15456 = AXIS2_PLACEMENT_3D ( 'NONE', #33604, #28446, #25590 ) ;
#15455 = DIRECTION ( 'NONE',  ( 1.000000000000000000, 0.000000000000000000, 0.000000000000000000 ) ) ;
#15457 = DIRECTION ( 'NONE',  ( 0.000000000000000000, 1.836970198721029441E-16, -1.000000000000000000 ) ) ;
#15458 = CARTESIAN_POINT ( 'NONE',  ( 11.99999999999999645, -145.0000000000000000, 174.9999999999999432 ) ) ;
#15459 = CARTESIAN_POINT ( 'NONE',  ( 0.000000000000000000, -27.53147453683434520, 13.05640081644832939 ) ) ;
#15460 = PLANE ( 'NONE',  #30648 ) ;
#15461 = ORIENTED_EDGE ( 'NONE', *, *, #3652, .F. ) ;
#15462 = PRODUCT_DEFINITION_SHAPE ( 'NONE', 'NONE',  #35138 ) ;
#15463 = CARTESIAN_POINT ( 'NONE',  ( -365.0000000000000000, -119.0000000000000000, 113.9999999999999858 ) ) ;
#15464 = CARTESIAN_POINT ( 'NONE',  ( 0.5288002398009233884, 27.45925096103277241, -18.99654502929918465 ) ) ;
#15465 = EDGE_CURVE ( 'NONE', #6886, #8440, #13689, .T. ) ;
#15466 = VECTOR ( 'NONE', #19205, 1000.000000000000000 ) ;
#15467 = CARTESIAN_POINT ( 'NONE',  ( -145.0000000000000568, 87.50000000000000000, 65.00000000000000000 ) ) ;
#15468 = ORIENTED_EDGE ( 'NONE', *, *, #10734, .T. ) ;
#15469 = TOROIDAL_SURFACE ( 'NONE', #31921, 30.47050528711511674, 8.000000000000000000 ) ;
#15470 = AXIS2_PLACEMENT_3D ( 'NONE', #8106, #16491, #32139 ) ;
#15472 = AXIS2_PLACEMENT_3D ( 'NONE', #2498, #5683, #2850 ) ;
#15471 = DIRECTION ( 'NONE',  ( -0.000000000000000000, -0.000000000000000000, -1.000000000000000000 ) ) ;
#15473 = ORIENTED_EDGE ( 'NONE', *, *, #29645, .T. ) ;
#15474 = VECTOR ( 'NONE', #11224, 1000.000000000000000 ) ;
#15475 = FACE_OUTER_BOUND ( 'NONE', #14566, .T. ) ;
#15476 = EDGE_CURVE ( 'NONE', #16412, #24248, #27213, .T. ) ;
#15477 = DIRECTION ( 'NONE',  ( -0.000000000000000000, 1.000000000000000000, -0.000000000000000000 ) ) ;
#15478 = EDGE_CURVE ( 'NONE', #20728, #32317, #7442, .T. ) ;
#15479 = EDGE_CURVE ( 'NONE', #32751, #18201, #25236, .T. ) ;
#15480 = CARTESIAN_POINT ( 'NONE',  ( 21.24400529595485310, -24.65555945140048522, 68.31122994652405112 ) ) ;
#15481 = CARTESIAN_POINT ( 'NONE',  ( 0.000000000000000000, -0.09145294252657359957, -30.47036804522409525 ) ) ;
#15482 = CARTESIAN_POINT ( 'NONE',  ( 12.00000000000001066, -134.9999999999999716, 194.9999999999999716 ) ) ;
#15483 = ADVANCED_FACE ( 'NONE', ( #9227 ), #1396, .T. ) ;
#15484 = VERTEX_POINT ( 'NONE', #1220 ) ;
#15485 = EDGE_LOOP ( 'NONE', ( #25033, #5935, #17385, #19724 ) ) ;
#15486 = CARTESIAN_POINT ( 'NONE',  ( 787.8120956739329586, 1048.916146239734189, 1753.598338701303419 ) ) ;
#15487 = VERTEX_POINT ( 'NONE', #6550 ) ;
#15488 = DIRECTION ( 'NONE',  ( 0.000000000000000000, 1.836970198721029441E-16, -1.000000000000000000 ) ) ;
#15489 = DIRECTION ( 'NONE',  ( 0.000000000000000000, 0.000000000000000000, -1.000000000000000000 ) ) ;
#15490 = CARTESIAN_POINT ( 'NONE',  ( 101.5068632955307208, -4.566352457759228045, 5.955250171528614800 ) ) ;
#15491 = ADVANCED_FACE ( 'NONE', ( #6723, #25951 ), #1046, .T. ) ;
#15492 = ORIENTED_EDGE ( 'NONE', *, *, #1248, .T. ) ;
#15493 = CARTESIAN_POINT ( 'NONE',  ( 0.000000000000000000, 0.000000000000000000, 0.000000000000000000 ) ) ;
#15495 = CARTESIAN_POINT ( 'NONE',  ( -365.0000000000000000, 130.9999999999999716, 126.0000000000000000 ) ) ;
#15494 = CARTESIAN_POINT ( 'NONE',  ( 2.033800778447012014, 27.12277411069248245, 20.36158770325061695 ) ) ;
#15496 = ORIENTED_EDGE ( 'NONE', *, *, #23991, .F. ) ;
#15497 = VERTEX_POINT ( 'NONE', #30595 ) ;
#15498 = DIRECTION ( 'NONE',  ( 0.6876994588534236508, 0.7259954919231305093, -0.000000000000000000 ) ) ;
#15499 = VERTEX_POINT ( 'NONE', #28276 ) ;
#15500 = CYLINDRICAL_SURFACE ( 'NONE', #8438, 16.19999999999999929 ) ;
#15501 = DIRECTION ( 'NONE',  ( -1.000000000000000000, 0.000000000000000000, 0.000000000000000000 ) ) ;
#15502 = ORIENTED_EDGE ( 'NONE', *, *, #31570, .T. ) ;
#15503 = LINE ( 'NONE', #26519, #13459 ) ;
#15504 = ORIENTED_EDGE ( 'NONE', *, *, #27559, .F. ) ;
#15505 = PLANE ( 'NONE',  #11806 ) ;
#15506 = CARTESIAN_POINT ( 'NONE',  ( -29.68486519896224962, 23.49918569563710946, 68.31122994652405112 ) ) ;
#15507 = DIRECTION ( 'NONE',  ( -0.7071067811865435759, 0.000000000000000000, 0.7071067811865514585 ) ) ;
#15508 = EDGE_CURVE ( 'NONE', #17362, #32005, #6186, .T. ) ;
#15511 = LINE ( 'NONE', #15340, #33858 ) ;
#15510 = CARTESIAN_POINT ( 'NONE',  ( 22.89764159710611224, 13.56412600238610366, -77.50000000000000000 ) ) ;
#15509 = AXIS2_PLACEMENT_3D ( 'NONE', #14080, #3736, #724 ) ;
#15512 = EDGE_CURVE ( 'NONE', #11201, #7081, #20097, .T. ) ;
#15513 = VECTOR ( 'NONE', #16745, 1000.000000000000000 ) ;
#15514 = VECTOR ( 'NONE', #16271, 1000.000000000000000 ) ;
#15515 = CIRCLE ( 'NONE', #22909, 30.47050528711512030 ) ;
#15516 = FACE_OUTER_BOUND ( 'NONE', #20039, .T. ) ;
#15517 = CARTESIAN_POINT ( 'NONE',  ( -5.021133111224782120, 16.12922284503173742, -67.50000000000000000 ) ) ;
#15518 = CARTESIAN_POINT ( 'NONE',  ( 0.02407890056655738464, 28.29688452313417812, -12.88099432405573630 ) ) ;
#15519 = DIRECTION ( 'NONE',  ( 1.000000000000000000, 0.000000000000000000, 0.000000000000000000 ) ) ;
#15520 = ORIENTED_EDGE ( 'NONE', *, *, #14796, .F. ) ;
#15521 = ORIENTED_EDGE ( 'NONE', *, *, #19745, .F. ) ;
#15522 = ORIENTED_EDGE ( 'NONE', *, *, #33879, .F. ) ;
#15523 = FACE_OUTER_BOUND ( 'NONE', #11724, .T. ) ;
#15524 = CARTESIAN_POINT ( 'NONE',  ( 822.4997240610829294, 1334.697290463532227, 1678.876119909286672 ) ) ;
#15525 = VERTEX_POINT ( 'NONE', #12092 ) ;
#15526 = ORIENTED_EDGE ( 'NONE', *, *, #21739, .T. ) ;
#15527 = EDGE_LOOP ( 'NONE', ( #28302, #25889, #30640, #27497 ) ) ;
#15528 = DIRECTION ( 'NONE',  ( 0.000000000000000000, 0.000000000000000000, 1.000000000000000000 ) ) ;
#15529 = AXIS2_PLACEMENT_3D ( 'NONE', #5997, #19209, #5818 ) ;
#15530 = ORIENTED_EDGE ( 'NONE', *, *, #610, .F. ) ;
#15531 = CARTESIAN_POINT ( 'NONE',  ( 11.99999999999999645, 140.9999999999999716, -155.0000000000000000 ) ) ;
#15532 = VECTOR ( 'NONE', #6160, 1000.000000000000000 ) ;
#15533 = CARTESIAN_POINT ( 'NONE',  ( 0.000000000000000000, 3.524919873834583163E-15, 68.31122994652405112 ) ) ;
#15534 = VERTEX_POINT ( 'NONE', #22586 ) ;
#15535 = VECTOR ( 'NONE', #22125, 1000.000000000000000 ) ;
#15536 = ORIENTED_EDGE ( 'NONE', *, *, #15862, .F. ) ;
#15537 = VECTOR ( 'NONE', #32952, 1000.000000000000000 ) ;
#15538 = CARTESIAN_POINT ( 'NONE',  ( -500.0000000000000000, -137.0000000000000000, 190.9999999999999716 ) ) ;
#15539 = DIRECTION ( 'NONE',  ( 0.05413890858541543089, 0.9985334138511240409, 0.000000000000000000 ) ) ;
#15540 = FACE_OUTER_BOUND ( 'NONE', #20450, .T. ) ;
#15541 = LINE ( 'NONE', #18579, #27331 ) ;
#15542 = FACE_OUTER_BOUND ( 'NONE', #16534, .T. ) ;
#15543 = EDGE_LOOP ( 'NONE', ( #15415, #29772, #20086, #17085 ) ) ;
#15544 = DIRECTION ( 'NONE',  ( 0.000000000000000000, 0.000000000000000000, -1.000000000000000000 ) ) ;
#15545 = CARTESIAN_POINT ( 'NONE',  ( -499.9999999999999432, -113.0000000000000000, -159.0000000000000000 ) ) ;
#15546 = ORIENTED_EDGE ( 'NONE', *, *, #25588, .F. ) ;
#15547 = CARTESIAN_POINT ( 'NONE',  ( 0.1835380628080924836, -24.33633102984340724, -21.19365992153305100 ) ) ;
#15548 = EDGE_CURVE ( 'NONE', #9992, #27517, #5735, .T. ) ;
#15549 = CARTESIAN_POINT ( 'NONE',  ( 15.99999999999998579, -55.00000000000000711, -154.9999999999999716 ) ) ;
#15550 = DIRECTION ( 'NONE',  ( -1.000000000000000000, 0.000000000000000000, 0.000000000000000000 ) ) ;
#15551 = ADVANCED_FACE ( 'NONE', ( #33788 ), #30762, .F. ) ;
#15553 = CARTESIAN_POINT ( 'NONE',  ( -107.3021478268368014, 4.579603235088350210, -5.941779048586183443 ) ) ;
#15552 = CARTESIAN_POINT ( 'NONE',  ( 20.62763069236413926, -31.74750072459299588, 49.43553178847298568 ) ) ;
#15554 = EDGE_CURVE ( 'NONE', #12516, #32323, #3524, .T. ) ;
#15555 = AXIS2_PLACEMENT_3D ( 'NONE', #12714, #21051, #15737 ) ;
#15556 = CARTESIAN_POINT ( 'NONE',  ( -365.0000000000000000, 130.9999999999999716, 111.9999999999999858 ) ) ;
#15557 = ORIENTED_EDGE ( 'NONE', *, *, #9565, .F. ) ;
#15558 = EDGE_CURVE ( 'NONE', #22891, #25011, #6367, .T. ) ;
#15559 = CARTESIAN_POINT ( 'NONE',  ( 105.9472385653803173, 5.662516510817760640, -11.14395138485681436 ) ) ;
#15561 = CARTESIAN_POINT ( 'NONE',  ( 0.2204769333330932612, 10.04478976116410927, -9.601913782316097823 ) ) ;
#15560 = SURFACE_STYLE_USAGE ( .BOTH. , #28901 ) ;
#15562 = AXIS2_PLACEMENT_3D ( 'NONE', #23990, #34511, #7439 ) ;
#15564 = ORIENTED_EDGE ( 'NONE', *, *, #9298, .T. ) ;
#15563 = CIRCLE ( 'NONE', #19555, 4.309328216469825001 ) ;
#15565 = VECTOR ( 'NONE', #8893, 1000.000000000000000 ) ;
#15566 = DIRECTION ( 'NONE',  ( -1.000000000000000000, 0.000000000000000000, 0.000000000000000000 ) ) ;
#15567 = PRODUCT_DEFINITION_SHAPE ( 'NONE', 'NONE',  #35211 ) ;
#15568 = VERTEX_POINT ( 'NONE', #22934 ) ;
#15569 =( REPRESENTATION_RELATIONSHIP ('NONE','NONE', #23037, #28231 ) REPRESENTATION_RELATIONSHIP_WITH_TRANSFORMATION ( #18483 )SHAPE_REPRESENTATION_RELATIONSHIP( ) );
#15570 = VERTEX_POINT ( 'NONE', #31125 ) ;
#15571 = DIRECTION ( 'NONE',  ( 0.000000000000000000, -1.000000000000000000, 3.374343856708137958E-53 ) ) ;
#15572 = EDGE_LOOP ( 'NONE', ( #21737, #545, #5211, #955 ) ) ;
#15573 = ORIENTED_EDGE ( 'NONE', *, *, #1889, .T. ) ;
#15574 = CARTESIAN_POINT ( 'NONE',  ( 1.394999999999999574, -10.89151784028265801, -32.64600270996228204 ) ) ;
#15575 = CIRCLE ( 'NONE', #28630, 3.999999999999976019 ) ;
#15576 = DIRECTION ( 'NONE',  ( 0.000000000000000000, 0.000000000000000000, 1.000000000000000000 ) ) ;
#15577 = FACE_OUTER_BOUND ( 'NONE', #22262, .T. ) ;
#15578 = ORIENTED_EDGE ( 'NONE', *, *, #18287, .T. ) ;
#15579 = ORIENTED_EDGE ( 'NONE', *, *, #17357, .T. ) ;
#15580 = DIRECTION ( 'NONE',  ( -0.6876994588534225405, 0.7259954919231316195, 0.000000000000000000 ) ) ;
#15581 = CARTESIAN_POINT ( 'NONE',  ( -12.00000000000001066, 144.9999999999999716, 155.0000000000000000 ) ) ;
#15582 = CARTESIAN_POINT ( 'NONE',  ( 0.000000000000000000, 3.524919873834583163E-15, 68.31122994652405112 ) ) ;
#15583 = DIRECTION ( 'NONE',  ( 0.000000000000000000, 0.8486862100397269959, -0.5288966977476834419 ) ) ;
#15584 = DIRECTION ( 'NONE',  ( 1.000000000000000000, 0.000000000000000000, 0.000000000000000000 ) ) ;
#15585 = UNCERTAINTY_MEASURE_WITH_UNIT (LENGTH_MEASURE( 1.000000000000000082E-05 ), #5257, 'distance_accuracy_value', 'NONE');
#15586 = VERTEX_POINT ( 'NONE', #12443 ) ;
#15587 = PRODUCT_DEFINITION_FORMATION_WITH_SPECIFIED_SOURCE ( 'ANY', '', #985, .NOT_KNOWN. ) ;
#15588 = ORIENTED_EDGE ( 'NONE', *, *, #28908, .T. ) ;
#15589 = CARTESIAN_POINT ( 'NONE',  ( -345.0000000000000000, -125.0000000000000284, 168.9999999999999716 ) ) ;
#15590 = AXIS2_PLACEMENT_3D ( 'NONE', #28340, #757, #6429 ) ;
#15591 = AXIS2_PLACEMENT_3D ( 'NONE', #17554, #3809, #8987 ) ;
#15592 = CARTESIAN_POINT ( 'NONE',  ( 1.040000000000000924, -18.66807150955393624, -28.91175816027522316 ) ) ;
#15593 = ORIENTED_EDGE ( 'NONE', *, *, #24746, .F. ) ;
#15594 = EDGE_CURVE ( 'NONE', #4360, #25058, #30200, .T. ) ;
#15595 = AXIS2_PLACEMENT_3D ( 'NONE', #9307, #3600, #23480 ) ;
#15596 = CARTESIAN_POINT ( 'NONE',  ( 1.394999999999999574, 14.89726405156217126, 31.02351007835983054 ) ) ;
#15597 = DIRECTION ( 'NONE',  ( 0.000000000000000000, 0.000000000000000000, 1.000000000000000000 ) ) ;
#15598 = EDGE_CURVE ( 'NONE', #10504, #23746, #20001, .T. ) ;
#15599 = CARTESIAN_POINT ( 'NONE',  ( 2.765921099434983876, -15.32140196853734970, -27.05343472113007763 ) ) ;
#15600 = ORIENTED_EDGE ( 'NONE', *, *, #17732, .F. ) ;
#15601 = CARTESIAN_POINT ( 'NONE',  ( -15.99999999999998579, 124.9999999999999716, 162.9999999999999716 ) ) ;
#15602 = ORIENTED_EDGE ( 'NONE', *, *, #18488, .F. ) ;
#15603 = DIRECTION ( 'NONE',  ( 0.000000000000000000, 1.836970198721029441E-16, -1.000000000000000000 ) ) ;
#15604 = ORIENTED_EDGE ( 'NONE', *, *, #13932, .T. ) ;
#15605 = ADVANCED_FACE ( 'NONE', ( #17784 ), #25770, .T. ) ;
#15607 = CARTESIAN_POINT ( 'NONE',  ( 0.000000000000000000, 45.00000000000000711, -36.68877005347592757 ) ) ;
#15606 =( NAMED_UNIT ( * ) SI_UNIT ( $, .STERADIAN. ) SOLID_ANGLE_UNIT ( ) );
#15608 = DIRECTION ( 'NONE',  ( 0.000000000000000000, 1.000000000000000000, -3.374343856708137958E-53 ) ) ;
#15609 = VECTOR ( 'NONE', #22923, 1000.000000000000000 ) ;
#15610 = VERTEX_POINT ( 'NONE', #23122 ) ;
#15611 = EDGE_CURVE ( 'NONE', #1054, #9976, #33962, .T. ) ;
#15612 = PLANE ( 'NONE',  #23405 ) ;
#15613 = LINE ( 'NONE', #9904, #11118 ) ;
#15614 = VECTOR ( 'NONE', #7275, 1000.000000000000000 ) ;
#15615 = EDGE_CURVE ( 'NONE', #10302, #9321, #27912, .T. ) ;
#15616 = EDGE_LOOP ( 'NONE', ( #6084, #17766, #29454, #13639 ) ) ;
#15617 = EDGE_CURVE ( 'NONE', #7575, #17615, #3705, .T. ) ;
#15618 = CARTESIAN_POINT ( 'NONE',  ( 212.5000000000000000, 1.224646799147353256E-15, -10.00000000000000000 ) ) ;
#15619 = AXIS2_PLACEMENT_3D ( 'NONE', #933, #11433, #19457 ) ;
#15620 = DIRECTION ( 'NONE',  ( -7.893605728314051750E-14, 1.618803117314786530E-15, 1.000000000000000000 ) ) ;
#15621 = VECTOR ( 'NONE', #8231, 1000.000000000000227 ) ;
#15622 = EDGE_LOOP ( 'NONE', ( #5656, #28162, #4355, #30797 ) ) ;
#15623 = CARTESIAN_POINT ( 'NONE',  ( 99.56119438876471861, -1.867505626284030162, 12.36477516193776260 ) ) ;
#15624 = EDGE_LOOP ( 'NONE', ( #17477, #16785, #33173, #29986 ) ) ;
#15625 = LINE ( 'NONE', #27156, #23544 ) ;
#15626 = CARTESIAN_POINT ( 'NONE',  ( -418.0000000000000000, -137.0000000000000000, 154.9999999999999716 ) ) ;
#15627 = CARTESIAN_POINT ( 'NONE',  ( -101.8763945071601285, -4.063426306576022995, -6.307665442424296387 ) ) ;
#15628 = DIRECTION ( 'NONE',  ( -1.000000000000000000, 0.000000000000000000, -5.546364386991661285E-52 ) ) ;
#15629 = ITEM_DEFINED_TRANSFORMATION ( 'NONE', 'NONE', #7558,  #28566 ) ;
#15630 = ORIENTED_EDGE ( 'NONE', *, *, #18810, .F. ) ;
#15631 = ORIENTED_EDGE ( 'NONE', *, *, #34381, .F. ) ;
#15632 = VERTEX_POINT ( 'NONE', #10101 ) ;
#15633 = DIRECTION ( 'NONE',  ( 1.000000000000000000, 0.000000000000000000, 0.000000000000000000 ) ) ;
#15634 = CARTESIAN_POINT ( 'NONE',  ( 0.000000000000000000, -29.69698570178027808, 11.75786841620004175 ) ) ;
#15635 = VECTOR ( 'NONE', #27114, 1000.000000000000000 ) ;
#15636 = CARTESIAN_POINT ( 'NONE',  ( -9.978866888775632660, -5.758675521474011738, -87.50000000000000000 ) ) ;
#15637 = DIRECTION ( 'NONE',  ( 0.000000000000000000, 1.000000000000000000, 0.000000000000000000 ) ) ;
#15638 = CARTESIAN_POINT ( 'NONE',  ( 19.99999999999998934, 136.9999999999999716, -175.0000000000000284 ) ) ;
#15639 = CYLINDRICAL_SURFACE ( 'NONE', #27203, 2.524999999999999467 ) ;
#15640 = ORIENTED_EDGE ( 'NONE', *, *, #7854, .T. ) ;
#15641 = VECTOR ( 'NONE', #5097, 1000.000000000000000 ) ;
#15642 = DIRECTION ( 'NONE',  ( 0.000000000000000000, 0.000000000000000000, 1.000000000000000000 ) ) ;
#15643 = DIRECTION ( 'NONE',  ( 1.300283923313630633E-47, 0.000000000000000000, 1.000000000000000000 ) ) ;
#15644 = ORIENTED_EDGE ( 'NONE', *, *, #14811, .F. ) ;
#15645 = FACE_OUTER_BOUND ( 'NONE', #5392, .T. ) ;
#15646 = EDGE_LOOP ( 'NONE', ( #3778, #15136, #25428, #23992 ) ) ;
#15647 = VECTOR ( 'NONE', #14389, 1000.000000000000000 ) ;
#15648 = VECTOR ( 'NONE', #1072, 1000.000000000000000 ) ;
#15649 = DIRECTION ( 'NONE',  ( 0.000000000000000000, 1.836970198721029441E-16, -1.000000000000000000 ) ) ;
#15650 = VERTEX_POINT ( 'NONE', #10274 ) ;
#15651 = DIRECTION ( 'NONE',  ( 0.000000000000000000, -0.5288966977476834419, 0.8486862100397269959 ) ) ;
#15652 = EDGE_CURVE ( 'NONE', #5999, #27971, #20613, .T. ) ;
#15653 = DIRECTION ( 'NONE',  ( 0.000000000000000000, -1.224646799147353207E-16, 1.000000000000000000 ) ) ;
#15654 = ADVANCED_BREP_SHAPE_REPRESENTATION ( '', ( #10823, #28566 ), #5242 ) ;
#15655 = EDGE_LOOP ( 'NONE', ( #18276, #27368, #10128, #8705, #24856, #21344, #11918, #33224 ) ) ;
#15656 = ADVANCED_FACE ( 'NONE', ( #9928 ), #18489, .F. ) ;
#15657 = EDGE_CURVE ( 'NONE', #18691, #2115, #29328, .T. ) ;
#15658 = CARTESIAN_POINT ( 'NONE',  ( -20.00000000000007461, 136.9999999999999432, -187.0000000000000000 ) ) ;
#15659 = LINE ( 'NONE', #33982, #8813 ) ;
#15660 = DIRECTION ( 'NONE',  ( 0.000000000000000000, 1.000000000000000000, -0.000000000000000000 ) ) ;
#15661 = ORIENTED_EDGE ( 'NONE', *, *, #6303, .F. ) ;
#15662 = AXIS2_PLACEMENT_3D ( 'NONE', #5692, #32760, #21732 ) ;
#15663 = EDGE_LOOP ( 'NONE', ( #7897, #24334, #17855, #4975 ) ) ;
#15664 = DIRECTION ( 'NONE',  ( -0.1063910735369017202, 0.9943243633099136947, -1.000770725407181676E-14 ) ) ;
#15665 = VECTOR ( 'NONE', #29106, 1000.000000000000000 ) ;
#15666 = ORIENTED_EDGE ( 'NONE', *, *, #10132, .F. ) ;
#15667 = AXIS2_PLACEMENT_3D ( 'NONE', #16340, #29506, #5452 ) ;
#15668 = EDGE_CURVE ( 'NONE', #12145, #19346, #34212, .T. ) ;
#15669 = CARTESIAN_POINT ( 'NONE',  ( 0.000000000000000000, 3.524919873834583163E-15, 68.31122994652405112 ) ) ;
#15670 = CARTESIAN_POINT ( 'NONE',  ( 0.000000000000000000, -33.69708579775584667, 49.43553178847298568 ) ) ;
#15671 = CARTESIAN_POINT ( 'NONE',  ( 105.3950378164618229, -5.727834534852265236, 4.841784820303065118 ) ) ;
#15672 = CIRCLE ( 'NONE', #4840, 10.00000000000000000 ) ;
#15673 = ORIENTED_EDGE ( 'NONE', *, *, #33046, .F. ) ;
#15674 = AXIS2_PLACEMENT_3D ( 'NONE', #17034, #14535, #22714 ) ;
#15675 = PLANE ( 'NONE',  #1615 ) ;
#15676 = AXIS2_PLACEMENT_3D ( 'NONE', #10948, #32604, #27453 ) ;
#15677 = EDGE_CURVE ( 'NONE', #3383, #24130, #18886, .T. ) ;
#15678 = ADVANCED_FACE ( 'NONE', ( #12790 ), #21314, .T. ) ;
#15679 = CIRCLE ( 'NONE', #20226, 3.999999999999976019 ) ;
#15681 = CARTESIAN_POINT ( 'NONE',  ( 2.606461809142830433, -3.232363112765826330, 32.10887868570996773 ) ) ;
#15680 = FACE_OUTER_BOUND ( 'NONE', #23977, .T. ) ;
#15682 = EDGE_CURVE ( 'NONE', #20094, #27049, #20787, .T. ) ;
#15683 = VERTEX_POINT ( 'NONE', #26648 ) ;
#15684 = EDGE_LOOP ( 'NONE', ( #6362, #28839, #32832, #26997 ) ) ;
#15685 = CARTESIAN_POINT ( 'NONE',  ( -34.04247984038124031, 16.56841925338180488, 68.31122994652405112 ) ) ;
#15686 = ORIENTED_EDGE ( 'NONE', *, *, #1128, .F. ) ;
#15687 = EDGE_CURVE ( 'NONE', #474, #1054, #34134, .T. ) ;
#15688 = LINE ( 'NONE', #28669, #13556 ) ;
#15689 = CARTESIAN_POINT ( 'NONE',  ( -23.78520691327551972, 22.21414650552150860, -36.68877005347593467 ) ) ;
#15690 = ORIENTED_EDGE ( 'NONE', *, *, #20572, .T. ) ;
#15691 = CIRCLE ( 'NONE', #14551, 34.41491905851385269 ) ;
#15692 = LINE ( 'NONE', #23330, #27094 ) ;
#15693 = ORIENTED_EDGE ( 'NONE', *, *, #3556, .F. ) ;
#15694 = VECTOR ( 'NONE', #24097, 1000.000000000000000 ) ;
#15695 = CARTESIAN_POINT ( 'NONE',  ( -499.9999999999999432, -141.0000000000000000, -187.0000000000000000 ) ) ;
#15696 = CARTESIAN_POINT ( 'NONE',  ( 28.11866956577617316, 16.38733641342591341, 49.43553178847298568 ) ) ;
#15698 = CARTESIAN_POINT ( 'NONE',  ( 22.89764159710615132, -1.579009122040560431, -87.50000000000000000 ) ) ;
#15697 = FACE_OUTER_BOUND ( 'NONE', #31319, .T. ) ;
#15699 = EDGE_CURVE ( 'NONE', #10968, #2751, #9776, .T. ) ;
#15700 = ADVANCED_FACE ( 'NONE', ( #7771 ), #15817, .F. ) ;
#15701 = CARTESIAN_POINT ( 'NONE',  ( -442.0000000000000000, 105.0000000000000000, 132.0000000000000000 ) ) ;
#15702 = DIRECTION ( 'NONE',  ( 5.546364386991661285E-52, 0.000000000000000000, 1.000000000000000000 ) ) ;
#15703 = LINE ( 'NONE', #13027, #28666 ) ;
#15704 = CARTESIAN_POINT ( 'NONE',  ( 2.783128901175710990, 18.40312061469657579, -24.78412275958813282 ) ) ;
#15705 = ORIENTED_EDGE ( 'NONE', *, *, #19604, .F. ) ;
#15706 = CARTESIAN_POINT ( 'NONE',  ( 826.3720134449782790, 1261.339464624697257, 1753.598338701303192 ) ) ;
#15707 = EDGE_LOOP ( 'NONE', ( #27196, #7397, #3147, #18453, #31974, #26827, #30177, #19880 ) ) ;
#15708 = VERTEX_POINT ( 'NONE', #13133 ) ;
#15709 = VECTOR ( 'NONE', #21614, 1000.000000000000114 ) ;
#15710 = CARTESIAN_POINT ( 'NONE',  ( 2.789999999999999147, 25.67797970382134309, 16.40405592474765939 ) ) ;
#15711 = DIRECTION ( 'NONE',  ( 0.000000000000000000, -1.000000000000000000, 0.000000000000000000 ) ) ;
#15712 = ORIENTED_EDGE ( 'NONE', *, *, #4030, .T. ) ;
#15713 = VERTEX_POINT ( 'NONE', #2092 ) ;
#15714 = FACE_OUTER_BOUND ( 'NONE', #33873, .T. ) ;
#15715 = DIRECTION ( 'NONE',  ( 0.000000000000000000, 0.000000000000000000, 1.000000000000000000 ) ) ;
#15716 = EDGE_CURVE ( 'NONE', #1290, #11374, #26822, .T. ) ;
#15717 = CONTEXT_DEPENDENT_SHAPE_REPRESENTATION ( #13545, #34603 ) ;
#15719 = EDGE_CURVE ( 'NONE', #30318, #17643, #25578, .T. ) ;
#15718 = B_SPLINE_CURVE_WITH_KNOTS ( 'NONE', 3,
 ( #22660, #9115, #19983, #30835 ),
 .UNSPECIFIED., .F., .F.,
 ( 4, 4 ),
 ( 3.087659402431792624E-07, 0.0006880453895802092143 ),
 .UNSPECIFIED. ) ;
#15720 = PLANE ( 'NONE',  #15246 ) ;
#15721 = CARTESIAN_POINT ( 'NONE',  ( 11.99999999999999645, -55.00000000000002132, 162.9999999999999716 ) ) ;
#15722 = ORIENTED_EDGE ( 'NONE', *, *, #12842, .T. ) ;
#15723 = ORIENTED_EDGE ( 'NONE', *, *, #10412, .T. ) ;
#15724 = CARTESIAN_POINT ( 'NONE',  ( -500.0000000000000000, -113.0000000000000000, 162.9999999999999716 ) ) ;
#15725 = CARTESIAN_POINT ( 'NONE',  ( 0.006871111354928813829, 25.89075856630370964, -16.81059844634632228 ) ) ;
#15726 = AXIS2_PLACEMENT_3D ( 'NONE', #26795, #34284, #23605 ) ;
#15727 = EDGE_CURVE ( 'NONE', #10508, #23413, #32502, .T. ) ;
#15728 = LINE ( 'NONE', #29585, #8493 ) ;
#15729 = CARTESIAN_POINT ( 'NONE',  ( 0.000000000000000000, 0.000000000000000000, 5.429999999999999716 ) ) ;
#15730 = DIRECTION ( 'NONE',  ( -1.000000000000000000, 0.000000000000000000, 0.000000000000000000 ) ) ;
#15731 = EDGE_LOOP ( 'NONE', ( #19928, #3841, #7998, #25452, #29923, #8236, #2264, #2827, #13588, #34164, #13960 ) ) ;
#15732 = DIRECTION ( 'NONE',  ( -0.000000000000000000, -1.000000000000000000, -0.000000000000000000 ) ) ;
#15733 = DIRECTION ( 'NONE',  ( 0.000000000000000000, 1.836970198721029441E-16, -1.000000000000000000 ) ) ;
#15734 = B_SPLINE_CURVE_WITH_KNOTS ( 'NONE', 3,
 ( #11946, #6400, #3384, #19780, #1251, #22443 ),
 .UNSPECIFIED., .F., .F.,
 ( 4, 2, 4 ),
 ( 2.570076372303527286E-07, 0.001873455364168429135, 0.003746653720699627977 ),
 .UNSPECIFIED. ) ;
#15735 = EDGE_CURVE ( 'NONE', #28091, #2086, #31911, .T. ) ;
#15736 = FACE_OUTER_BOUND ( 'NONE', #5561, .T. ) ;
#15737 = DIRECTION ( 'NONE',  ( 1.000000000000000000, 0.000000000000000000, 0.000000000000000000 ) ) ;
#15738 = FACE_BOUND ( 'NONE', #3027, .T. ) ;
#15740 = CARTESIAN_POINT ( 'NONE',  ( 0.000000000000000000, 0.000000000000000000, 0.000000000000000000 ) ) ;
#15739 = CARTESIAN_POINT ( 'NONE',  ( 0.000000000000000000, -23.41952779159775488, 19.49300927180538778 ) ) ;
#15741 = AXIS2_PLACEMENT_3D ( 'NONE', #22979, #1437, #33834 ) ;
#15742 = CARTESIAN_POINT ( 'NONE',  ( -19.99999999999998934, -56.99999999999997868, -154.9999999999999716 ) ) ;
#15743 = ORIENTED_EDGE ( 'NONE', *, *, #17297, .T. ) ;
#15744 = LINE ( 'NONE', #34597, #19029 ) ;
#15746 = LINE ( 'NONE', #23897, #20837 ) ;
#15745 = FACE_OUTER_BOUND ( 'NONE', #21103, .T. ) ;
#15747 = CIRCLE ( 'NONE', #19147, 0.3000000000000016542 ) ;
#15748 = EDGE_LOOP ( 'NONE', ( #23447, #26196 ) ) ;
#15749 = DIRECTION ( 'NONE',  ( 0.000000000000000000, -1.224646799147353207E-16, 1.000000000000000000 ) ) ;
#15750 = EDGE_CURVE ( 'NONE', #19356, #31410, #20501, .T. ) ;
#15751 = AXIS2_PLACEMENT_3D ( 'NONE', #9685, #26752, #4498 ) ;
#15752 = VERTEX_POINT ( 'NONE', #34308 ) ;
#15753 = ORIENTED_EDGE ( 'NONE', *, *, #25356, .F. ) ;
#15754 = CARTESIAN_POINT ( 'NONE',  ( 2.765921099433443331, -29.68817180695682723, 9.232883799364120847 ) ) ;
#15755 = ORIENTED_EDGE ( 'NONE', *, *, #16191, .T. ) ;
#15756 = ORIENTED_EDGE ( 'NONE', *, *, #6337, .T. ) ;
#15757 = DIRECTION ( 'NONE',  ( 0.000000000000000000, 1.000000000000000000, 1.224646799147353207E-16 ) ) ;
#15758 = AXIS2_PLACEMENT_3D ( 'NONE', #6418, #28149, #1098 ) ;
#15759 = EDGE_CURVE ( 'NONE', #181, #21502, #31632, .T. ) ;
#15760 = ADVANCED_FACE ( 'NONE', ( #1908 ), #27002, .F. ) ;
#15761 = VECTOR ( 'NONE', #15498, 1000.000000000000114 ) ;
#15762 = EDGE_CURVE ( 'NONE', #9264, #26418, #14191, .T. ) ;
#15763 = DIRECTION ( 'NONE',  ( 1.000000000000000000, 3.040835319149746090E-31, 1.232595164407830946E-32 ) ) ;
#15764 = DIRECTION ( 'NONE',  ( -1.000000000000000000, -0.000000000000000000, -0.000000000000000000 ) ) ;
#15765 = ORIENTED_EDGE ( 'NONE', *, *, #12117, .T. ) ;
#15766 = VERTEX_POINT ( 'NONE', #32330 ) ;
#15767 = SHAPE_REPRESENTATION ( 'chainlinkage2', ( #28566 ), #8124 ) ;
#15768 = DIRECTION ( 'NONE',  ( 0.000000000000000000, 1.000000000000000000, 0.000000000000000000 ) ) ;
#15769 = DIRECTION ( 'NONE',  ( 1.000000000000000000, 0.000000000000000000, -1.232595164407831220E-32 ) ) ;
#15770 = DIRECTION ( 'NONE',  ( 0.000000000000000000, 0.000000000000000000, 1.000000000000000000 ) ) ;
#15771 = DIRECTION ( 'NONE',  ( 1.000000000000000000, 0.000000000000000000, 0.000000000000000000 ) ) ;
#15772 = DIRECTION ( 'NONE',  ( 0.000000000000000000, 0.000000000000000000, -1.000000000000000000 ) ) ;
#15773 = ORIENTED_EDGE ( 'NONE', *, *, #18038, .T. ) ;
#15774 = LINE ( 'NONE', #26254, #7095 ) ;
#15775 = PLANE ( 'NONE',  #19294 ) ;
#15776 = ORIENTED_EDGE ( 'NONE', *, *, #15256, .T. ) ;
#15777 = VECTOR ( 'NONE', #32494, 1000.000000000000000 ) ;
#15778 = PLANE ( 'NONE',  #30997 ) ;
#15779 = DIRECTION ( 'NONE',  ( -0.9075754196709575616, -0.4198891015602634891, -0.000000000000000000 ) ) ;
#15780 = PLANE ( 'NONE',  #34514 ) ;
#15781 = VERTEX_POINT ( 'NONE', #5451 ) ;
#15782 = DIRECTION ( 'NONE',  ( 0.000000000000000000, 1.836970198721029441E-16, -1.000000000000000000 ) ) ;
#15783 = ORIENTED_EDGE ( 'NONE', *, *, #16342, .T. ) ;
#15784 = CARTESIAN_POINT ( 'NONE',  ( -442.0000000000000000, -104.9999999999999716, -187.0000000000000000 ) ) ;
#15785 = ORIENTED_EDGE ( 'NONE', *, *, #9863, .T. ) ;
#15786 = B_SPLINE_CURVE_WITH_KNOTS ( 'NONE', 3,
 ( #15961, #27496, #2928, #14164, #7927, #29996 ),
 .UNSPECIFIED., .F., .F.,
 ( 4, 2, 4 ),
 ( 2.036796643443874831E-07, 0.001873401978039412061, 0.003746600276414479517 ),
 .UNSPECIFIED. ) ;
#15788 = CARTESIAN_POINT ( 'NONE',  ( 145.0000000000000568, -97.56119630548165844, -180.0000000000000000 ) ) ;
#15787 = CARTESIAN_POINT ( 'NONE',  ( -449.9999999999999432, -125.0000000000000000, -101.9999999999999858 ) ) ;
#15789 = CYLINDRICAL_SURFACE ( 'NONE', #32438, 3.999999999999976019 ) ;
#15790 = VECTOR ( 'NONE', #7774, 1000.000000000000000 ) ;
#15791 = CIRCLE ( 'NONE', #31661, 34.41491905851385269 ) ;
#15792 = B_SPLINE_CURVE_WITH_KNOTS ( 'NONE', 3,
 ( #21462, #32131, #13107, #10611 ),
 .UNSPECIFIED., .F., .F.,
 ( 4, 4 ),
 ( 0.001749480761540356689, 0.003748098735642882602 ),
 .UNSPECIFIED. ) ;
#15793 = ORIENTED_EDGE ( 'NONE', *, *, #8259, .T. ) ;
#15794 = APPLICATION_CONTEXT ( 'automotive_design' ) ;
#15795 = CARTESIAN_POINT ( 'NONE',  ( 35.44043929807611448, -12.65143121711728291, 10.00000000000000000 ) ) ;
#15796 = DIRECTION ( 'NONE',  ( -0.000000000000000000, 1.000000000000000000, 0.000000000000000000 ) ) ;
#15797 = ORIENTED_EDGE ( 'NONE', *, *, #7976, .F. ) ;
#15798 = VECTOR ( 'NONE', #32500, 1000.000000000000000 ) ;
#15799 = CARTESIAN_POINT ( 'NONE',  ( 776.0558884506368713, 1158.788928547790647, 1753.598338701303419 ) ) ;
#15800 = EDGE_CURVE ( 'NONE', #4606, #29888, #26821, .T. ) ;
#15801 = ORIENTED_EDGE ( 'NONE', *, *, #14167, .F. ) ;
#15802 = CARTESIAN_POINT ( 'NONE',  ( 110.5486025016846412, -1.510413401456684790, 12.41397948795683526 ) ) ;
#15803 = ORIENTED_EDGE ( 'NONE', *, *, #6080, .T. ) ;
#15804 = CARTESIAN_POINT ( 'NONE',  ( 212.5000000000000000, 0.000000000000000000, 0.000000000000000000 ) ) ;
#15805 = ADVANCED_FACE ( 'NONE', ( #27169 ), #11168, .F. ) ;
#15806 = CARTESIAN_POINT ( 'NONE',  ( -449.9999999999999432, -112.9999999999999858, -174.9999999999999716 ) ) ;
#15807 = EDGE_CURVE ( 'NONE', #30104, #19820, #16607, .T. ) ;
#15808 = AXIS2_PLACEMENT_3D ( 'NONE', #19882, #6320, #17224 ) ;
#15809 = CARTESIAN_POINT ( 'NONE',  ( -99.89370470387717660, -0.3451077285824861729, -7.494041212912380345 ) ) ;
#15810 = CARTESIAN_POINT ( 'NONE',  ( 2.789999999999999147, 0.000000000000000000, 0.000000000000000000 ) ) ;
#15811 = EDGE_LOOP ( 'NONE', ( #9670, #24743, #18620, #31310, #19298, #33459, #14497, #20940 ) ) ;
#15812 = ORIENTED_EDGE ( 'NONE', *, *, #12670, .F. ) ;
#15813 = ORIENTED_EDGE ( 'NONE', *, *, #18741, .F. ) ;
#15814 = CARTESIAN_POINT ( 'NONE',  ( 143.0000000000000568, -12.50000000000001066, 15.00000000000001243 ) ) ;
#15815 = EDGE_CURVE ( 'NONE', #14078, #2690, #1245, .T. ) ;
#15816 = CARTESIAN_POINT ( 'NONE',  ( -37.85301660235036536, 0.7430237821112669616, 15.81122994652406355 ) ) ;
#15817 = CYLINDRICAL_SURFACE ( 'NONE', #2371, 2.033421858999711951 ) ;
#15818 = CIRCLE ( 'NONE', #20350, 4.000000000000003553 ) ;
#15819 = AXIS2_PLACEMENT_3D ( 'NONE', #30082, #3, #24726 ) ;
#15820 = DIRECTION ( 'NONE',  ( -1.000000000000000000, 0.000000000000000000, 0.000000000000000000 ) ) ;
#15821 = CARTESIAN_POINT ( 'NONE',  ( -70.00000000000000000, 4.559999999999908127, 172.9900000000000091 ) ) ;
#15822 = DIRECTION ( 'NONE',  ( -1.000000000000000000, -0.000000000000000000, -0.000000000000000000 ) ) ;
#15823 = ORIENTED_EDGE ( 'NONE', *, *, #16935, .T. ) ;
#15824 = CARTESIAN_POINT ( 'NONE',  ( -19.99999999999998934, -134.9999999999999716, 162.9999999999999716 ) ) ;
#15825 = EDGE_CURVE ( 'NONE', #17242, #32490, #6837, .T. ) ;
#15826 = CARTESIAN_POINT ( 'NONE',  ( 2.789999999999999147, 30.27116788629744804, -3.198253332533264714 ) ) ;
#15827 = COLOUR_RGB ( '',0.7921568627450980005, 0.8196078431372548767, 0.9333333333333333481 ) ;
#15828 = CARTESIAN_POINT ( 'NONE',  ( -499.9999999999999432, 112.9999999999999574, -194.9999999999999716 ) ) ;
#15829 = ORIENTED_EDGE ( 'NONE', *, *, #3471, .T. ) ;
#15830 = CARTESIAN_POINT ( 'NONE',  ( -12.00000000000001243, 134.9999999999998863, 194.9999999999999716 ) ) ;
#15831 = ORIENTED_EDGE ( 'NONE', *, *, #6165, .F. ) ;
#15832 = CARTESIAN_POINT ( 'NONE',  ( -105.3411554791202036, 5.114806216612618250, -11.40564585725304170 ) ) ;
#15833 = CARTESIAN_POINT ( 'NONE',  ( 0.000000000000000000, 45.00000000000000711, -36.68877005347592757 ) ) ;
#15834 = VECTOR ( 'NONE', #27820, 1000.000000000000000 ) ;
#15835 = ORIENTED_EDGE ( 'NONE', *, *, #27607, .T. ) ;
#15836 = FACE_OUTER_BOUND ( 'NONE', #11940, .T. ) ;
#15837 = CARTESIAN_POINT ( 'NONE',  ( -19.99999999999998934, 124.9999999999999716, 162.9999999999999716 ) ) ;
#15838 = DIRECTION ( 'NONE',  ( 0.000000000000000000, -1.131431318426415506E-52, -1.000000000000000000 ) ) ;
#15839 = ORIENTED_EDGE ( 'NONE', *, *, #7181, .T. ) ;
#15840 = VECTOR ( 'NONE', #4254, 1000.000000000000000 ) ;
#15841 = ORIENTED_EDGE ( 'NONE', *, *, #19614, .T. ) ;
#15842 = CARTESIAN_POINT ( 'NONE',  ( 767.0658476328222832, 1242.809291489245425, 1753.598338701303646 ) ) ;
#15843 =( REPRESENTATION_RELATIONSHIP ('NONE','NONE', #23037, #28231 ) REPRESENTATION_RELATIONSHIP_WITH_TRANSFORMATION ( #27078 )SHAPE_REPRESENTATION_RELATIONSHIP( ) );
#15844 = AXIS2_PLACEMENT_3D ( 'NONE', #35063, #26859, #10678 ) ;
#15845 = ORIENTED_EDGE ( 'NONE', *, *, #26917, .T. ) ;
#15846 = CARTESIAN_POINT ( 'NONE',  ( -8.000000000000001776, 0.000000000000000000, -10.30000000000000071 ) ) ;
#15847 = ADVANCED_FACE ( 'NONE', ( #30192 ), #32857, .T. ) ;
#15848 = CIRCLE ( 'NONE', #3873, 1.649999999999999467 ) ;
#15849 = CARTESIAN_POINT ( 'NONE',  ( -12.00000000000001066, -56.99999999999997868, -175.0000000000000000 ) ) ;
#15850 = CARTESIAN_POINT ( 'NONE',  ( -410.0000000000000568, -137.0000000000000000, -175.0000000000000000 ) ) ;
#15851 = CARTESIAN_POINT ( 'NONE',  ( 100.7152960566303364, -3.833500081834649187, 6.453260708061876905 ) ) ;
#15852 = ORIENTED_EDGE ( 'NONE', *, *, #10167, .T. ) ;
#15853 = EDGE_CURVE ( 'NONE', #11201, #12516, #5205, .T. ) ;
#15854 = FACE_OUTER_BOUND ( 'NONE', #7076, .T. ) ;
#15855 = EDGE_CURVE ( 'NONE', #14675, #15650, #31508, .T. ) ;
#15856 = CIRCLE ( 'NONE', #11295, 7.999999999999979572 ) ;
#15858 = CARTESIAN_POINT ( 'NONE',  ( -12.00000000000001066, 136.9999999999999716, 155.0000000000000000 ) ) ;
#15857 = PLANE ( 'NONE',  #10527 ) ;
#15859 = VECTOR ( 'NONE', #6975, 1000.000000000000000 ) ;
#15860 = EDGE_LOOP ( 'NONE', ( #1465, #21697, #25385, #21208, #14700, #647 ) ) ;
#15861 = ORIENTED_EDGE ( 'NONE', *, *, #17553, .F. ) ;
#15862 = EDGE_CURVE ( 'NONE', #22453, #29721, #8066, .T. ) ;
#15863 = EDGE_CURVE ( 'NONE', #17221, #11449, #32425, .T. ) ;
#15864 = DIRECTION ( 'NONE',  ( 0.000000000000000000, -1.000000000000000000, -2.132064625830773463E-16 ) ) ;
#15865 = ORIENTED_EDGE ( 'NONE', *, *, #15598, .T. ) ;
#15866 = LINE ( 'NONE', #20832, #12496 ) ;
#15867 = CARTESIAN_POINT ( 'NONE',  ( 0.02407890056655695096, -21.56796757982795043, -22.39322359481629476 ) ) ;
#15868 = EDGE_LOOP ( 'NONE', ( #15640, #1464 ) ) ;
#15869=STYLED_ITEM('',(#35254),#10172);
#15870 = CARTESIAN_POINT ( 'NONE',  ( -20.00000000000007461, -109.0000000000000142, -162.9999999999999716 ) ) ;
#15871 = PRODUCT_DEFINITION_SHAPE ( 'NONE', 'NONE',  #35236 ) ;
#15872 = LINE ( 'NONE', #4144, #22880 ) ;
#15873 = ORIENTED_EDGE ( 'NONE', *, *, #1370, .T. ) ;
#15874 = B_SPLINE_CURVE_WITH_KNOTS ( 'NONE', 3,
 ( #14683, #33349, #28539, #8970 ),
 .UNSPECIFIED., .F., .F.,
 ( 4, 4 ),
 ( 0.005298349227682462234, 0.005985217865144625352 ),
 .UNSPECIFIED. ) ;
#15875 = B_SPLINE_CURVE_WITH_KNOTS ( 'NONE', 3,
 ( #6677, #822, #3651, #3995, #25725, #14543 ),
 .UNSPECIFIED., .F., .F.,
 ( 4, 2, 4 ),
 ( 1.991142096567452048E-07, 0.001873397407604851950, 0.003746595701000047206 ),
 .UNSPECIFIED. ) ;
#15876 = DIRECTION ( 'NONE',  ( 0.000000000000000000, 1.836970198721029688E-16, -1.000000000000000000 ) ) ;
#15877 = CARTESIAN_POINT ( 'NONE',  ( -5.021133111224679091, 28.08988295778447508, -67.50000000000000000 ) ) ;
#15878 = ADVANCED_FACE ( 'NONE', ( #11342 ), #479, .F. ) ;
#15879 = CARTESIAN_POINT ( 'NONE',  ( 2.719051661303893752, -27.07192087577324102, 16.48097105307871502 ) ) ;
#15880 = VECTOR ( 'NONE', #8311, 1000.000000000000000 ) ;
#15882 = CARTESIAN_POINT ( 'NONE',  ( -365.0000000000000000, 116.9999999999999858, 126.0000000000000000 ) ) ;
#15881 = PLANE ( 'NONE',  #5952 ) ;
#15883 = CARTESIAN_POINT ( 'NONE',  ( -5.469264258321805627, 1.713938105891546382, -0.7500000000000000000 ) ) ;
#15884 = CARTESIAN_POINT ( 'NONE',  ( -19.99999999999998934, 144.9999999999999716, -162.9999999999999147 ) ) ;
#15885 = FACE_OUTER_BOUND ( 'NONE', #4374, .T. ) ;
#15886 = EDGE_CURVE ( 'NONE', #29470, #8179, #2956, .T. ) ;
#15887 = AXIS2_PLACEMENT_3D ( 'NONE', #18614, #23920, #29625 ) ;
#15888 = ORIENTED_EDGE ( 'NONE', *, *, #3646, .T. ) ;
#15889 = EDGE_CURVE ( 'NONE', #32399, #14788, #27697, .T. ) ;
#15890 = LINE ( 'NONE', #2323, #3482 ) ;
#15891 = CARTESIAN_POINT ( 'NONE',  ( 787.0597240610876497, 1342.348721680644530, 1510.856790487179978 ) ) ;
#15892 = VERTEX_POINT ( 'NONE', #10637 ) ;
#15893 = ORIENTED_EDGE ( 'NONE', *, *, #26629, .T. ) ;
#15894 = VECTOR ( 'NONE', #11504, 1000.000000000000000 ) ;
#15895 = CARTESIAN_POINT ( 'NONE',  ( 110.7380848894536598, 0.3991779689724688773, 7.500000000000000000 ) ) ;
#15896 = CARTESIAN_POINT ( 'NONE',  ( 788.6998024004168428, 1372.775055875512862, 1753.598338701303646 ) ) ;
#15897 = ORIENTED_EDGE ( 'NONE', *, *, #20276, .T. ) ;
#15898 = DIRECTION ( 'NONE',  ( -3.469446951953832974E-18, -1.000000000000000000, -7.888609052210116302E-31 ) ) ;
#15899 = SURFACE_SIDE_STYLE ('',( #29404 ) ) ;
#15900 = TOROIDAL_SURFACE ( 'NONE', #7049, 30.47050528711511674, 8.000000000000000000 ) ;
#15901 = ITEM_DEFINED_TRANSFORMATION ( 'NONE', 'NONE', #16714,  #28566 ) ;
#15902 = CARTESIAN_POINT ( 'NONE',  ( 11.99999999999999645, 134.9999999999998863, 187.0000000000000000 ) ) ;
#15903 = ORIENTED_EDGE ( 'NONE', *, *, #10444, .T. ) ;
#15904 = VERTEX_POINT ( 'NONE', #21489 ) ;
#15905 = EDGE_CURVE ( 'NONE', #24475, #26754, #7950, .T. ) ;
#15906 = EDGE_CURVE ( 'NONE', #18186, #20191, #24315, .T. ) ;
#15907 = CARTESIAN_POINT ( 'NONE',  ( -12.00000000000001066, 104.9999999999999858, -155.0000000000000000 ) ) ;
#15908 = LINE ( 'NONE', #32246, #28882 ) ;
#15909 = CYLINDRICAL_SURFACE ( 'NONE', #13056, 5.115020388170798959 ) ;
#15910 = DIRECTION ( 'NONE',  ( -0.000000000000000000, -1.000000000000000000, -0.000000000000000000 ) ) ;
#15911 = CARTESIAN_POINT ( 'NONE',  ( 2.783107617110828880, 23.98878059851154632, 19.42891868047417958 ) ) ;
#15912 = EDGE_LOOP ( 'NONE', ( #8155, #33149, #24011, #22276 ) ) ;
#15913 = LINE ( 'NONE', #29589, #35089 ) ;
#15914 = PLANE ( 'NONE',  #898 ) ;
#15915 = DIRECTION ( 'NONE',  ( 1.000000000000000000, 0.000000000000000000, 0.000000000000000000 ) ) ;
#15916 = VECTOR ( 'NONE', #21086, 1000.000000000000114 ) ;
#15917 = LINE ( 'NONE', #10561, #16813 ) ;
#15918 = DIRECTION ( 'NONE',  ( 0.000000000000000000, -0.3681245526846723126, -0.9297764858882535677 ) ) ;
#15919 = FACE_OUTER_BOUND ( 'NONE', #28515, .T. ) ;
#15921 = LINE ( 'NONE', #11269, #19665 ) ;
#15920 = DIRECTION ( 'NONE',  ( -1.000000000000000000, -0.000000000000000000, -0.000000000000000000 ) ) ;
#15922 = LINE ( 'NONE', #24068, #11631 ) ;
#15923 = ORIENTED_EDGE ( 'NONE', *, *, #2646, .T. ) ;
#15924 = CARTESIAN_POINT ( 'NONE',  ( -355.0000000000000000, -119.0000000000000000, 126.0000000000000000 ) ) ;
#15926 = DIRECTION ( 'NONE',  ( 0.000000000000000000, -6.123233995736766036E-17, -1.000000000000000000 ) ) ;
#15925 = LINE ( 'NONE', #27102, #13230 ) ;
#15927 = ADVANCED_FACE ( 'NONE', ( #1178 ), #6325, .F. ) ;
#15928 = AXIS2_PLACEMENT_3D ( 'NONE', #14923, #684, #6709 ) ;
#15929 = EDGE_CURVE ( 'NONE', #16123, #31755, #30727, .T. ) ;
#15930 = EDGE_CURVE ( 'NONE', #31987, #4626, #5131, .T. ) ;
#15931 = ORIENTED_EDGE ( 'NONE', *, *, #34474, .T. ) ;
#15932 = DIRECTION ( 'NONE',  ( 0.000000000000000000, 0.000000000000000000, -1.000000000000000000 ) ) ;
#15933 = ADVANCED_FACE ( 'NONE', ( #19709 ), #6684, .F. ) ;
#15934 = VERTEX_POINT ( 'NONE', #28052 ) ;
#15935 = ADVANCED_FACE ( 'NONE', ( #30557 ), #11515, .T. ) ;
#15936 = VERTEX_POINT ( 'NONE', #25018 ) ;
#15937 = DIRECTION ( 'NONE',  ( -1.000000000000000000, 0.000000000000000000, 0.000000000000000000 ) ) ;
#15938 = ORIENTED_EDGE ( 'NONE', *, *, #11713, .F. ) ;
#15939 = EDGE_LOOP ( 'NONE', ( #118, #31664, #2771, #4168 ) ) ;
#15940 = LINE ( 'NONE', #8246, #8218 ) ;
#15941 = FACE_OUTER_BOUND ( 'NONE', #23906, .T. ) ;
#15942 = DIRECTION ( 'NONE',  ( 0.000000000000000000, 1.836970198721029441E-16, -1.000000000000000000 ) ) ;
#15943 = ORIENTED_EDGE ( 'NONE', *, *, #5837, .F. ) ;
#15944 = ORIENTED_EDGE ( 'NONE', *, *, #4343, .F. ) ;
#15945 = CARTESIAN_POINT ( 'NONE',  ( 1.395000000000002238, -2.430610048906255649, 34.32897884578299852 ) ) ;
#15946 = CARTESIAN_POINT ( 'NONE',  ( -37.12776225901827587, -7.411627343331143258, -17.41927665145495041 ) ) ;
#15947 = DIRECTION ( 'NONE',  ( 0.000000000000000000, -0.5000000000000018874, -0.8660254037844374864 ) ) ;
#15948 = ORIENTED_EDGE ( 'NONE', *, *, #2592, .T. ) ;
#15949 = CIRCLE ( 'NONE', #25005, 34.41491905851385269 ) ;
#15950 = LINE ( 'NONE', #21089, #28706 ) ;
#15951 = CARTESIAN_POINT ( 'NONE',  ( -20.63749999999999574, 0.000000000000000000, 0.000000000000000000 ) ) ;
#15952 = ORIENTED_EDGE ( 'NONE', *, *, #26292, .T. ) ;
#15953 = DIRECTION ( 'NONE',  ( 0.000000000000000000, -0.000000000000000000, 1.000000000000000000 ) ) ;
#15954 = DIRECTION ( 'NONE',  ( 1.000000000000000000, 0.000000000000000000, -0.000000000000000000 ) ) ;
#15955 = CYLINDRICAL_SURFACE ( 'NONE', #8932, 7.999999999999986677 ) ;
#15956 = EDGE_LOOP ( 'NONE', ( #23832, #26064, #32243, #2282 ) ) ;
#15957 = CARTESIAN_POINT ( 'NONE',  ( -10.00000000000000000, 3.520859547548641820E-15, 87.50000000000000000 ) ) ;
#15958 = ORIENTED_EDGE ( 'NONE', *, *, #17021, .F. ) ;
#15959 = CARTESIAN_POINT ( 'NONE',  ( -5.021133111224679091, 24.02303923978504940, -67.50000000000000000 ) ) ;
#15960 = VERTEX_POINT ( 'NONE', #31250 ) ;
#15961 = CARTESIAN_POINT ( 'NONE',  ( 2.765921099433443775, -26.45933846664182099, -16.32596387352474565 ) ) ;
#15962 = CARTESIAN_POINT ( 'NONE',  ( -19.99999999999998934, 134.9999999999999432, -186.9999999999999716 ) ) ;
#15963 = EDGE_CURVE ( 'NONE', #15487, #29615, #34781, .T. ) ;
#15964 = EDGE_CURVE ( 'NONE', #19610, #22312, #25029, .T. ) ;
#15965 = EDGE_LOOP ( 'NONE', ( #25370, #5817, #10126, #12329 ) ) ;
#15966 = CARTESIAN_POINT ( 'NONE',  ( -110.1150203881707910, 0.000000000000000000, 57.49999999999999289 ) ) ;
#15967 = DIRECTION ( 'NONE',  ( 0.000000000000000000, -2.225651257388386197E-16, -1.000000000000000000 ) ) ;
#15968 = ORIENTED_EDGE ( 'NONE', *, *, #1055, .F. ) ;
#15969 = AXIS2_PLACEMENT_3D ( 'NONE', #31798, #7406, #2778 ) ;
#15970 = CARTESIAN_POINT ( 'NONE',  ( 769.1404724369333508, 1223.419976964294619, 1753.598338701303419 ) ) ;
#15971 = ORIENTED_EDGE ( 'NONE', *, *, #18373, .T. ) ;
#15972 = CARTESIAN_POINT ( 'NONE',  ( -100.1627706953726005, 1.696271239234545813, 7.312686146626633743 ) ) ;
#15973 = ORIENTED_EDGE ( 'NONE', *, *, #3603, .T. ) ;
#15974 = DIRECTION ( 'NONE',  ( -0.000000000000000000, 1.836970198721029934E-16, -1.000000000000000000 ) ) ;
#15975 = LINE ( 'NONE', #10263, #5606 ) ;
#15976 = CARTESIAN_POINT ( 'NONE',  ( -100.0598114771552929, -1.370240552585038962, -7.381692049079064510 ) ) ;
#15977 = VECTOR ( 'NONE', #23364, 1000.000000000000000 ) ;
#15978 = DIRECTION ( 'NONE',  ( 0.000000000000000000, -1.000000000000000000, 2.225651257388386197E-16 ) ) ;
#15979 = ORIENTED_EDGE ( 'NONE', *, *, #25205, .F. ) ;
#15980 = ORIENTED_EDGE ( 'NONE', *, *, #11984, .T. ) ;
#15981 = VECTOR ( 'NONE', #31100, 1000.000000000000000 ) ;
#15982 = ORIENTED_EDGE ( 'NONE', *, *, #13540, .F. ) ;
#15983 = DIRECTION ( 'NONE',  ( -0.000000000000000000, -0.000000000000000000, -1.000000000000000000 ) ) ;
#15984 = DIRECTION ( 'NONE',  ( 1.000000000000000000, 0.000000000000000000, -0.000000000000000000 ) ) ;
#15985 = DIRECTION ( 'NONE',  ( 0.000000000000000000, 1.000000000000000000, 0.000000000000000000 ) ) ;
#15986 = CYLINDRICAL_SURFACE ( 'NONE', #23057, 16.19999999999999574 ) ;
#15987 = DIRECTION ( 'NONE',  ( 0.000000000000000000, 0.000000000000000000, -1.000000000000000000 ) ) ;
#15988 = DIRECTION ( 'NONE',  ( 1.000000000000000000, 0.000000000000000000, 0.000000000000000000 ) ) ;
#15989 = CARTESIAN_POINT ( 'NONE',  ( -13.53398258527560749, -35.36769364574539765, 68.31122994652405112 ) ) ;
#15990 = EDGE_LOOP ( 'NONE', ( #14925, #331, #20416, #32208 ) ) ;
#15991 = CIRCLE ( 'NONE', #23908, 30.47050528711512030 ) ;
#15992 = CARTESIAN_POINT ( 'NONE',  ( 0.5248941363854600084, 20.67343389904918993, -26.20724806577283061 ) ) ;
#15993 = CARTESIAN_POINT ( 'NONE',  ( -410.0000000000000568, 137.0000000000000000, 154.9999999999999716 ) ) ;
#15994 = CARTESIAN_POINT ( 'NONE',  ( 2.765921099433442443, 28.29688452313417812, -12.88099432405573630 ) ) ;
#15995 = VERTEX_POINT ( 'NONE', #3662 ) ;
#15996 = DIRECTION ( 'NONE',  ( 0.000000000000000000, 1.836970198721029688E-16, -1.000000000000000000 ) ) ;
#15997 = ORIENTED_EDGE ( 'NONE', *, *, #3982, .F. ) ;
#15998 = CARTESIAN_POINT ( 'NONE',  ( -99.88497961182919482, 6.264410040187948829E-16, -12.50000000000000000 ) ) ;
#15999 = EDGE_CURVE ( 'NONE', #17643, #17012, #28530, .T. ) ;
#16000 = FACE_OUTER_BOUND ( 'NONE', #5485, .T. ) ;
#16001 = ADVANCED_FACE ( 'NONE', ( #27870 ), #17228, .T. ) ;
#16003 = EDGE_LOOP ( 'NONE', ( #8771, #4481, #5295, #15223 ) ) ;
#16002 = VECTOR ( 'NONE', #3004, 1000.000000000000000 ) ;
#16004 = LINE ( 'NONE', #26842, #14893 ) ;
#16005 = AXIS2_PLACEMENT_3D ( 'NONE', #10075, #10250, #1373 ) ;
#16006 = FACE_BOUND ( 'NONE', #17913, .T. ) ;
#16008 = CARTESIAN_POINT ( 'NONE',  ( -11.99999999999998224, -145.0000000000000000, 155.0000000000000000 ) ) ;
#16007 = PRODUCT_DEFINITION ( 'UNKNOWN', '', #16149, #4991 ) ;
#16009 = AXIS2_PLACEMENT_3D ( 'NONE', #11971, #25647, #9107 ) ;
#16010 = ORIENTED_EDGE ( 'NONE', *, *, #28775, .F. ) ;
#16011 = VERTEX_POINT ( 'NONE', #1009 ) ;
#16012 = DIRECTION ( 'NONE',  ( -7.893605728314050488E-14, 1.618803117314786135E-15, 0.9999999999999998890 ) ) ;
#16013 = LINE ( 'NONE', #26848, #5310 ) ;
#16014 = AXIS2_PLACEMENT_3D ( 'NONE', #34, #13225, #2868 ) ;
#16015 = VERTEX_POINT ( 'NONE', #20059 ) ;
#16016 = LINE ( 'NONE', #30054, #26583 ) ;
#16017 = VECTOR ( 'NONE', #9830, 1000.000000000000000 ) ;
#16018 = LINE ( 'NONE', #2464, #6744 ) ;
#16019 = DIRECTION ( 'NONE',  ( -1.000000000000000000, 0.000000000000000000, 0.000000000000000000 ) ) ;
#16020 = CARTESIAN_POINT ( 'NONE',  ( 99.88220250681632706, -2.622468385745837072, 7.036045090041716854 ) ) ;
#16021 = ITEM_DEFINED_TRANSFORMATION ( 'NONE', 'NONE', #34848,  #28566 ) ;
#16022 = ORIENTED_EDGE ( 'NONE', *, *, #32930, .T. ) ;
#16023 = CYLINDRICAL_SURFACE ( 'NONE', #16913, 8.000000000000007105 ) ;
#16025 = CARTESIAN_POINT ( 'NONE',  ( 2.606461795830078643, -11.11596589742349295, 30.29626325691701183 ) ) ;
#16024 = DIRECTION ( 'NONE',  ( 0.000000000000000000, -1.836970198721029688E-16, 1.000000000000000000 ) ) ;
#16027 = ORIENTED_EDGE ( 'NONE', *, *, #4049, .F. ) ;
#16026 = CIRCLE ( 'NONE', #23400, 3.999999999999948042 ) ;
#16028 = VERTEX_POINT ( 'NONE', #11880 ) ;
#16029 = DIRECTION ( 'NONE',  ( 0.000000000000000000, 0.000000000000000000, -1.000000000000000000 ) ) ;
#16030 = AXIS2_PLACEMENT_3D ( 'NONE', #28948, #17598, #26101 ) ;
#16031 = ORIENTED_EDGE ( 'NONE', *, *, #2205, .T. ) ;
#16032 = AXIS2_PLACEMENT_3D ( 'NONE', #11857, #11318, #19510 ) ;
#16033 = VECTOR ( 'NONE', #24019, 1000.000000000000000 ) ;
#16034 = DIRECTION ( 'NONE',  ( 0.000000000000000000, 0.000000000000000000, -1.000000000000000000 ) ) ;
#16035 = LINE ( 'NONE', #26869, #14889 ) ;
#16036 = ORIENTED_EDGE ( 'NONE', *, *, #4672, .F. ) ;
#16037 = PLANE ( 'NONE',  #962 ) ;
#16038 = DIRECTION ( 'NONE',  ( 0.000000000000000000, 1.000000000000000000, 0.000000000000000000 ) ) ;
#16039 = EDGE_LOOP ( 'NONE', ( #16459, #19268, #8688, #24721 ) ) ;
#16040 = DIRECTION ( 'NONE',  ( 0.000000000000000000, 0.000000000000000000, 1.000000000000000000 ) ) ;
#16041 = DIRECTION ( 'NONE',  ( 0.000000000000000000, 0.000000000000000000, 1.000000000000000000 ) ) ;
#16042 = EDGE_CURVE ( 'NONE', #20191, #22259, #24461, .T. ) ;
#16043 = AXIS2_PLACEMENT_3D ( 'NONE', #16514, #22188, #27340 ) ;
#16044 = FACE_OUTER_BOUND ( 'NONE', #28763, .T. ) ;
#16045 = CARTESIAN_POINT ( 'NONE',  ( 2.789999999999999147, -5.984944020946091570, 31.37417528048439763 ) ) ;
#16046 =( REPRESENTATION_RELATIONSHIP ('NONE','NONE', #23037, #15767 ) REPRESENTATION_RELATIONSHIP_WITH_TRANSFORMATION ( #1390 )SHAPE_REPRESENTATION_RELATIONSHIP( ) );
#16047 = CARTESIAN_POINT ( 'NONE',  ( 7.699999999999998401, 0.000000000000000000, -16.00000000000000000 ) ) ;
#16048 = CARTESIAN_POINT ( 'NONE',  ( 21.17270648470164218, -7.613573412837960852, 20.00000000000000000 ) ) ;
#16050 = EDGE_CURVE ( 'NONE', #19987, #21251, #16550, .T. ) ;
#16049 = CARTESIAN_POINT ( 'NONE',  ( 1.749999999999999778, 6.183021911001840287, 33.85493898757064812 ) ) ;
#16051 = EDGE_CURVE ( 'NONE', #23168, #32120, #1190, .T. ) ;
#16052 = AXIS2_PLACEMENT_3D ( 'NONE', #8856, #2803, #13850 ) ;
#16053 = ORIENTED_EDGE ( 'NONE', *, *, #25264, .F. ) ;
#16054 = VECTOR ( 'NONE', #17188, 1000.000000000000000 ) ;
#16055 = ADVANCED_FACE ( 'NONE', ( #22550 ), #11696, .T. ) ;
#16056 = EDGE_CURVE ( 'NONE', #27961, #5569, #14899, .T. ) ;
#16057 = CARTESIAN_POINT ( 'NONE',  ( -365.0000000000000000, -114.9999999999999858, 113.9999999999999858 ) ) ;
#16058 = CARTESIAN_POINT ( 'NONE',  ( 827.0597240610711651, 1289.348721680646577, 1505.886119909294621 ) ) ;
#16059 = UNCERTAINTY_MEASURE_WITH_UNIT (LENGTH_MEASURE( 1.000000000000000082E-05 ), #29921, 'distance_accuracy_value', 'NONE');
#16060 = ORIENTED_EDGE ( 'NONE', *, *, #1243, .T. ) ;
#16061 = VERTEX_POINT ( 'NONE', #20235 ) ;
#16062 = EDGE_CURVE ( 'NONE', #31793, #8977, #17697, .T. ) ;
#16063 = CARTESIAN_POINT ( 'NONE',  ( -12.00000000000001066, -105.0000000000000142, 174.9999999999999432 ) ) ;
#16064 = DIRECTION ( 'NONE',  ( 0.3348468428034098165, -0.9422725677130736610, 2.647142942144873083E-15 ) ) ;
#16065 = VERTEX_POINT ( 'NONE', #9882 ) ;
#16066 = LINE ( 'NONE', #31706, #16226 ) ;
#16067 =( NAMED_UNIT ( * ) PLANE_ANGLE_UNIT ( ) SI_UNIT ( $, .RADIAN. ) );
#16068 = CARTESIAN_POINT ( 'NONE',  ( -499.9999999999999432, -105.0000000000000142, -187.0000000000000000 ) ) ;
#16069 = ORIENTED_EDGE ( 'NONE', *, *, #32870, .F. ) ;
#16070 = VERTEX_POINT ( 'NONE', #20749 ) ;
#16071 = CARTESIAN_POINT ( 'NONE',  ( 26.97014235612466493, -26.57093094961043533, 49.43553178847298568 ) ) ;
#16072 = CARTESIAN_POINT ( 'NONE',  ( 2.789999999999999147, 27.60935207499570154, -12.89090262359623118 ) ) ;
#16073 = CARTESIAN_POINT ( 'NONE',  ( 0.000000000000000000, -29.00730259674833178, -9.328884633909240165 ) ) ;
#16074 = CARTESIAN_POINT ( 'NONE',  ( 19.99999999999998934, 136.9999999999999716, 155.0000000000000000 ) ) ;
#16075 = LINE ( 'NONE', #24405, #25079 ) ;
#16076 = ORIENTED_EDGE ( 'NONE', *, *, #4972, .T. ) ;
#16077 = AXIS2_PLACEMENT_3D ( 'NONE', #3685, #7523, #23564 ) ;
#16078 = FACE_BOUND ( 'NONE', #12463, .T. ) ;
#16079 = LINE ( 'NONE', #18225, #29327 ) ;
#16080 = DIRECTION ( 'NONE',  ( 1.000000000000000000, -0.000000000000000000, -0.000000000000000000 ) ) ;
#16081 = AXIS2_PLACEMENT_3D ( 'NONE', #1234, #30780, #6906 ) ;
#16082 = AXIS2_PLACEMENT_3D ( 'NONE', #34598, #25886, #7002 ) ;
#16083 = CIRCLE ( 'NONE', #725, 32.54542015209056416 ) ;
#16084 = CARTESIAN_POINT ( 'NONE',  ( -19.99999999999998934, -145.0000000000000000, -162.9999999999999432 ) ) ;
#16085 = DIRECTION ( 'NONE',  ( 0.000000000000000000, 2.309213040847544338E-50, 1.000000000000000000 ) ) ;
#16087 = CARTESIAN_POINT ( 'NONE',  ( 25.76952721012208158, 19.87802405277947670, 49.43553178847298568 ) ) ;
#16086 = CYLINDRICAL_SURFACE ( 'NONE', #3649, 2.525000000000000799 ) ;
#16088 = DIRECTION ( 'NONE',  ( 1.000000000000000000, 0.000000000000000000, 0.000000000000000000 ) ) ;
#16089 = ORIENTED_EDGE ( 'NONE', *, *, #15351, .T. ) ;
#16090 = CARTESIAN_POINT ( 'NONE',  ( -445.9999999999999432, -104.9999999999999716, -187.0000000000000000 ) ) ;
#16092 = FACE_OUTER_BOUND ( 'NONE', #20750, .T. ) ;
#16091 = DIRECTION ( 'NONE',  ( 0.000000000000000000, 0.000000000000000000, -1.000000000000000000 ) ) ;
#16093 = EDGE_CURVE ( 'NONE', #2574, #23168, #4692, .T. ) ;
#16094 = VERTEX_POINT ( 'NONE', #15071 ) ;
#16095 = EDGE_CURVE ( 'NONE', #5845, #19421, #4015, .T. ) ;
#16096 = EDGE_CURVE ( 'NONE', #13700, #23708, #19947, .T. ) ;
#16097 = CARTESIAN_POINT ( 'NONE',  ( -12.00000000000006573, -145.0000000000000000, -194.9999999999999432 ) ) ;
#16098 = ORIENTED_EDGE ( 'NONE', *, *, #16365, .T. ) ;
#16099 = AXIS2_PLACEMENT_3D ( 'NONE', #30794, #14257, #22260 ) ;
#16100 = VECTOR ( 'NONE', #14908, 1000.000000000000000 ) ;
#16101 = VECTOR ( 'NONE', #27412, 1000.000000000000000 ) ;
#16102 = VECTOR ( 'NONE', #23044, 1000.000000000000000 ) ;
#16103 = ORIENTED_EDGE ( 'NONE', *, *, #27361, .T. ) ;
#16104 = DIRECTION ( 'NONE',  ( -0.000000000000000000, -1.836970198721029688E-16, 1.000000000000000000 ) ) ;
#16105 = ORIENTED_EDGE ( 'NONE', *, *, #634, .F. ) ;
#16106 = ORIENTED_EDGE ( 'NONE', *, *, #32984, .T. ) ;
#16107 = CARTESIAN_POINT ( 'NONE',  ( 2.783084753007022627, 27.98916443103619045, -12.86217335695007868 ) ) ;
#16108 = EDGE_CURVE ( 'NONE', #29515, #30502, #29023, .T. ) ;
#16109 = CYLINDRICAL_SURFACE ( 'NONE', #30014, 5.115020388170798959 ) ;
#16110 = CARTESIAN_POINT ( 'NONE',  ( -12.00000000000001066, -112.9999999999999858, 174.9999999999999432 ) ) ;
#16111 = ORIENTED_EDGE ( 'NONE', *, *, #31700, .F. ) ;
#16112 = ORIENTED_EDGE ( 'NONE', *, *, #11590, .T. ) ;
#16113 = DIRECTION ( 'NONE',  ( 0.000000000000000000, 1.000000000000000000, -3.421138828918010427E-49 ) ) ;
#16114 = CARTESIAN_POINT ( 'NONE',  ( -418.0000000000000568, 104.9999999999999858, -155.0000000000000000 ) ) ;
#16115 = EDGE_CURVE ( 'NONE', #34702, #31399, #12923, .T. ) ;
#16116 = DIRECTION ( 'NONE',  ( 1.000000000000000000, 0.000000000000000000, 0.000000000000000000 ) ) ;
#16117 = DIRECTION ( 'NONE',  ( -0.000000000000000000, 0.5288966977476834419, -0.8486862100397269959 ) ) ;
#16118 = ORIENTED_EDGE ( 'NONE', *, *, #5135, .F. ) ;
#16119 = EDGE_CURVE ( 'NONE', #9803, #8292, #13687, .T. ) ;
#16120 = DIRECTION ( 'NONE',  ( 0.2149704402110236556, 0.9766205557100866574, -0.000000000000000000 ) ) ;
#16121 = CIRCLE ( 'NONE', #13821, 8.000000000000007105 ) ;
#16122 = FACE_OUTER_BOUND ( 'NONE', #25800, .T. ) ;
#16123 = VERTEX_POINT ( 'NONE', #4354 ) ;
#16124 = DIRECTION ( 'NONE',  ( 1.000000000000000000, 3.469446951953834515E-18, 0.000000000000000000 ) ) ;
#16125 = EDGE_CURVE ( 'NONE', #26960, #15297, #5709, .T. ) ;
#16126 = LINE ( 'NONE', #27134, #23430 ) ;
#16127 = CARTESIAN_POINT ( 'NONE',  ( -445.9999999999999432, 105.0000000000000142, 107.9999999999999858 ) ) ;
#16128 = ORIENTED_EDGE ( 'NONE', *, *, #25841, .F. ) ;
#16129 = AXIS2_PLACEMENT_3D ( 'NONE', #506, #9039, #8509 ) ;
#16130 = CARTESIAN_POINT ( 'NONE',  ( -6.500000000000000000, 0.000000000000000000, 4.679999999999999716 ) ) ;
#16131 = ORIENTED_EDGE ( 'NONE', *, *, #15668, .F. ) ;
#16132 = AXIS2_PLACEMENT_3D ( 'NONE', #11432, #19976, #30826 ) ;
#16133 = DIRECTION ( 'NONE',  ( 0.000000000000000000, -1.000000000000000000, -1.836970198721029441E-16 ) ) ;
#16134 = VERTEX_POINT ( 'NONE', #31593 ) ;
#16136 = SURFACE_STYLE_FILL_AREA ( #30343 ) ;
#16135 = CARTESIAN_POINT ( 'NONE',  ( -70.00000000000000000, 75.55999999999990280, 168.2400000000000091 ) ) ;
#16137 = CARTESIAN_POINT ( 'NONE',  ( 0.02407890056655738464, -11.07880054387200985, -29.04985141099774637 ) ) ;
#16138 = ORIENTED_EDGE ( 'NONE', *, *, #18289, .F. ) ;
#16139 = EDGE_CURVE ( 'NONE', #17480, #33119, #17139, .T. ) ;
#16140 = LINE ( 'NONE', #5594, #30209 ) ;
#16141 = CARTESIAN_POINT ( 'NONE',  ( 2.765921099433442887, -8.112136323389137260, 30.01377904834206589 ) ) ;
#16142 = VERTEX_POINT ( 'NONE', #15413 ) ;
#16143 = VECTOR ( 'NONE', #3164, 1000.000000000000000 ) ;
#16144 = ORIENTED_EDGE ( 'NONE', *, *, #15077, .F. ) ;
#16145 = CARTESIAN_POINT ( 'NONE',  ( -20.00000000000007461, 108.9999999999999858, -187.0000000000000000 ) ) ;
#16146 = CARTESIAN_POINT ( 'NONE',  ( 12.00000000000001066, 104.9999999999999858, 155.0000000000000000 ) ) ;
#16147 = ORIENTED_EDGE ( 'NONE', *, *, #30836, .F. ) ;
#16148 = LINE ( 'NONE', #15618, #30943 ) ;
#16149 = PRODUCT_DEFINITION_FORMATION_WITH_SPECIFIED_SOURCE ( 'ANY', '', #22877, .NOT_KNOWN. ) ;
#16150 = AXIS2_PLACEMENT_3D ( 'NONE', #26924, #22122, #8412 ) ;
#16151 = CARTESIAN_POINT ( 'NONE',  ( -109.1385531136273670, -3.010446655309096720, -6.870869395578498739 ) ) ;
#16152 = DIRECTION ( 'NONE',  ( -1.000000000000000000, 0.000000000000000000, 1.848892746611746966E-32 ) ) ;
#16153 = EDGE_LOOP ( 'NONE', ( #24360, #10247, #15705, #5906 ) ) ;
#16154 = ORIENTED_EDGE ( 'NONE', *, *, #17416, .T. ) ;
#16155 = AXIS2_PLACEMENT_3D ( 'NONE', #31142, #17984, #14952 ) ;
#16156 = PRODUCT_DEFINITION_SHAPE ( 'NONE', 'NONE',  #35231 ) ;
#16157 = ORIENTED_EDGE ( 'NONE', *, *, #20566, .F. ) ;
#16158 = DIRECTION ( 'NONE',  ( 0.000000000000000000, 0.000000000000000000, -1.000000000000000000 ) ) ;
#16159 = PLANE ( 'NONE',  #10086 ) ;
#16160 = DIRECTION ( 'NONE',  ( -3.040835319149746090E-31, -1.000000000000000000, 0.000000000000000000 ) ) ;
#16161 = ADVANCED_FACE ( 'NONE', ( #23589 ), #10062, .F. ) ;
#16162 = EDGE_CURVE ( 'NONE', #2097, #32385, #31423, .T. ) ;
#16163 = CARTESIAN_POINT ( 'NONE',  ( 2.789999999999999147, 30.27116788629744804, -3.198253332533264714 ) ) ;
#16164 = CARTESIAN_POINT ( 'NONE',  ( 2.719051666187956684, 4.557485336350932670, -31.36463980626626835 ) ) ;
#16165 = CARTESIAN_POINT ( 'NONE',  ( -349.0000000000000000, 124.9999999999999432, 183.0000000000000000 ) ) ;
#16166 = DIRECTION ( 'NONE',  ( 1.000000000000000000, 0.000000000000000000, 0.000000000000000000 ) ) ;
#16167 = EDGE_LOOP ( 'NONE', ( #29325, #10992, #33731, #5598 ) ) ;
#16168 = CARTESIAN_POINT ( 'NONE',  ( 0.07098928307139744376, 19.10423307544374438, -25.28978101402028145 ) ) ;
#16169 = CARTESIAN_POINT ( 'NONE',  ( 32.30227131129396412, -3.970848902647434286, 49.43553178847298568 ) ) ;
#16170 = DIRECTION ( 'NONE',  ( -1.000000000000000000, 0.000000000000000000, 0.000000000000000000 ) ) ;
#16171 = ORIENTED_EDGE ( 'NONE', *, *, #7704, .T. ) ;
#16172 = CIRCLE ( 'NONE', #248, 3.999999999999976019 ) ;
#16173 = EDGE_CURVE ( 'NONE', #2443, #7332, #32116, .T. ) ;
#16174 = DIRECTION ( 'NONE',  ( 1.000000000000000000, 0.000000000000000000, 0.000000000000000000 ) ) ;
#16175 = ORIENTED_EDGE ( 'NONE', *, *, #21401, .T. ) ;
#16176 = AXIS2_PLACEMENT_3D ( 'NONE', #11601, #14633, #22451 ) ;
#16177 = CARTESIAN_POINT ( 'NONE',  ( 0.000000000000000000, 17.98401995359670025, -24.59729088254937324 ) ) ;
#16178 = CARTESIAN_POINT ( 'NONE',  ( 5.021133111224369117, -5.758675521474011738, -87.50000000000000000 ) ) ;
#16179 = ORIENTED_EDGE ( 'NONE', *, *, #26034, .T. ) ;
#16180 = VECTOR ( 'NONE', #16798, 1000.000000000000000 ) ;
#16181 = ORIENTED_EDGE ( 'NONE', *, *, #18732, .F. ) ;
#16182 = VECTOR ( 'NONE', #20500, 1000.000000000000000 ) ;
#16183 = LINE ( 'NONE', #32878, #4628 ) ;
#16184 = DIRECTION ( 'NONE',  ( 0.000000000000000000, 0.000000000000000000, 1.000000000000000000 ) ) ;
#16185 = DIRECTION ( 'NONE',  ( 0.000000000000000000, 0.000000000000000000, -1.000000000000000000 ) ) ;
#16186 = AXIS2_PLACEMENT_3D ( 'NONE', #243, #13772, #16279 ) ;
#16187 = ORIENTED_EDGE ( 'NONE', *, *, #4357, .F. ) ;
#16188 = ORIENTED_EDGE ( 'NONE', *, *, #14033, .T. ) ;
#16189 = CARTESIAN_POINT ( 'NONE',  ( 814.5192040175139709, 1355.555863292066988, 1753.598338701303874 ) ) ;
#16190 = LINE ( 'NONE', #3513, #33734 ) ;
#16191 = EDGE_CURVE ( 'NONE', #14883, #6316, #31312, .T. ) ;
#16192 = ORIENTED_EDGE ( 'NONE', *, *, #4198, .T. ) ;
#16193 = DIRECTION ( 'NONE',  ( -1.000000000000000000, 0.000000000000000000, 1.232595164407831220E-32 ) ) ;
#16194 = FACE_OUTER_BOUND ( 'NONE', #25084, .T. ) ;
#16195 = AXIS2_PLACEMENT_3D ( 'NONE', #15058, #25900, #28221 ) ;
#16196 = CARTESIAN_POINT ( 'NONE',  ( 0.000000000000000000, 3.524919873834583163E-15, 68.31122994652405112 ) ) ;
#16197 = CARTESIAN_POINT ( 'NONE',  ( -102.4122856152638406, -4.424201595130935694, 6.060139114165001395 ) ) ;
#16198 = ORIENTED_EDGE ( 'NONE', *, *, #2202, .F. ) ;
#16199 = ORIENTED_EDGE ( 'NONE', *, *, #27408, .T. ) ;
#16200 = CARTESIAN_POINT ( 'NONE',  ( 10.00000000000000000, -7.794228634059966687, -13.49999999999999822 ) ) ;
#16201 = VECTOR ( 'NONE', #25420, 1000.000000000000000 ) ;
#16202 = EDGE_CURVE ( 'NONE', #13771, #7322, #21074, .T. ) ;
#16203 = CARTESIAN_POINT ( 'NONE',  ( -107.5838244394680032, 4.417479313406522223, 6.061799023038634715 ) ) ;
#16204 = EDGE_CURVE ( 'NONE', #33378, #11423, #15991, .T. ) ;
#16205 = ADVANCED_FACE ( 'NONE', ( #1865 ), #2048, .T. ) ;
#16207 = CARTESIAN_POINT ( 'NONE',  ( -99.88497961182919482, 6.264093345946822590E-16, -57.49999999999999289 ) ) ;
#16206 = CARTESIAN_POINT ( 'NONE',  ( 0.000000000000000000, 0.000000000000000000, 20.00000000000000000 ) ) ;
#16208 = CIRCLE ( 'NONE', #15619, 30.47050528711511674 ) ;
#16209 = VERTEX_POINT ( 'NONE', #7198 ) ;
#16210 = VERTEX_POINT ( 'NONE', #34622 ) ;
#16211 = AXIS2_PLACEMENT_3D ( 'NONE', #5155, #32748, #27411 ) ;
#16212 = DIRECTION ( 'NONE',  ( 1.000000000000000000, -0.000000000000000000, -0.000000000000000000 ) ) ;
#16213 = EDGE_LOOP ( 'NONE', ( #19863, #3185, #27201, #18533 ) ) ;
#16214 = VECTOR ( 'NONE', #11908, 1000.000000000000000 ) ;
#16215 = CARTESIAN_POINT ( 'NONE',  ( -349.0000000000000000, -125.0000000000000284, 181.0000000000000000 ) ) ;
#16216 = DIRECTION ( 'NONE',  ( 1.000000000000000000, 0.000000000000000000, 0.000000000000000000 ) ) ;
#16217 = EDGE_LOOP ( 'NONE', ( #14259, #34617, #25995, #3887, #20465, #22510, #14510, #17171 ) ) ;
#16218 = ORIENTED_EDGE ( 'NONE', *, *, #24293, .T. ) ;
#16219 = DIRECTION ( 'NONE',  ( 0.000000000000000000, 0.000000000000000000, 1.000000000000000000 ) ) ;
#16220 = CARTESIAN_POINT ( 'NONE',  ( -500.0000000000000000, -145.0000000000000000, -155.0000000000000000 ) ) ;
#16221 = VERTEX_POINT ( 'NONE', #21087 ) ;
#16222 = CARTESIAN_POINT ( 'NONE',  ( 19.99999999999998934, 4.559999999999908127, 172.9900000000000091 ) ) ;
#16223 = DIRECTION ( 'NONE',  ( 1.000000000000000000, 0.000000000000000000, 0.000000000000000000 ) ) ;
#16224 = CARTESIAN_POINT ( 'NONE',  ( 11.99999999999999645, -124.9999999999999432, -194.9999999999999432 ) ) ;
#16225 = CARTESIAN_POINT ( 'NONE',  ( -15.99999999999998579, -32.99999999999997158, 154.9999999999999716 ) ) ;
#16226 = VECTOR ( 'NONE', #10719, 1000.000000000000000 ) ;
#16227 = CARTESIAN_POINT ( 'NONE',  ( 0.02407890056441847060, -0.3931553186915530129, 31.08824725498900321 ) ) ;
#16228 = DIRECTION ( 'NONE',  ( 0.000000000000000000, 0.000000000000000000, 1.000000000000000000 ) ) ;
#16229 = CARTESIAN_POINT ( 'NONE',  ( 1.749999999999999778, 34.17636915695680244, 4.045051921974837761 ) ) ;
#16230 = AXIS2_PLACEMENT_3D ( 'NONE', #14010, #14373, #25198 ) ;
#16231 = ORIENTED_EDGE ( 'NONE', *, *, #31224, .F. ) ;
#16233 = VECTOR ( 'NONE', #16532, 1000.000000000000000 ) ;
#16232 = DIRECTION ( 'NONE',  ( 0.000000000000000000, 0.000000000000000000, 1.000000000000000000 ) ) ;
#16234 = DIRECTION ( 'NONE',  ( -1.047444401652940007E-14, 1.000000000000000000, 6.982962677686266711E-15 ) ) ;
#16235 = VERTEX_POINT ( 'NONE', #7547 ) ;
#16236 = COLOUR_RGB ( '',0.7921568627450980005, 0.8196078431372548767, 0.9333333333333333481 ) ;
#16237 = ORIENTED_EDGE ( 'NONE', *, *, #3516, .F. ) ;
#16238 = CARTESIAN_POINT ( 'NONE',  ( -8.267476927982267298, 31.47782073335737962, -36.68877005347593467 ) ) ;
#16239 = SHAPE_DEFINITION_REPRESENTATION ( #33659, #30518 ) ;
#16240 = EDGE_CURVE ( 'NONE', #7312, #493, #18438, .T. ) ;
#16241 = ORIENTED_EDGE ( 'NONE', *, *, #17986, .T. ) ;
#16242 = LINE ( 'NONE', #21916, #13951 ) ;
#16243 = CARTESIAN_POINT ( 'NONE',  ( -418.0000000000000000, -145.0000000000000000, 155.0000000000000000 ) ) ;
#16244 = ADVANCED_FACE ( 'NONE', ( #2220 ), #30739, .T. ) ;
#16245 = VECTOR ( 'NONE', #8827, 1000.000000000000000 ) ;
#16246 = ADVANCED_FACE ( 'NONE', ( #34984 ), #19311, .T. ) ;
#16247 = DIRECTION ( 'NONE',  ( 0.000000000000000000, -1.000000000000000000, -5.053935297177146739E-49 ) ) ;
#16248 = VERTEX_POINT ( 'NONE', #21617 ) ;
#16249 = ORIENTED_EDGE ( 'NONE', *, *, #22022, .F. ) ;
#16250 = DIRECTION ( 'NONE',  ( 0.7259954919231307313, 0.6876994588534234287, -0.000000000000000000 ) ) ;
#16251 = DIRECTION ( 'NONE',  ( -0.000000000000000000, 1.000000000000000000, -0.000000000000000000 ) ) ;
#16252 = EDGE_CURVE ( 'NONE', #4259, #1639, #32457, .T. ) ;
#16253 = VECTOR ( 'NONE', #21446, 1000.000000000000000 ) ;
#16254 = DIRECTION ( 'NONE',  ( 0.000000000000000000, 0.000000000000000000, 1.000000000000000000 ) ) ;
#16255 = CARTESIAN_POINT ( 'NONE',  ( 0.7561992253044003132, 14.91862693714140242, 30.45773629169372398 ) ) ;
#16256 = DIRECTION ( 'NONE',  ( -0.4684084406997900407, 0.8835120444460229372, 1.622985295858433783E-16 ) ) ;
#16257 = VERTEX_POINT ( 'NONE', #2741 ) ;
#16258 = FACE_BOUND ( 'NONE', #15748, .T. ) ;
#16259 = LINE ( 'NONE', #24409, #27054 ) ;
#16260 = CARTESIAN_POINT ( 'NONE',  ( 2.261199765031106867, -17.23487904370277235, 28.59786932736725618 ) ) ;
#16261 = VECTOR ( 'NONE', #5024, 1000.000000000000000 ) ;
#16262 = CARTESIAN_POINT ( 'NONE',  ( -418.0000000000000000, -109.0000000000000142, -174.9999999999999716 ) ) ;
#16263 = PRESENTATION_STYLE_ASSIGNMENT (( #18759 ) ) ;
#16264 = EDGE_CURVE ( 'NONE', #2759, #3106, #10281, .T. ) ;
#16265 = CARTESIAN_POINT ( 'NONE',  ( 10.00000000000000000, -7.794228634059937377, 13.50000000000000000 ) ) ;
#16267 = DIRECTION ( 'NONE',  ( -0.000000000000000000, -0.000000000000000000, -1.000000000000000000 ) ) ;
#16266 = DIRECTION ( 'NONE',  ( 0.000000000000000000, 1.836970198721029441E-16, -1.000000000000000000 ) ) ;
#16268 = CARTESIAN_POINT ( 'NONE',  ( 37.71145559917817280, 3.353962854566119756, 68.31122994652405112 ) ) ;
#16269 = EDGE_LOOP ( 'NONE', ( #22716, #22583, #14892, #5252 ) ) ;
#16270 = DIRECTION ( 'NONE',  ( -1.000000000000000000, -0.000000000000000000, -0.000000000000000000 ) ) ;
#16272 = CARTESIAN_POINT ( 'NONE',  ( 15.99999999999998579, -115.0000000000000000, -155.0000000000000284 ) ) ;
#16271 = DIRECTION ( 'NONE',  ( 0.000000000000000000, 0.000000000000000000, 1.000000000000000000 ) ) ;
#16273 = AXIS2_PLACEMENT_3D ( 'NONE', #14499, #27477, #19663 ) ;
#16274 = VERTEX_POINT ( 'NONE', #18959 ) ;
#16275 = CARTESIAN_POINT ( 'NONE',  ( 35.63428259149704758, -12.79065496477508823, 49.43553178847298568 ) ) ;
#16276 = CIRCLE ( 'NONE', #8891, 30.47050528711512030 ) ;
#16277 = ORIENTED_EDGE ( 'NONE', *, *, #22748, .T. ) ;
#16278 = ORIENTED_EDGE ( 'NONE', *, *, #28453, .T. ) ;
#16279 = DIRECTION ( 'NONE',  ( 0.000000000000000000, -1.836970198721029688E-16, 1.000000000000000000 ) ) ;
#16280 = VERTEX_POINT ( 'NONE', #437 ) ;
#16281 = EDGE_LOOP ( 'NONE', ( #3302, #18260, #30886, #22233, #29627, #3509, #6583 ) ) ;
#16282 = DIRECTION ( 'NONE',  ( 1.000000000000000000, 0.000000000000000000, -0.000000000000000000 ) ) ;
#16283 = AXIS2_PLACEMENT_3D ( 'NONE', #32132, #31949, #20936 ) ;
#16284 = CIRCLE ( 'NONE', #26482, 3.999999999999976019 ) ;
#16285 = DIRECTION ( 'NONE',  ( -1.000000000000000000, 0.000000000000000000, 0.000000000000000000 ) ) ;
#16286 = DIRECTION ( 'NONE',  ( 0.000000000000000000, 2.309213040847544338E-50, 1.000000000000000000 ) ) ;
#16287 = CIRCLE ( 'NONE', #3182, 32.54542015209054995 ) ;
#16288 = VERTEX_POINT ( 'NONE', #29802 ) ;
#16289 = ORIENTED_EDGE ( 'NONE', *, *, #8899, .F. ) ;
#16290 = CARTESIAN_POINT ( 'NONE',  ( 5.021133111224265200, -13.65249191622732816, -67.50000000000000000 ) ) ;
#16291 = FILL_AREA_STYLE ('',( #7909 ) ) ;
#16292 = EDGE_CURVE ( 'NONE', #1376, #32413, #30145, .T. ) ;
#16293 = EDGE_CURVE ( 'NONE', #12566, #27067, #5053, .T. ) ;
#16294 = CARTESIAN_POINT ( 'NONE',  ( 99.30126570083648119, -0.7699128213881771821, -12.48180554319666236 ) ) ;
#16295 = DIRECTION ( 'NONE',  ( 1.000000000000000000, 0.000000000000000000, 0.000000000000000000 ) ) ;
#16296 = ORIENTED_EDGE ( 'NONE', *, *, #32344, .T. ) ;
#16297 = AXIS2_PLACEMENT_3D ( 'NONE', #3396, #27434, #33307 ) ;
#16298 = DIRECTION ( 'NONE',  ( 0.000000000000000000, 0.000000000000000000, 1.000000000000000000 ) ) ;
#16299 = EDGE_CURVE ( 'NONE', #15650, #27137, #53, .T. ) ;
#16300 = EDGE_CURVE ( 'NONE', #19582, #8355, #13440, .T. ) ;
#16301 = DIRECTION ( 'NONE',  ( -1.000000000000000000, -0.000000000000000000, -0.000000000000000000 ) ) ;
#16302 = ORIENTED_EDGE ( 'NONE', *, *, #10376, .F. ) ;
#16303 = VECTOR ( 'NONE', #8089, 1000.000000000000000 ) ;
#16304 = DIRECTION ( 'NONE',  ( 1.000000000000000000, 0.000000000000000000, -1.232595164407831220E-32 ) ) ;
#16305 = CARTESIAN_POINT ( 'NONE',  ( 2.789999999999999591, 0.000000000000000000, 0.000000000000000000 ) ) ;
#16306 = LINE ( 'NONE', #16478, #34867 ) ;
#16307 = CARTESIAN_POINT ( 'NONE',  ( -5.469264258321805627, 1.713938105891546382, 3.930000000000000160 ) ) ;
#16308 = ORIENTED_EDGE ( 'NONE', *, *, #9299, .T. ) ;
#16309 = CYLINDRICAL_SURFACE ( 'NONE', #32585, 16.19999999999999929 ) ;
#16310 = EDGE_LOOP ( 'NONE', ( #26834, #4957, #25314, #7054 ) ) ;
#16312 = DIRECTION ( 'NONE',  ( 1.000000000000000000, 0.000000000000000000, 0.000000000000000000 ) ) ;
#16311 = DIRECTION ( 'NONE',  ( 1.000000000000000000, -0.000000000000000000, -0.000000000000000000 ) ) ;
#16314 = MECHANICAL_DESIGN_GEOMETRIC_PRESENTATION_REPRESENTATION (  '', ( #7178 ), #31631 ) ;
#16313 = CARTESIAN_POINT ( 'NONE',  ( 22.10765473302597073, -12.47301499840863848, -87.50000000000000000 ) ) ;
#16315 = ADVANCED_FACE ( 'NONE', ( #22470 ), #19141, .F. ) ;
#16316 = EDGE_LOOP ( 'NONE', ( #7038, #33126, #17094, #6696 ) ) ;
#16317 = DIRECTION ( 'NONE',  ( 0.000000000000000000, 0.000000000000000000, -1.000000000000000000 ) ) ;
#16318 = CARTESIAN_POINT ( 'NONE',  ( -26.18205399241665177, -19.33143609808334418, -36.68877005347593467 ) ) ;
#16319 = CIRCLE ( 'NONE', #10051, 3.999999999999976019 ) ;
#16320 = VERTEX_POINT ( 'NONE', #8439 ) ;
#16321 = ADVANCED_FACE ( 'NONE', ( #24439 ), #21971, .T. ) ;
#16322 = VECTOR ( 'NONE', #32904, 1000.000000000000000 ) ;
#16323 = EDGE_CURVE ( 'NONE', #33860, #5983, #29979, .T. ) ;
#16324 = ORIENTED_EDGE ( 'NONE', *, *, #3450, .T. ) ;
#16325 = CARTESIAN_POINT ( 'NONE',  ( -6.500000000000000000, 0.000000000000000000, -0.7520000000000004459 ) ) ;
#16326 = CARTESIAN_POINT ( 'NONE',  ( -109.9396462212316266, 1.371756618311864795, 7.381329779211299957 ) ) ;
#16327 = ORIENTED_EDGE ( 'NONE', *, *, #24601, .F. ) ;
#16328 = ORIENTED_EDGE ( 'NONE', *, *, #1546, .F. ) ;
#16329 = PLANE ( 'NONE',  #12766 ) ;
#16330 = CARTESIAN_POINT ( 'NONE',  ( 15.99999999999998579, 75.55999999999990280, 177.7400000000000091 ) ) ;
#16331 = CARTESIAN_POINT ( 'NONE',  ( 3.235562306570555532E-30, -11.61907005722761532, -67.50000000000000000 ) ) ;
#16332 = DIRECTION ( 'NONE',  ( 0.000000000000000000, 1.836970198721029441E-16, -1.000000000000000000 ) ) ;
#16333 = ORIENTED_EDGE ( 'NONE', *, *, #3162, .F. ) ;
#16334 = ORIENTED_EDGE ( 'NONE', *, *, #8334, .T. ) ;
#16335 = DIRECTION ( 'NONE',  ( 0.000000000000000000, 0.000000000000000000, 1.000000000000000000 ) ) ;
#16337 = VECTOR ( 'NONE', #8474, 1000.000000000000000 ) ;
#16336 = CARTESIAN_POINT ( 'NONE',  ( -19.99999999999998934, 75.55999999999990280, -177.7400000000000091 ) ) ;
#16338 = CARTESIAN_POINT ( 'NONE',  ( -410.0000000000000568, 105.0000000000000142, 107.9999999999999858 ) ) ;
#16339 = DIRECTION ( 'NONE',  ( 0.000000000000000000, 0.000000000000000000, -1.000000000000000000 ) ) ;
#16340 = CARTESIAN_POINT ( 'NONE',  ( 11.99999999999999645, -115.0000000000000000, 162.9999999999999716 ) ) ;
#16341 = CYLINDRICAL_SURFACE ( 'NONE', #12626, 2.524999999999999467 ) ;
#16342 = EDGE_CURVE ( 'NONE', #21040, #23180, #34157, .T. ) ;
#16343 = EDGE_CURVE ( 'NONE', #31298, #26980, #5743, .T. ) ;
#16344 = FACE_OUTER_BOUND ( 'NONE', #19275, .T. ) ;
#16345 = CARTESIAN_POINT ( 'NONE',  ( 129.3530333899765594, 6.000000000000000000, -62.49999999999999289 ) ) ;
#16346 = ORIENTED_EDGE ( 'NONE', *, *, #4669, .F. ) ;
#16347 = PRESENTATION_LAYER_ASSIGNMENT (  '', '', ( #32229 ) ) ;
#16348 = DIRECTION ( 'NONE',  ( 0.000000000000000000, 0.5000000000000004441, -0.8660254037844382635 ) ) ;
#16349 = DIRECTION ( 'NONE',  ( 0.000000000000000000, -2.309213040847544338E-50, -1.000000000000000000 ) ) ;
#16350 = EDGE_CURVE ( 'NONE', #842, #15934, #19391, .T. ) ;
#16351 = CARTESIAN_POINT ( 'NONE',  ( 0.1396634953578575200, 2.649662288468964011, -13.49999999999999822 ) ) ;
#16352 = VERTEX_POINT ( 'NONE', #27480 ) ;
#16353 = AXIS2_PLACEMENT_3D ( 'NONE', #13576, #24408, #24237 ) ;
#16354 = VECTOR ( 'NONE', #30292, 1000.000000000000000 ) ;
#16355 = DIRECTION ( 'NONE',  ( 0.000000000000000000, 0.000000000000000000, -1.000000000000000000 ) ) ;
#16356 = ORIENTED_EDGE ( 'NONE', *, *, #34112, .F. ) ;
#16357 = CARTESIAN_POINT ( 'NONE',  ( -106.1720655868554530, 4.981785521925212734, -11.46442881298733063 ) ) ;
#16358 = DIRECTION ( 'NONE',  ( -0.000000000000000000, -1.000000000000000000, -0.000000000000000000 ) ) ;
#16359 = VECTOR ( 'NONE', #25194, 1000.000000000000227 ) ;
#16360 = VERTEX_POINT ( 'NONE', #3092 ) ;
#16361 = DIRECTION ( 'NONE',  ( 0.000000000000000000, 0.000000000000000000, 1.000000000000000000 ) ) ;
#16362 = FACE_OUTER_BOUND ( 'NONE', #12081, .T. ) ;
#16363 = CARTESIAN_POINT ( 'NONE',  ( 1.395000000000002238, 32.09669216789253454, -12.41728656686340138 ) ) ;
#16364 = ORIENTED_EDGE ( 'NONE', *, *, #33301, .F. ) ;
#16365 = EDGE_CURVE ( 'NONE', #19238, #769, #21635, .T. ) ;
#16366 = ADVANCED_FACE ( 'NONE', ( #13267 ), #7911, .T. ) ;
#16367 = EDGE_LOOP ( 'NONE', ( #9064, #6563, #19397, #4294 ) ) ;
#16368 = AXIS2_PLACEMENT_3D ( 'NONE', #203, #23917, #19266 ) ;
#16369 = DIRECTION ( 'NONE',  ( 2.631201909438060269E-14, -5.396010391056495992E-16, 0.9999999999999998890 ) ) ;
#16370 = CARTESIAN_POINT ( 'NONE',  ( -6.500000000000000000, 0.000000000000000000, 4.679999999999999716 ) ) ;
#16371 = ORIENTED_EDGE ( 'NONE', *, *, #17468, .T. ) ;
#16372 = DIRECTION ( 'NONE',  ( 0.000000000000000000, 0.000000000000000000, -1.000000000000000000 ) ) ;
#16373 = EDGE_CURVE ( 'NONE', #21039, #20858, #6107, .T. ) ;
#16374 = FACE_OUTER_BOUND ( 'NONE', #34841, .T. ) ;
#16375 = AXIS2_PLACEMENT_3D ( 'NONE', #27202, #16193, #34691 ) ;
#16376 = CIRCLE ( 'NONE', #1020, 3.999999999999982681 ) ;
#16377 = ADVANCED_FACE ( 'NONE', ( #1140 ), #12004, .F. ) ;
#16378 = CARTESIAN_POINT ( 'NONE',  ( -37.58721499952019940, -4.609089608337754385, 68.31122994652405112 ) ) ;
#16379 = DIRECTION ( 'NONE',  ( -1.000000000000000000, 0.000000000000000000, 0.000000000000000000 ) ) ;
#16380 = ORIENTED_EDGE ( 'NONE', *, *, #10497, .T. ) ;
#16381 = VERTEX_POINT ( 'NONE', #30857 ) ;
#16383 = EDGE_CURVE ( 'NONE', #31862, #30622, #13715, .T. ) ;
#16382 = ORIENTED_EDGE ( 'NONE', *, *, #8142, .T. ) ;
#16384 = DIRECTION ( 'NONE',  ( -1.000000000000000000, 0.000000000000000000, 0.000000000000000000 ) ) ;
#16385 = CARTESIAN_POINT ( 'NONE',  ( 2.789999999999998703, 18.19930456030770927, 24.67628137665903054 ) ) ;
#16386 = AXIS2_PLACEMENT_3D ( 'NONE', #34980, #4871, #15770 ) ;
#16387 = CARTESIAN_POINT ( 'NONE',  ( 25.76952721012208158, 19.87802405277947315, 68.31122994652405112 ) ) ;
#16388 = EDGE_LOOP ( 'NONE', ( #2270, #14328, #33048, #9732 ) ) ;
#16389 = ORIENTED_EDGE ( 'NONE', *, *, #3451, .F. ) ;
#16390 = DIRECTION ( 'NONE',  ( -1.000000000000000000, 0.000000000000000000, 0.000000000000000000 ) ) ;
#16391 = EDGE_LOOP ( 'NONE', ( #19337, #30993, #475 ) ) ;
#16392 = FACE_OUTER_BOUND ( 'NONE', #34434, .T. ) ;
#16393 = CYLINDRICAL_SURFACE ( 'NONE', #33047, 4.000000000000003553 ) ;
#16394 = VERTEX_POINT ( 'NONE', #17536 ) ;
#16395 = ORIENTED_EDGE ( 'NONE', *, *, #31183, .T. ) ;
#16396 = CARTESIAN_POINT ( 'NONE',  ( 0.000000000000000000, 9.539392014169456147, 3.000000000000000000 ) ) ;
#16397 = CIRCLE ( 'NONE', #28320, 9.999999999999994671 ) ;
#16398 = DIRECTION ( 'NONE',  ( 0.000000000000000000, 0.000000000000000000, 1.000000000000000000 ) ) ;
#16399 = ORIENTED_EDGE ( 'NONE', *, *, #12799, .T. ) ;
#16400 = CARTESIAN_POINT ( 'NONE',  ( 129.3530333899765594, 6.000000000000000000, -62.49999999999999289 ) ) ;
#16401 = DIRECTION ( 'NONE',  ( 0.000000000000000000, 0.000000000000000000, 1.000000000000000000 ) ) ;
#16402 = CYLINDRICAL_SURFACE ( 'NONE', #14434, 44.99999999999997868 ) ;
#16403 = CARTESIAN_POINT ( 'NONE',  ( 15.99999999999998579, -115.0000000000000142, 162.9999999999999716 ) ) ;
#16404 = AXIS2_PLACEMENT_3D ( 'NONE', #5323, #13365, #27400 ) ;
#16405 = VECTOR ( 'NONE', #17482, 1000.000000000000000 ) ;
#16406 = CARTESIAN_POINT ( 'NONE',  ( 2.789999999999999147, 14.63235270440936731, 27.43224275967444470 ) ) ;
#16407 = DIRECTION ( 'NONE',  ( 0.000000000000000000, 0.000000000000000000, -1.000000000000000000 ) ) ;
#16408 = DIRECTION ( 'NONE',  ( 0.000000000000000000, 1.000000000000000000, -3.374343856708137958E-53 ) ) ;
#16409 = CIRCLE ( 'NONE', #26065, 8.000000000000007105 ) ;
#16410 = EDGE_CURVE ( 'NONE', #22371, #25531, #11838, .T. ) ;
#16411 = ADVANCED_FACE ( 'NONE', ( #3793, #23030 ), #28191, .T. ) ;
#16412 = VERTEX_POINT ( 'NONE', #30513 ) ;
#16413 = CARTESIAN_POINT ( 'NONE',  ( 35.44043929807611448, -32.65143121711728469, 10.00000000000000000 ) ) ;
#16414 = CARTESIAN_POINT ( 'NONE',  ( 787.0597240610716199, 1342.348721680644530, 1680.876119909291219 ) ) ;
#16415 = ORIENTED_EDGE ( 'NONE', *, *, #14773, .T. ) ;
#16416 = ORIENTED_EDGE ( 'NONE', *, *, #1104, .F. ) ;
#16417 = CIRCLE ( 'NONE', #22661, 4.682234377621698584 ) ;
#16418 = CARTESIAN_POINT ( 'NONE',  ( 103.0977060123724698, 5.416883352271473662, 5.187895480218550404 ) ) ;
#16419 = SHAPE_DEFINITION_REPRESENTATION ( #11796, #47 ) ;
#16420 = EDGE_LOOP ( 'NONE', ( #31507, #31502, #9897, #34554, #30344, #4734, #26971, #3976 ) ) ;
#16421 = DIRECTION ( 'NONE',  ( 1.204656189240283493E-16, 0.9836764282395641379, 0.1799463379062031521 ) ) ;
#16422 = CONTEXT_DEPENDENT_SHAPE_REPRESENTATION ( #11733, #5034 ) ;
#16424 = DIRECTION ( 'NONE',  ( 0.000000000000000000, 1.000000000000000000, 0.000000000000000000 ) ) ;
#16423 = CARTESIAN_POINT ( 'NONE',  ( 2.789999999999999147, 7.350529080603541487, 30.20932655202940254 ) ) ;
#16425 = ORIENTED_EDGE ( 'NONE', *, *, #33309, .F. ) ;
#16426 = ORIENTED_EDGE ( 'NONE', *, *, #8957, .T. ) ;
#16427 = CARTESIAN_POINT ( 'NONE',  ( 10.17231796313409298, 6.310691531022070144, -77.50000000000000000 ) ) ;
#16428 = DIRECTION ( 'NONE',  ( 1.000000000000000000, 0.000000000000000000, 0.000000000000000000 ) ) ;
#16429 = FACE_OUTER_BOUND ( 'NONE', #16269, .T. ) ;
#16430 = DIRECTION ( 'NONE',  ( -1.000000000000000000, -0.000000000000000000, -0.000000000000000000 ) ) ;
#16431 = CARTESIAN_POINT ( 'NONE',  ( 2.789999999999999147, 23.53611639059710114, 19.35207786518998319 ) ) ;
#16432 = ORIENTED_EDGE ( 'NONE', *, *, #15122, .F. ) ;
#16433 = VECTOR ( 'NONE', #21659, 1000.000000000000000 ) ;
#16434 = CARTESIAN_POINT ( 'NONE',  ( -36.47450208408277916, 26.16822801941811605, 52.41980080743829973 ) ) ;
#16435 = FACE_OUTER_BOUND ( 'NONE', #35051, .T. ) ;
#16436 = DIRECTION ( 'NONE',  ( -0.000000000000000000, 0.000000000000000000, 1.000000000000000000 ) ) ;
#16437 = CARTESIAN_POINT ( 'NONE',  ( -2.791255079241054649, -37.75727539589166071, 68.31122994652405112 ) ) ;
#16438 = SURFACE_SIDE_STYLE ('',( #16615 ) ) ;
#16439 = CARTESIAN_POINT ( 'NONE',  ( 0.02407890056655868569, -17.95514392185398833, -25.38201125280375692 ) ) ;
#16441 = FACE_OUTER_BOUND ( 'NONE', #14135, .T. ) ;
#16440 = DIRECTION ( 'NONE',  ( 1.000000000000000000, 0.000000000000000000, 0.000000000000000000 ) ) ;
#16442 = AXIS2_PLACEMENT_3D ( 'NONE', #17926, #6849, #28751 ) ;
#16443 = CYLINDRICAL_SURFACE ( 'NONE', #5325, 2.033421858999711951 ) ;
#16444 = VERTEX_POINT ( 'NONE', #22852 ) ;
#16445 = CARTESIAN_POINT ( 'NONE',  ( -36.90749871141738936, 3.535880188965249360, 16.10314088816767253 ) ) ;
#16447 = CARTESIAN_POINT ( 'NONE',  ( 110.6869025488327196, -0.7897130297925551989, -7.460902677354920520 ) ) ;
#16446 = CARTESIAN_POINT ( 'NONE',  ( -12.00000000000001066, -28.99999999999999645, 155.0000000000000000 ) ) ;
#16448 = EDGE_CURVE ( 'NONE', #1305, #30793, #33146, .T. ) ;
#16449 = AXIS2_PLACEMENT_3D ( 'NONE', #15060, #10800, #32493 ) ;
#16450 = ADVANCED_FACE ( 'NONE', ( #3615 ), #5928, .T. ) ;
#16451 = ORIENTED_EDGE ( 'NONE', *, *, #18858, .F. ) ;
#16452 = LINE ( 'NONE', #16275, #19474 ) ;
#16453 = EDGE_CURVE ( 'NONE', #28489, #24869, #12184, .T. ) ;
#16454 = VERTEX_POINT ( 'NONE', #33168 ) ;
#16455 = AXIS2_PLACEMENT_3D ( 'NONE', #7552, #32292, #29285 ) ;
#16456 = VERTEX_POINT ( 'NONE', #33523 ) ;
#16457 = LINE ( 'NONE', #32275, #8205 ) ;
#16458 = ORIENTED_EDGE ( 'NONE', *, *, #16564, .F. ) ;
#16459 = ORIENTED_EDGE ( 'NONE', *, *, #29849, .T. ) ;
#16460 = CARTESIAN_POINT ( 'NONE',  ( 2.783128927722727575, 20.89672672271989029, 22.72123193261248630 ) ) ;
#16461 = EDGE_CURVE ( 'NONE', #31033, #34772, #3437, .T. ) ;
#16462 = AXIS2_PLACEMENT_3D ( 'NONE', #26773, #18784, #2387 ) ;
#16463 = PLANE ( 'NONE',  #2720 ) ;
#16464 = CARTESIAN_POINT ( 'NONE',  ( 0.000000000000000000, -13.59935610937951900, -28.90010281771846223 ) ) ;
#16465 = ORIENTED_EDGE ( 'NONE', *, *, #2644, .T. ) ;
#16466 = ORIENTED_EDGE ( 'NONE', *, *, #4803, .T. ) ;
#16467 = PLANE ( 'NONE',  #12288 ) ;
#16468 = LINE ( 'NONE', #25150, #27739 ) ;
#16469 = CARTESIAN_POINT ( 'NONE',  ( 109.3101759974547633, -3.792433597769626630, -11.91175651985687622 ) ) ;
#16470 = CARTESIAN_POINT ( 'NONE',  ( 9.199999999999999289, -15.58845726811992627, 0.000000000000000000 ) ) ;
#16471 = EDGE_LOOP ( 'NONE', ( #27776, #10490, #20105, #18180 ) ) ;
#16472 = MECHANICAL_DESIGN_GEOMETRIC_PRESENTATION_REPRESENTATION (  '', ( #30077 ), #2799 ) ;
#16473 = LINE ( 'NONE', #13791, #11141 ) ;
#16474 = DIRECTION ( 'NONE',  ( 0.000000000000000000, 1.836970198721029441E-16, -1.000000000000000000 ) ) ;
#16475 = ORIENTED_EDGE ( 'NONE', *, *, #15451, .F. ) ;
#16476 = CARTESIAN_POINT ( 'NONE',  ( 0.02407890056655781832, 18.59128259035472297, 24.91982945642928016 ) ) ;
#16477 = CARTESIAN_POINT ( 'NONE',  ( 34.58310883014599568, -15.42890216704097206, 68.31122994652405112 ) ) ;
#16478 = CARTESIAN_POINT ( 'NONE',  ( -442.0000000000000000, 141.0000000000000000, -155.0000000000000000 ) ) ;
#16479 = VECTOR ( 'NONE', #8860, 1000.000000000000000 ) ;
#16480 = DIRECTION ( 'NONE',  ( 0.000000000000000000, 0.000000000000000000, -1.000000000000000000 ) ) ;
#16481 = ORIENTED_EDGE ( 'NONE', *, *, #14478, .F. ) ;
#16482 = B_SPLINE_CURVE_WITH_KNOTS ( 'NONE', 3,
 ( #13872, #24712, #22060, #32900, #8522, #30232 ),
 .UNSPECIFIED., .F., .F.,
 ( 4, 2, 4 ),
 ( 4.404817078215036745E-07, 0.001874269662699934880, 0.003748098843692048571 ),
 .UNSPECIFIED. ) ;
#16483 = CARTESIAN_POINT ( 'NONE',  ( -45.00000000000000000, -46.95407462254104303, 36.69637551990492597 ) ) ;
#16484 = ORIENTED_EDGE ( 'NONE', *, *, #21002, .T. ) ;
#16486 = CARTESIAN_POINT ( 'NONE',  ( 2.231373069951498422, 30.82732872002351598, 13.00174666746740293 ) ) ;
#16485 = LINE ( 'NONE', #13801, #10294 ) ;
#16487 = CARTESIAN_POINT ( 'NONE',  ( 2.789999999999999147, 2.005524111408194088, 31.87689292423238996 ) ) ;
#16488 = EDGE_CURVE ( 'NONE', #10620, #25489, #30686, .T. ) ;
#16489 = CIRCLE ( 'NONE', #24331, 4.000000000000003553 ) ;
#16490 = ORIENTED_EDGE ( 'NONE', *, *, #1313, .F. ) ;
#16491 = DIRECTION ( 'NONE',  ( -1.000000000000000000, -0.000000000000000000, -0.000000000000000000 ) ) ;
#16492 = CARTESIAN_POINT ( 'NONE',  ( 2.765921099433442443, -30.46391896562403190, -6.211548095912885259 ) ) ;
#16493 = ADVANCED_FACE ( 'NONE', ( #33882 ), #25154, .T. ) ;
#16494 = EDGE_CURVE ( 'NONE', #19524, #2456, #30324, .T. ) ;
#16495 = ORIENTED_EDGE ( 'NONE', *, *, #2037, .F. ) ;
#16496 = EDGE_CURVE ( 'NONE', #13672, #30715, #14327, .T. ) ;
#16497 = ADVANCED_FACE ( 'NONE', ( #22504, #14146 ), #783, .T. ) ;
#16498 = VERTEX_POINT ( 'NONE', #11653 ) ;
#16499 = DIRECTION ( 'NONE',  ( 1.000000000000000000, 0.000000000000000000, 0.000000000000000000 ) ) ;
#16500 = CARTESIAN_POINT ( 'NONE',  ( 0.000000000000000000, 3.524919873834583163E-15, 68.31122994652405112 ) ) ;
#16501 = EDGE_LOOP ( 'NONE', ( #27535, #11283, #21773, #10005 ) ) ;
#16502 = ORIENTED_EDGE ( 'NONE', *, *, #22, .F. ) ;
#16503 = LINE ( 'NONE', #30179, #21837 ) ;
#16504 = ADVANCED_FACE ( 'NONE', ( #20012, #6459, #15542 ), #20525, .F. ) ;
#16505 = CIRCLE ( 'NONE', #23321, 1.999999999999999112 ) ;
#16506 = DIRECTION ( 'NONE',  ( -0.000000000000000000, -1.836970198721029688E-16, 1.000000000000000000 ) ) ;
#16507 = DIRECTION ( 'NONE',  ( -0.1081190184239421148, 0.9941379571543595972, -0.000000000000000000 ) ) ;
#16508 = FACE_OUTER_BOUND ( 'NONE', #10556, .T. ) ;
#16509 = ORIENTED_EDGE ( 'NONE', *, *, #30636, .T. ) ;
#16510 = ORIENTED_EDGE ( 'NONE', *, *, #9500, .T. ) ;
#16511 = CARTESIAN_POINT ( 'NONE',  ( -143.0000000000000568, -99.56883598056833762, -180.0000000000000000 ) ) ;
#16512 = DIRECTION ( 'NONE',  ( 0.000000000000000000, 0.000000000000000000, -1.000000000000000000 ) ) ;
#16513 = DIRECTION ( 'NONE',  ( 0.6051742151937650194, 0.7960930657056437543, 0.000000000000000000 ) ) ;
#16514 = CARTESIAN_POINT ( 'NONE',  ( -9.410814080250917257, 36.67205378194064735, 68.31122994652405112 ) ) ;
#16515 = CARTESIAN_POINT ( 'NONE',  ( 22.89764159710613001, 4.274639749586562232, -87.50000000000000000 ) ) ;
#16517 = CARTESIAN_POINT ( 'NONE',  ( -144.4704739938196099, -45.49999999999999289, 65.00000000000000000 ) ) ;
#16516 =( REPRESENTATION_RELATIONSHIP ('NONE','NONE', #23037, #28231 ) REPRESENTATION_RELATIONSHIP_WITH_TRANSFORMATION ( #7855 )SHAPE_REPRESENTATION_RELATIONSHIP( ) );
#16518 = CARTESIAN_POINT ( 'NONE',  ( 0.000000000000000000, 2.281310696040539424E-14, -36.68877005347592757 ) ) ;
#16519 = ORIENTED_EDGE ( 'NONE', *, *, #19745, .T. ) ;
#16520 = DIRECTION ( 'NONE',  ( 0.000000000000000000, 0.000000000000000000, -1.000000000000000000 ) ) ;
#16521 = CYLINDRICAL_SURFACE ( 'NONE', #671, 16.19999999999999218 ) ;
#16522 = CARTESIAN_POINT ( 'NONE',  ( -414.0000000000000568, 105.0000000000000142, 187.0000000000000000 ) ) ;
#16523 = ORIENTED_EDGE ( 'NONE', *, *, #29246, .F. ) ;
#16524 = DIRECTION ( 'NONE',  ( 0.000000000000000000, 0.000000000000000000, 1.000000000000000000 ) ) ;
#16525 = VERTEX_POINT ( 'NONE', #20873 ) ;
#16526 = B_SPLINE_CURVE_WITH_KNOTS ( 'NONE', 3,
 ( #33899, #23050, #14702, #25349 ),
 .UNSPECIFIED., .F., .F.,
 ( 4, 4 ),
 ( 2.180635439307156695E-07, 0.0006879539277919046554 ),
 .UNSPECIFIED. ) ;
#16527 = DIRECTION ( 'NONE',  ( 0.000000000000000000, -0.000000000000000000, 1.000000000000000000 ) ) ;
#16528 = CARTESIAN_POINT ( 'NONE',  ( -100.3431920928583736, 2.122570655097208547, -12.31945284403700569 ) ) ;
#16529 = AXIS2_PLACEMENT_3D ( 'NONE', #18997, #24840, #21648 ) ;
#16530 = ORIENTED_EDGE ( 'NONE', *, *, #3369, .T. ) ;
#16531 = CARTESIAN_POINT ( 'NONE',  ( -70.00000000000000000, 75.55999999999990280, -168.2400000000000091 ) ) ;
#16532 = DIRECTION ( 'NONE',  ( 0.000000000000000000, 1.000000000000000000, -3.374343856708137958E-53 ) ) ;
#16533 = CARTESIAN_POINT ( 'NONE',  ( 0.000000000000000000, 17.11426446101236820, -24.44276559937708271 ) ) ;
#16534 = EDGE_LOOP ( 'NONE', ( #5329, #4237, #11301, #11573 ) ) ;
#16535 = ORIENTED_EDGE ( 'NONE', *, *, #240, .T. ) ;
#16536 = CIRCLE ( 'NONE', #18241, 4.682234377621698584 ) ;
#16537 = EDGE_CURVE ( 'NONE', #32615, #26158, #18056, .T. ) ;
#16538 = EDGE_CURVE ( 'NONE', #25782, #26683, #29237, .T. ) ;
#16539 = DIRECTION ( 'NONE',  ( 2.631201909438060585E-14, -5.396010391056496978E-16, 1.000000000000000000 ) ) ;
#16540 = VECTOR ( 'NONE', #34020, 1000.000000000000000 ) ;
#16541 = CARTESIAN_POINT ( 'NONE',  ( 0.1835381793512137760, -32.24848086092538324, 1.209851624881392862 ) ) ;
#16542 = ORIENTED_EDGE ( 'NONE', *, *, #1922, .T. ) ;
#16543 = DIRECTION ( 'NONE',  ( -0.7621620551276372391, 0.6473862847818266930, 0.000000000000000000 ) ) ;
#16544 = SURFACE_STYLE_FILL_AREA ( #29702 ) ;
#16545 = DIRECTION ( 'NONE',  ( -1.232595164407830946E-32, -3.421138828918010427E-49, 1.000000000000000000 ) ) ;
#16546 = CARTESIAN_POINT ( 'NONE',  ( -499.9999999999999432, -141.0000000000000000, -162.9999999999999716 ) ) ;
#16547 = VERTEX_POINT ( 'NONE', #34403 ) ;
#16548 = VERTEX_POINT ( 'NONE', #31720 ) ;
#16549 = ORIENTED_EDGE ( 'NONE', *, *, #10492, .F. ) ;
#16550 = CIRCLE ( 'NONE', #25619, 8.000000000000007105 ) ;
#16551 = CYLINDRICAL_SURFACE ( 'NONE', #20306, 4.000000000000003553 ) ;
#16552 = EDGE_CURVE ( 'NONE', #29888, #34690, #26559, .T. ) ;
#16554 = CIRCLE ( 'NONE', #19394, 7.999999999999979572 ) ;
#16553 = DIRECTION ( 'NONE',  ( 0.000000000000000000, 0.000000000000000000, 1.000000000000000000 ) ) ;
#16555 = CARTESIAN_POINT ( 'NONE',  ( 15.04122381213380599, 28.86114964982168019, 49.43553178847298568 ) ) ;
#16556 = VERTEX_POINT ( 'NONE', #2004 ) ;
#16557 = ORIENTED_EDGE ( 'NONE', *, *, #68, .F. ) ;
#16558 = DIRECTION ( 'NONE',  ( 0.000000000000000000, 0.000000000000000000, -1.000000000000000000 ) ) ;
#16559 = ORIENTED_EDGE ( 'NONE', *, *, #28844, .T. ) ;
#16560 = ADVANCED_FACE ( 'NONE', ( #34579 ), #12522, .T. ) ;
#16561 = FACE_OUTER_BOUND ( 'NONE', #19934, .T. ) ;
#16562 = DIRECTION ( 'NONE',  ( 3.697785493223492838E-32, 1.934419779023891545E-16, -1.000000000000000000 ) ) ;
#16563 = ORIENTED_EDGE ( 'NONE', *, *, #22304, .T. ) ;
#16564 = EDGE_CURVE ( 'NONE', #30135, #24825, #5733, .T. ) ;
#16566 = EDGE_CURVE ( 'NONE', #4415, #14959, #9665, .T. ) ;
#16565 = VERTEX_POINT ( 'NONE', #34048 ) ;
#16567 = CARTESIAN_POINT ( 'NONE',  ( -4.875000000000000000, 2.702098422956710877, -0.7500000000000000000 ) ) ;
#16568 = VECTOR ( 'NONE', #27260, 1000.000000000000000 ) ;
#16569 = CIRCLE ( 'NONE', #26216, 7.999999999999979572 ) ;
#16571 = LINE ( 'NONE', #11572, #30848 ) ;
#16570 = CIRCLE ( 'NONE', #25638, 7.999999999999979572 ) ;
#16572 = ORIENTED_EDGE ( 'NONE', *, *, #8852, .F. ) ;
#16573 = FACE_OUTER_BOUND ( 'NONE', #32992, .T. ) ;
#16574 = CARTESIAN_POINT ( 'NONE',  ( 2.789999999999999147, -5.984944020945660803, -28.84917528048448787 ) ) ;
#16575 = EDGE_CURVE ( 'NONE', #23165, #23630, #21045, .T. ) ;
#16576 = DIRECTION ( 'NONE',  ( -0.000000000000000000, 1.000000000000000000, -0.000000000000000000 ) ) ;
#16577 = CARTESIAN_POINT ( 'NONE',  ( -5.021133111225196011, -25.61315202898006049, -67.50000000000000000 ) ) ;
#16578 = CARTESIAN_POINT ( 'NONE',  ( -500.0000000000000000, -113.0000000000000000, 187.0000000000000000 ) ) ;
#16579 = CARTESIAN_POINT ( 'NONE',  ( 21.24400529595486020, -24.65555945140047811, 49.43553178847298568 ) ) ;
#16580 = DIRECTION ( 'NONE',  ( 0.000000000000000000, 1.131431318426415506E-52, 1.000000000000000000 ) ) ;
#16581 = AXIS2_PLACEMENT_3D ( 'NONE', #4040, #17266, #28622 ) ;
#16582 = EDGE_LOOP ( 'NONE', ( #32092, #18664, #21997, #2248 ) ) ;
#16583 = EDGE_CURVE ( 'NONE', #23102, #31704, #31209, .T. ) ;
#16584 = CARTESIAN_POINT ( 'NONE',  ( 32.30227131129396412, -3.970848902647434286, 49.43553178847298568 ) ) ;
#16585 = DIRECTION ( 'NONE',  ( 2.631201909438060269E-14, -5.396010391056495992E-16, 0.9999999999999998890 ) ) ;
#16586 = ORIENTED_EDGE ( 'NONE', *, *, #29603, .T. ) ;
#16587 = ORIENTED_EDGE ( 'NONE', *, *, #19110, .F. ) ;
#16588 = VECTOR ( 'NONE', #19060, 1000.000000000000000 ) ;
#16589 = CARTESIAN_POINT ( 'NONE',  ( 99.88736582462350100, 2.611822472857947108, 7.032742872185955285 ) ) ;
#16590 = SHAPE_DEFINITION_REPRESENTATION ( #29947, #28231 ) ;
#16591 = AXIS2_PLACEMENT_3D ( 'NONE', #9568, #18285, #12421 ) ;
#16592 = VERTEX_POINT ( 'NONE', #17701 ) ;
#16593 = AXIS2_PLACEMENT_3D ( 'NONE', #21996, #24641, #22527 ) ;
#16594 = CIRCLE ( 'NONE', #1236, 2.525000000000000799 ) ;
#16595 = CARTESIAN_POINT ( 'NONE',  ( -445.9999999999999432, -137.0000000000000000, -175.0000000000000000 ) ) ;
#16597 = CARTESIAN_POINT ( 'NONE',  ( -500.0000000000000000, -113.0000000000000000, 190.9999999999999716 ) ) ;
#16596 = DIRECTION ( 'NONE',  ( -1.000000000000000000, 0.000000000000000000, -0.000000000000000000 ) ) ;
#16598 = ORIENTED_EDGE ( 'NONE', *, *, #32963, .F. ) ;
#16599 = ORIENTED_EDGE ( 'NONE', *, *, #15558, .T. ) ;
#16600 = LINE ( 'NONE', #30642, #4902 ) ;
#16601 = CARTESIAN_POINT ( 'NONE',  ( 11.99999999999999645, 134.9999999999998863, 162.9999999999999716 ) ) ;
#16602 = EDGE_CURVE ( 'NONE', #6498, #1469, #7153, .T. ) ;
#16603 = CARTESIAN_POINT ( 'NONE',  ( -499.9999999999999432, -141.0000000000000000, -187.0000000000000000 ) ) ;
#16604 = DIRECTION ( 'NONE',  ( 0.000000000000000000, 0.000000000000000000, 1.000000000000000000 ) ) ;
#16605 = FACE_OUTER_BOUND ( 'NONE', #30912, .T. ) ;
#16606 = ORIENTED_EDGE ( 'NONE', *, *, #25287, .F. ) ;
#16607 = CIRCLE ( 'NONE', #2290, 12.50000000000000000 ) ;
#16608 = ADVANCED_FACE ( 'NONE', ( #6986 ), #34754, .F. ) ;
#16609 = CARTESIAN_POINT ( 'NONE',  ( 0.000000000000000000, 23.53611639059741378, -19.35207786518964213 ) ) ;
#16610 = FACE_OUTER_BOUND ( 'NONE', #26643, .T. ) ;
#16611 = EDGE_CURVE ( 'NONE', #5255, #13812, #14057, .T. ) ;
#16612 = CARTESIAN_POINT ( 'NONE',  ( 15.04122381213380244, 28.86114964982166597, 68.31122994652405112 ) ) ;
#16613 = PRODUCT ( 'bearing', 'bearing', '', ( #32579 ) ) ;
#16614 = LINE ( 'NONE', #33319, #6096 ) ;
#16615 = SURFACE_STYLE_FILL_AREA ( #3058 ) ;
#16616 = CARTESIAN_POINT ( 'NONE',  ( 143.0000000000000568, -97.49999999999998579, 63.00000000000000000 ) ) ;
#16619 = CARTESIAN_POINT ( 'NONE',  ( -101.6271750261120417, 3.859208454723694892, -6.436243333213718998 ) ) ;
#16618 = PLANE ( 'NONE',  #10503 ) ;
#16617 = VECTOR ( 'NONE', #33631, 1000.000000000000000 ) ;
#16620 = VECTOR ( 'NONE', #12618, 1000.000000000000000 ) ;
#16621 = DIRECTION ( 'NONE',  ( 0.000000000000000000, 0.2486898871648417775, 0.9685831611286344067 ) ) ;
#16622 = ORIENTED_EDGE ( 'NONE', *, *, #22151, .T. ) ;
#16624 = VECTOR ( 'NONE', #3543, 1000.000000000000000 ) ;
#16623 = FACE_OUTER_BOUND ( 'NONE', #17967, .T. ) ;
#16626 = DIRECTION ( 'NONE',  ( 0.000000000000000000, 0.000000000000000000, 1.000000000000000000 ) ) ;
#16625 = SURFACE_STYLE_USAGE ( .BOTH. , #8581 ) ;
#16627 = VERTEX_POINT ( 'NONE', #20362 ) ;
#16628 =( LENGTH_UNIT ( ) NAMED_UNIT ( * ) SI_UNIT ( .MILLI., .METRE. ) );
#16629 = EDGE_LOOP ( 'NONE', ( #5967, #30196, #26164, #30298 ) ) ;
#16630 = ORIENTED_EDGE ( 'NONE', *, *, #13001, .T. ) ;
#16631 = CYLINDRICAL_SURFACE ( 'NONE', #34930, 7.999999999999992895 ) ;
#16632 = ORIENTED_EDGE ( 'NONE', *, *, #10486, .T. ) ;
#16633 = EDGE_LOOP ( 'NONE', ( #15812, #24955, #26626, #270, #27986, #3987, #11525, #680, #14288 ) ) ;
#16634 = DIRECTION ( 'NONE',  ( -0.000000000000000000, 0.08715574274766170471, 0.9961946980917453232 ) ) ;
#16636 = AXIS2_PLACEMENT_3D ( 'NONE', #33241, #17067, #32522 ) ;
#16635 = CONTEXT_DEPENDENT_SHAPE_REPRESENTATION ( #21020, #19985 ) ;
#16637 = LINE ( 'NONE', #22139, #13534 ) ;
#16638 = TOROIDAL_SURFACE ( 'NONE', #2967, 30.47050528711512030, 8.000000000000000000 ) ;
#16639 = CARTESIAN_POINT ( 'NONE',  ( -2.216215597024039141, -32.46987467335852529, 68.31122994652405112 ) ) ;
#16640 = ORIENTED_EDGE ( 'NONE', *, *, #8514, .T. ) ;
#16641 = CIRCLE ( 'NONE', #9257, 2.000000000000001776 ) ;
#16642 = VERTEX_POINT ( 'NONE', #18222 ) ;
#16643 = CARTESIAN_POINT ( 'NONE',  ( -15.00000000000000000, 0.000000000000000000, 20.00000000000000000 ) ) ;
#16644 = DIRECTION ( 'NONE',  ( -1.000000000000000000, -0.000000000000000000, -0.000000000000000000 ) ) ;
#16645 = EDGE_CURVE ( 'NONE', #13606, #32956, #33602, .T. ) ;
#16646 = CARTESIAN_POINT ( 'NONE',  ( 103.4959836398287649, -5.550599894338584583, -11.20035359757824089 ) ) ;
#16647 = DIRECTION ( 'NONE',  ( 0.000000000000000000, 0.000000000000000000, 1.000000000000000000 ) ) ;
#16648 = ORIENTED_EDGE ( 'NONE', *, *, #7608, .F. ) ;
#16649 = EDGE_CURVE ( 'NONE', #30837, #17242, #17878, .T. ) ;
#16650 = CARTESIAN_POINT ( 'NONE',  ( -12.00000000000001066, -145.0000000000000000, 162.9999999999999716 ) ) ;
#16651 = ADVANCED_FACE ( 'NONE', ( #15195 ), #20704, .T. ) ;
#16652 = LINE ( 'NONE', #27835, #26113 ) ;
#16653 = ORIENTED_EDGE ( 'NONE', *, *, #14689, .T. ) ;
#16654 = DIRECTION ( 'NONE',  ( 1.000000000000000000, 0.000000000000000000, 0.000000000000000000 ) ) ;
#16655 = CARTESIAN_POINT ( 'NONE',  ( 11.99999999999999645, 104.9999999999999858, -155.0000000000000000 ) ) ;
#16656 = DIRECTION ( 'NONE',  ( -1.000000000000000000, -0.000000000000000000, -0.000000000000000000 ) ) ;
#16657 = DIRECTION ( 'NONE',  ( 0.000000000000000000, 0.000000000000000000, 1.000000000000000000 ) ) ;
#16658 = ORIENTED_EDGE ( 'NONE', *, *, #27703, .T. ) ;
#16659 = DIRECTION ( 'NONE',  ( -1.000000000000000000, -0.000000000000000000, -0.000000000000000000 ) ) ;
#16660 = ORIENTED_EDGE ( 'NONE', *, *, #17905, .T. ) ;
#16662 =( NAMED_UNIT ( * ) PLANE_ANGLE_UNIT ( ) SI_UNIT ( $, .RADIAN. ) );
#16661 = CYLINDRICAL_SURFACE ( 'NONE', #22244, 34.41491905851385269 ) ;
#16663 = AXIS2_PLACEMENT_3D ( 'NONE', #8377, #30093, #8901 ) ;
#16665 = ORIENTED_EDGE ( 'NONE', *, *, #9871, .T. ) ;
#16664 = VECTOR ( 'NONE', #12807, 1000.000000000000000 ) ;
#16666 = AXIS2_PLACEMENT_3D ( 'NONE', #11097, #25126, #22300 ) ;
#16667 = AXIS2_PLACEMENT_3D ( 'NONE', #7922, #19321, #32991 ) ;
#16668 = CARTESIAN_POINT ( 'NONE',  ( 11.99999999999999645, -124.9999999999999432, -186.9999999999999716 ) ) ;
#16669 = CARTESIAN_POINT ( 'NONE',  ( -12.00000000000001066, -124.9999999999999432, -186.9999999999999716 ) ) ;
#16670 = ORIENTED_EDGE ( 'NONE', *, *, #33309, .T. ) ;
#16671 = VERTEX_POINT ( 'NONE', #1823 ) ;
#16672 = VERTEX_POINT ( 'NONE', #12705 ) ;
#16673 = LINE ( 'NONE', #5599, #13506 ) ;
#16674 = FACE_OUTER_BOUND ( 'NONE', #3601, .T. ) ;
#16675 = VERTEX_POINT ( 'NONE', #5012 ) ;
#16676 = ORIENTED_EDGE ( 'NONE', *, *, #30089, .F. ) ;
#16677 = CYLINDRICAL_SURFACE ( 'NONE', #10471, 34.41491905851385269 ) ;
#16678 = CIRCLE ( 'NONE', #6998, 34.41491905851385269 ) ;
#16679 = CARTESIAN_POINT ( 'NONE',  ( 0.000000000000000000, -33.69708579775584667, 49.43553178847298568 ) ) ;
#16680 = DIRECTION ( 'NONE',  ( -0.000000000000000000, -0.000000000000000000, -1.000000000000000000 ) ) ;
#16681 = EDGE_LOOP ( 'NONE', ( #27465, #34153, #14745, #3462 ) ) ;
#16682 = ORIENTED_EDGE ( 'NONE', *, *, #16095, .F. ) ;
#16683 = EDGE_CURVE ( 'NONE', #29789, #7256, #29587, .T. ) ;
#16684 = DIRECTION ( 'NONE',  ( -1.000000000000000000, 0.000000000000000000, 0.000000000000000000 ) ) ;
#16685 = DIRECTION ( 'NONE',  ( 0.000000000000000000, 1.000000000000000000, 0.000000000000000000 ) ) ;
#16686 = DIRECTION ( 'NONE',  ( -0.5611870653623813876, 0.8276889981568912313, 0.000000000000000000 ) ) ;
#16687 = EDGE_CURVE ( 'NONE', #33582, #30318, #16075, .T. ) ;
#16688 = DIRECTION ( 'NONE',  ( -0.000000000000000000, -1.000000000000000000, -0.000000000000000000 ) ) ;
#16689 = AXIS2_PLACEMENT_3D ( 'NONE', #1382, #28608, #33949 ) ;
#16690 = LINE ( 'NONE', #2957, #13959 ) ;
#16691 = AXIS2_PLACEMENT_3D ( 'NONE', #23937, #31946, #4709 ) ;
#16692 = CARTESIAN_POINT ( 'NONE',  ( -442.0000000000000000, 124.9999999999999432, -159.0000000000000000 ) ) ;
#16693 = CIRCLE ( 'NONE', #1338, 0.3000000000000016542 ) ;
#16694 = LINE ( 'NONE', #34856, #30056 ) ;
#16695 = EDGE_LOOP ( 'NONE', ( #30626, #12827, #11616, #5779, #9876, #23620, #19553, #9633 ) ) ;
#16696 = EDGE_CURVE ( 'NONE', #5869, #16070, #215, .T. ) ;
#16697 = CARTESIAN_POINT ( 'NONE',  ( 10.17231796313407344, -3.615060903476078114, -87.50000000000000000 ) ) ;
#16698 = CARTESIAN_POINT ( 'NONE',  ( 0.02407890056655651728, -15.32140196853772984, 27.05343472112986092 ) ) ;
#16699 = LINE ( 'NONE', #24673, #10958 ) ;
#16700 = ORIENTED_EDGE ( 'NONE', *, *, #16299, .F. ) ;
#16701 = ADVANCED_FACE ( 'NONE', ( #2345 ), #21405, .T. ) ;
#16702 = CARTESIAN_POINT ( 'NONE',  ( -499.9999999999999432, -137.0000000000000000, -155.0000000000000000 ) ) ;
#16703 = VERTEX_POINT ( 'NONE', #7868 ) ;
#16704 = FACE_OUTER_BOUND ( 'NONE', #6961, .T. ) ;
#16705 = CARTESIAN_POINT ( 'NONE',  ( -106.6587923562685916, 4.850327849261239166, 11.52145900171629656 ) ) ;
#16706 = ADVANCED_FACE ( 'NONE', ( #10897 ), #5533, .F. ) ;
#16707 = ADVANCED_FACE ( 'NONE', ( #2523 ), #13402, .F. ) ;
#16708 = AXIS2_PLACEMENT_3D ( 'NONE', #8510, #19379, #2460 ) ;
#16709 = EDGE_LOOP ( 'NONE', ( #2199, #24718, #26815, #5032, #30475, #1962 ) ) ;
#16710 = CARTESIAN_POINT ( 'NONE',  ( 0.000000000000000000, 0.000000000000000000, 0.000000000000000000 ) ) ;
#16711 = DIRECTION ( 'NONE',  ( -0.000000000000000000, -0.000000000000000000, -1.000000000000000000 ) ) ;
#16712 = CARTESIAN_POINT ( 'NONE',  ( -12.00000000000001066, -124.9999999999999432, -154.9999999999999716 ) ) ;
#16713 = ORIENTED_EDGE ( 'NONE', *, *, #14063, .F. ) ;
#16714 = AXIS2_PLACEMENT_3D ( 'NONE', #18472, #2073, #5080 ) ;
#16715 = AXIS2_PLACEMENT_3D ( 'NONE', #14517, #979, #15042 ) ;
#16716 = DIRECTION ( 'NONE',  ( 2.631201909438060585E-14, -5.396010391056496978E-16, 1.000000000000000000 ) ) ;
#16717 = VECTOR ( 'NONE', #5504, 1000.000000000000000 ) ;
#16718 = DIRECTION ( 'NONE',  ( -1.000000000000000000, 0.000000000000000000, -5.546364386991661285E-52 ) ) ;
#16719 = ORIENTED_EDGE ( 'NONE', *, *, #5797, .T. ) ;
#16720 = CARTESIAN_POINT ( 'NONE',  ( 0.7564103395634697025, -9.974843919188980834, -32.41553303492231208 ) ) ;
#16721 =( LENGTH_UNIT ( ) NAMED_UNIT ( * ) SI_UNIT ( .MILLI., .METRE. ) );
#16722 = CARTESIAN_POINT ( 'NONE',  ( -442.0000000000000000, 137.0000000000000000, 154.9999999999999716 ) ) ;
#16723 = CARTESIAN_POINT ( 'NONE',  ( -100.9608953138632899, -3.142556659824618404, 6.811296903636076649 ) ) ;
#16724 = ORIENTED_EDGE ( 'NONE', *, *, #20395, .T. ) ;
#16726 = ORIENTED_EDGE ( 'NONE', *, *, #24817, .T. ) ;
#16725 =( REPRESENTATION_RELATIONSHIP ('NONE','NONE', #23037, #15767 ) REPRESENTATION_RELATIONSHIP_WITH_TRANSFORMATION ( #15319 )SHAPE_REPRESENTATION_RELATIONSHIP( ) );
#16727 = ORIENTED_EDGE ( 'NONE', *, *, #3485, .F. ) ;
#16728 = CARTESIAN_POINT ( 'NONE',  ( 0.006892404480090298657, -29.45646641511004660, 9.233692607045616896 ) ) ;
#16729 = CARTESIAN_POINT ( 'NONE',  ( 0.02407890056655825201, -31.05158812718220673, -1.559667679918931738 ) ) ;
#16730 = CIRCLE ( 'NONE', #22406, 10.00000000000000888 ) ;
#16731 = CARTESIAN_POINT ( 'NONE',  ( -3.250000000000000000, -5.838643359331793015, -0.7500000000000000000 ) ) ;
#16732 = ORIENTED_EDGE ( 'NONE', *, *, #21307, .T. ) ;
#16733 = ORIENTED_EDGE ( 'NONE', *, *, #15930, .F. ) ;
#16734 = CARTESIAN_POINT ( 'NONE',  ( 1.040000000000001590, -30.02688531850382958, -16.81585001935613022 ) ) ;
#16735 = ORIENTED_EDGE ( 'NONE', *, *, #3989, .F. ) ;
#16736 = DIRECTION ( 'NONE',  ( -1.000000000000000000, -3.469446951953834515E-18, 0.000000000000000000 ) ) ;
#16737 = EDGE_CURVE ( 'NONE', #28601, #23670, #2341, .T. ) ;
#16738 = DIRECTION ( 'NONE',  ( 0.000000000000000000, 0.000000000000000000, 1.000000000000000000 ) ) ;
#16739 = ORIENTED_EDGE ( 'NONE', *, *, #33758, .T. ) ;
#16740 = CARTESIAN_POINT ( 'NONE',  ( 0.02407890056655564992, -30.46391896562403190, -6.211548095912885259 ) ) ;
#16741 = VERTEX_POINT ( 'NONE', #5704 ) ;
#16742 = ADVANCED_FACE ( 'NONE', ( #8398 ), #5362, .T. ) ;
#16743 = ADVANCED_FACE ( 'NONE', ( #16605 ), #27439, .F. ) ;
#16744 = VECTOR ( 'NONE', #1331, 1000.000000000000000 ) ;
#16745 = DIRECTION ( 'NONE',  ( 0.000000000000000000, 1.836970198721029441E-16, -1.000000000000000000 ) ) ;
#16746 = VERTEX_POINT ( 'NONE', #13743 ) ;
#16747 = CARTESIAN_POINT ( 'NONE',  ( 17.88561705399011714, -27.19023860642122514, 68.31122994652405112 ) ) ;
#16749 = AXIS2_PLACEMENT_3D ( 'NONE', #29963, #5911, #5730 ) ;
#16748 = CARTESIAN_POINT ( 'NONE',  ( -119.9999999999997726, 0.000000000000000000, 10.00000000000000000 ) ) ;
#16750 = LINE ( 'NONE', #11225, #29199 ) ;
#16751 = LINE ( 'NONE', #27936, #6600 ) ;
#16752 = DIRECTION ( 'NONE',  ( -1.000000000000000000, 0.000000000000000000, 0.000000000000000000 ) ) ;
#16753 = LINE ( 'NONE', #16048, #5953 ) ;
#16754 = DIRECTION ( 'NONE',  ( -1.000000000000000000, -0.000000000000000000, -0.000000000000000000 ) ) ;
#16755 = EDGE_CURVE ( 'NONE', #11863, #4938, #23012, .T. ) ;
#16756 = CIRCLE ( 'NONE', #33791, 4.682234377621698584 ) ;
#16757 = ORIENTED_EDGE ( 'NONE', *, *, #6456, .F. ) ;
#16758 = DIRECTION ( 'NONE',  ( 0.1063910735368947813, -0.9943243633099144718, -3.335902418024520312E-15 ) ) ;
#16759 = ORIENTED_EDGE ( 'NONE', *, *, #1640, .T. ) ;
#16760 = VECTOR ( 'NONE', #23668, 1000.000000000000000 ) ;
#16762 = ORIENTED_EDGE ( 'NONE', *, *, #24709, .T. ) ;
#16761 = EDGE_CURVE ( 'NONE', #23261, #5794, #21661, .T. ) ;
#16763 = ORIENTED_EDGE ( 'NONE', *, *, #12854, .T. ) ;
#16764 = DIRECTION ( 'NONE',  ( -1.000000000000000000, -0.000000000000000000, -0.000000000000000000 ) ) ;
#16765 = EDGE_CURVE ( 'NONE', #24033, #17068, #5177, .T. ) ;
#16766 = AXIS2_PLACEMENT_3D ( 'NONE', #34415, #6996, #25881 ) ;
#16767 = ADVANCED_FACE ( 'NONE', ( #7687 ), #21580, .T. ) ;
#16768 = CARTESIAN_POINT ( 'NONE',  ( 105.7860010550761416, 5.687433884741868617, 4.889179432777876144 ) ) ;
#16769 = APPLICATION_PROTOCOL_DEFINITION ( 'draft international standard', 'automotive_design', 1998, #2351 ) ;
#16770 = VECTOR ( 'NONE', #12156, 1000.000000000000000 ) ;
#16771 = ORIENTED_EDGE ( 'NONE', *, *, #29776, .T. ) ;
#16772 = CARTESIAN_POINT ( 'NONE',  ( 2.789999999999998703, 20.82898695786926524, -22.50081875905949147 ) ) ;
#16773 = DIRECTION ( 'NONE',  ( 0.000000000000000000, 0.000000000000000000, 1.000000000000000000 ) ) ;
#16774 = VECTOR ( 'NONE', #8865, 1000.000000000000227 ) ;
#16775 = EDGE_CURVE ( 'NONE', #12335, #32759, #26198, .T. ) ;
#16776 = CONTEXT_DEPENDENT_SHAPE_REPRESENTATION ( #34689, #21245 ) ;
#16778 = DIRECTION ( 'NONE',  ( 1.232595164407830946E-32, 7.496237820289040735E-63, -1.000000000000000000 ) ) ;
#16777 = CARTESIAN_POINT ( 'NONE',  ( 9.199999999999999289, 15.58845726811990495, 0.000000000000000000 ) ) ;
#16779 = ORIENTED_EDGE ( 'NONE', *, *, #5639, .T. ) ;
#16780 = VERTEX_POINT ( 'NONE', #34939 ) ;
#16781 = CARTESIAN_POINT ( 'NONE',  ( 117.4999999999998579, 0.000000000000000000, 12.50000000000000000 ) ) ;
#16782 = CARTESIAN_POINT ( 'NONE',  ( 0.07094832122174615785, 12.21437217961350719, 29.24586132675256422 ) ) ;
#16783 = PLANE ( 'NONE',  #31865 ) ;
#16784 = CYLINDRICAL_SURFACE ( 'NONE', #17851, 3.999999999999948042 ) ;
#16785 = ORIENTED_EDGE ( 'NONE', *, *, #7254, .F. ) ;
#16786 = LINE ( 'NONE', #29944, #19215 ) ;
#16787 = FACE_OUTER_BOUND ( 'NONE', #23195, .T. ) ;
#16788 = CIRCLE ( 'NONE', #3110, 15.00000000000000000 ) ;
#16789 = CARTESIAN_POINT ( 'NONE',  ( 50.00050000000000239, 0.000000000000000000, 0.000000000000000000 ) ) ;
#16790 = EDGE_CURVE ( 'NONE', #34661, #890, #24576, .T. ) ;
#16791 = EDGE_CURVE ( 'NONE', #15484, #26364, #24067, .T. ) ;
#16792 = EDGE_LOOP ( 'NONE', ( #26690, #25529, #17454, #18236 ) ) ;
#16793 = CIRCLE ( 'NONE', #27561, 4.750000000000004441 ) ;
#16794 = CARTESIAN_POINT ( 'NONE',  ( 1.749999999999999778, 34.17636915695680244, -4.045051921974834208 ) ) ;
#16795 = EDGE_CURVE ( 'NONE', #13175, #31799, #30646, .T. ) ;
#16796 = AXIS2_PLACEMENT_3D ( 'NONE', #30902, #28236, #25552 ) ;
#16797 = CARTESIAN_POINT ( 'NONE',  ( 15.99999999999998579, 4.559999999999908127, 172.9900000000000091 ) ) ;
#16799 = DIRECTION ( 'NONE',  ( -1.000000000000000000, 0.000000000000000000, 0.000000000000000000 ) ) ;
#16798 = DIRECTION ( 'NONE',  ( 1.000000000000000000, -0.000000000000000000, -0.000000000000000000 ) ) ;
#16800 = VECTOR ( 'NONE', #30571, 1000.000000000000000 ) ;
#16801 = AXIS2_PLACEMENT_3D ( 'NONE', #23651, #15305, #25969 ) ;
#16802 = FACE_OUTER_BOUND ( 'NONE', #34706, .T. ) ;
#16803 = EDGE_LOOP ( 'NONE', ( #9995, #25248, #14320, #19490 ) ) ;
#16804 = CARTESIAN_POINT ( 'NONE',  ( 6.857172176539690689, 37.23415287044793587, 68.31122994652405112 ) ) ;
#16805 =( LENGTH_UNIT ( ) NAMED_UNIT ( * ) SI_UNIT ( .MILLI., .METRE. ) );
#16806 = AXIS2_PLACEMENT_3D ( 'NONE', #15383, #23377, #28554 ) ;
#16807 = ORIENTED_EDGE ( 'NONE', *, *, #22419, .F. ) ;
#16808 = B_SPLINE_CURVE_WITH_KNOTS ( 'NONE', 3,
 ( #35056, #32716, #21522, #19039, #5646, #26501 ),
 .UNSPECIFIED., .F., .F.,
 ( 4, 2, 4 ),
 ( 2.120780580244199601E-07, 0.001873410385593401008, 0.003746608693128777694 ),
 .UNSPECIFIED. ) ;
#16809 = VERTEX_POINT ( 'NONE', #22108 ) ;
#16810 = ADVANCED_FACE ( 'NONE', ( #19798 ), #16784, .F. ) ;
#16811 = ADVANCED_FACE ( 'NONE', ( #11965 ), #27966, .F. ) ;
#16812 = VECTOR ( 'NONE', #2257, 1000.000000000000000 ) ;
#16813 = VECTOR ( 'NONE', #29593, 1000.000000000000000 ) ;
#16814 = ORIENTED_EDGE ( 'NONE', *, *, #16963, .T. ) ;
#16815 = FACE_BOUND ( 'NONE', #32897, .T. ) ;
#16816 = ORIENTED_EDGE ( 'NONE', *, *, #27429, .F. ) ;
#16817 = EDGE_LOOP ( 'NONE', ( #21915, #7425, #22519, #21542, #6755, #14808, #1811, #1608, #25410, #29479, #1765, #9271, #20505, #6127, #32271, #22484 ) ) ;
#16818 = CARTESIAN_POINT ( 'NONE',  ( 2.789999999999999147, 20.79173593595263014, 22.27454621808771762 ) ) ;
#16819 = AXIS2_PLACEMENT_3D ( 'NONE', #9375, #31088, #28414 ) ;
#16820 = ADVANCED_FACE ( 'NONE', ( #19625 ), #9873, .T. ) ;
#16821 = ITEM_DEFINED_TRANSFORMATION ( 'NONE', 'NONE', #9857,  #28566 ) ;
#16822 = ORIENTED_EDGE ( 'NONE', *, *, #22506, .T. ) ;
#16823 = DIRECTION ( 'NONE',  ( 1.000000000000000000, 0.000000000000000000, 0.000000000000000000 ) ) ;
#16824 = CARTESIAN_POINT ( 'NONE',  ( -499.9999999999999432, 140.9999999999999716, -187.0000000000000000 ) ) ;
#16825 = ORIENTED_EDGE ( 'NONE', *, *, #32441, .F. ) ;
#16826 = ORIENTED_EDGE ( 'NONE', *, *, #17909, .F. ) ;
#16827 = VECTOR ( 'NONE', #2452, 1000.000000000000000 ) ;
#16828 = FACE_OUTER_BOUND ( 'NONE', #17687, .T. ) ;
#16829 = ADVANCED_FACE ( 'NONE', ( #6233 ), #14282, .F. ) ;
#16830 = CARTESIAN_POINT ( 'NONE',  ( 10.00000000000000000, -1.505030548027689319, 3.180000000000000160 ) ) ;
#16831 = AXIS2_PLACEMENT_3D ( 'NONE', #13758, #2881, #225 ) ;
#16832 = LINE ( 'NONE', #22321, #18170 ) ;
#16833 = CARTESIAN_POINT ( 'NONE',  ( 1.394999999999999574, -33.39989884085085947, -8.296590337300607132 ) ) ;
#16834 = ORIENTED_EDGE ( 'NONE', *, *, #14194, .F. ) ;
#16835 = DIRECTION ( 'NONE',  ( 0.000000000000000000, 1.836970198721029441E-16, -1.000000000000000000 ) ) ;
#16836 = DIRECTION ( 'NONE',  ( -1.000000000000000000, 0.000000000000000000, 0.000000000000000000 ) ) ;
#16837 = ORIENTED_EDGE ( 'NONE', *, *, #29387, .F. ) ;
#16838 = CARTESIAN_POINT ( 'NONE',  ( 29.82459402470849952, -33.69708579775585378, -36.68877005347594888 ) ) ;
#16839 = DIRECTION ( 'NONE',  ( -0.000000000000000000, 1.836970198721029934E-16, -1.000000000000000000 ) ) ;
#16840 = CARTESIAN_POINT ( 'NONE',  ( 1.394999999999999574, 6.183021911002327897, -33.85493898757056996 ) ) ;
#16841 = CARTESIAN_POINT ( 'NONE',  ( -12.00000000000001066, -145.0000000000000000, 155.0000000000000000 ) ) ;
#16842 = FACE_OUTER_BOUND ( 'NONE', #9831, .T. ) ;
#16843 = DIRECTION ( 'NONE',  ( 0.000000000000000000, 1.836970198721029441E-16, -1.000000000000000000 ) ) ;
#16844 = ORIENTED_EDGE ( 'NONE', *, *, #4115, .T. ) ;
#16845 = ADVANCED_FACE ( 'NONE', ( #11792 ), #32944, .T. ) ;
#16847 = CYLINDRICAL_SURFACE ( 'NONE', #10040, 7.999999999999952038 ) ;
#16846 = CARTESIAN_POINT ( 'NONE',  ( 1.394999999999999574, 27.68252950111338251, 20.44661865013498669 ) ) ;
#16848 = ORIENTED_EDGE ( 'NONE', *, *, #25455, .T. ) ;
#16849 = FACE_OUTER_BOUND ( 'NONE', #6885, .T. ) ;
#16850 = CARTESIAN_POINT ( 'NONE',  ( -12.00000000000001066, 134.9999999999998863, 162.9999999999999716 ) ) ;
#16851 = AXIS2_PLACEMENT_3D ( 'NONE', #24023, #2844, #5334 ) ;
#16852 = EDGE_CURVE ( 'NONE', #12415, #13518, #6462, .T. ) ;
#16853 = ORIENTED_EDGE ( 'NONE', *, *, #24296, .F. ) ;
#16854 = ADVANCED_FACE ( 'NONE', ( #741 ), #19444, .F. ) ;
#16855 = ADVANCED_FACE ( 'NONE', ( #8923 ), #30281, .F. ) ;
#16856 = ORIENTED_EDGE ( 'NONE', *, *, #25026, .F. ) ;
#16857 = DIRECTION ( 'NONE',  ( -1.232595164407830946E-32, -3.421138828918010427E-49, 1.000000000000000000 ) ) ;
#16858 = LINE ( 'NONE', #27682, #29572 ) ;
#16859 = ORIENTED_EDGE ( 'NONE', *, *, #32824, .T. ) ;
#16860 = EDGE_LOOP ( 'NONE', ( #5465, #10940, #21218, #774, #30282, #29527, #8500, #988 ) ) ;
#16861 = DIRECTION ( 'NONE',  ( 0.000000000000000000, 0.000000000000000000, 1.000000000000000000 ) ) ;
#16862 = DIRECTION ( 'NONE',  ( 0.000000000000000000, -0.5000000000000004441, 0.8660254037844382635 ) ) ;
#16863 = AXIS2_PLACEMENT_3D ( 'NONE', #8393, #5699, #30106 ) ;
#16864 = CARTESIAN_POINT ( 'NONE',  ( 2.789999999999999147, 0.000000000000000000, 0.000000000000000000 ) ) ;
#16865 = CARTESIAN_POINT ( 'NONE',  ( 37.71145559917817280, 3.353962854566119756, 68.31122994652405112 ) ) ;
#16866 = ORIENTED_EDGE ( 'NONE', *, *, #10623, .F. ) ;
#16867 = ORIENTED_EDGE ( 'NONE', *, *, #10312, .T. ) ;
#16868 = DIRECTION ( 'NONE',  ( -0.8276889981568902321, -0.5611870653623829419, 0.000000000000000000 ) ) ;
#16869 = CYLINDRICAL_SURFACE ( 'NONE', #21516, 7.999999999999992895 ) ;
#16870 = LINE ( 'NONE', #27695, #16359 ) ;
#16871 = AXIS2_PLACEMENT_3D ( 'NONE', #14556, #25203, #33398 ) ;
#16872 = DIRECTION ( 'NONE',  ( 0.000000000000000000, 1.310824597558155437E-49, 1.000000000000000000 ) ) ;
#16873 = DIRECTION ( 'NONE',  ( 0.000000000000000000, 0.000000000000000000, -1.000000000000000000 ) ) ;
#16874 = LINE ( 'NONE', #19531, #29858 ) ;
#16875 = CARTESIAN_POINT ( 'NONE',  ( -430.0000000000000000, -131.0000000000000000, 128.0000000000000000 ) ) ;
#16876 = CARTESIAN_POINT ( 'NONE',  ( -9.978866888775426602, 18.16264470403145026, -67.50000000000000000 ) ) ;
#16877 = ORIENTED_EDGE ( 'NONE', *, *, #8308, .F. ) ;
#16878 = CONICAL_SURFACE ( 'NONE', #8336, 12.50000000000000000, 0.7853981633974431720 ) ;
#16879 = DIRECTION ( 'NONE',  ( 0.000000000000000000, 0.000000000000000000, -1.000000000000000000 ) ) ;
#16880 = DIRECTION ( 'NONE',  ( -1.000000000000000000, 0.000000000000000000, 0.000000000000000000 ) ) ;
#16881 = CARTESIAN_POINT ( 'NONE',  ( 0.000000000000000000, -33.69708579775585378, -36.68877005347594178 ) ) ;
#16882 = EDGE_LOOP ( 'NONE', ( #29155, #12686, #12169, #18671 ) ) ;
#16883 = CARTESIAN_POINT ( 'NONE',  ( -262.5000000000000000, 9.184850993605147944E-16, -7.500000000000000000 ) ) ;
#16884 = EDGE_LOOP ( 'NONE', ( #23938, #15823, #7669, #8725, #6710, #32406 ) ) ;
#16885 = CARTESIAN_POINT ( 'NONE',  ( -345.0000000000000000, 134.9999999999999716, 125.9999999999999716 ) ) ;
#16886 = DIRECTION ( 'NONE',  ( 0.000000000000000000, 1.836970198721029441E-16, -1.000000000000000000 ) ) ;
#16887 = AXIS2_PLACEMENT_3D ( 'NONE', #23715, #24049, #7863 ) ;
#16888 = ORIENTED_EDGE ( 'NONE', *, *, #27157, .F. ) ;
#16889 = EDGE_CURVE ( 'NONE', #5434, #8847, #15575, .T. ) ;
#16890 = CARTESIAN_POINT ( 'NONE',  ( 2.719051660387896696, 14.74858964725069654, 28.05334937082597335 ) ) ;
#16891 = DIRECTION ( 'NONE',  ( -1.232595164407830946E-32, -7.496237820289040735E-63, 1.000000000000000000 ) ) ;
#16892 = CARTESIAN_POINT ( 'NONE',  ( -12.00000000000001066, 144.9999999999999147, 162.9999999999999716 ) ) ;
#16893 = EDGE_CURVE ( 'NONE', #1848, #11811, #33125, .T. ) ;
#16894 = ORIENTED_EDGE ( 'NONE', *, *, #1262, .T. ) ;
#16895 = ADVANCED_FACE ( 'NONE', ( #16964 ), #24621, .T. ) ;
#16896 = DIRECTION ( 'NONE',  ( 0.1063910735369155841, -0.9943243633099125844, -3.335902418025060287E-15 ) ) ;
#16897 = DIRECTION ( 'NONE',  ( 2.891205793294675368E-16, 7.888609052210118054E-31, 1.000000000000000000 ) ) ;
#16898 = EDGE_CURVE ( 'NONE', #9865, #21866, #31864, .T. ) ;
#16899 = ORIENTED_EDGE ( 'NONE', *, *, #29932, .T. ) ;
#16900 = CARTESIAN_POINT ( 'NONE',  ( 1.040000000000000924, -10.37741591188871482, -32.81304455236878681 ) ) ;
#16901 = DIRECTION ( 'NONE',  ( 0.000000000000000000, 0.000000000000000000, 1.000000000000000000 ) ) ;
#16902 = CARTESIAN_POINT ( 'NONE',  ( -500.0000000000000000, -113.0000000000000000, 194.9999999999999716 ) ) ;
#16903 = CARTESIAN_POINT ( 'NONE',  ( -41.91706493227329133, 16.36947364650383818, -36.69637551990492597 ) ) ;
#16904 = EDGE_LOOP ( 'NONE', ( #26092, #24375, #11162, #34115, #34868, #10063, #6185, #30578 ) ) ;
#16905 = ORIENTED_EDGE ( 'NONE', *, *, #9383, .F. ) ;
#16906 = EDGE_LOOP ( 'NONE', ( #5492, #17815, #529, #30226 ) ) ;
#16907 = PRODUCT_DEFINITION_SHAPE ( 'NONE', 'NONE',  #35097 ) ;
#16908 = PRESENTATION_STYLE_ASSIGNMENT (( #25415 ) ) ;
#16909 = MECHANICAL_DESIGN_GEOMETRIC_PRESENTATION_REPRESENTATION (  '', ( #32229 ), #22585 ) ;
#16910 = EDGE_CURVE ( 'NONE', #13666, #6940, #10836, .T. ) ;
#16911 = CARTESIAN_POINT ( 'NONE',  ( 0.000000000000000000, 0.000000000000000000, 0.000000000000000000 ) ) ;
#16912 = VECTOR ( 'NONE', #9754, 1000.000000000000000 ) ;
#16913 = AXIS2_PLACEMENT_3D ( 'NONE', #27038, #32542, #7984 ) ;
#16914 = CARTESIAN_POINT ( 'NONE',  ( -499.9999999999999432, 112.9999999999999574, 194.9999999999999716 ) ) ;
#16915 = ORIENTED_EDGE ( 'NONE', *, *, #7701, .T. ) ;
#16916 = ORIENTED_EDGE ( 'NONE', *, *, #33742, .T. ) ;
#16917 = CARTESIAN_POINT ( 'NONE',  ( 2.606462089965854378, -28.84240889917340667, 14.47562221546536776 ) ) ;
#16918 = ORIENTED_EDGE ( 'NONE', *, *, #6815, .T. ) ;
#16919 = CARTESIAN_POINT ( 'NONE',  ( -35.00000000000000000, 3.432458613951609561, -15.93718699791188342 ) ) ;
#16920 = DIRECTION ( 'NONE',  ( -0.000000000000000000, 1.836970198721029934E-16, -1.000000000000000000 ) ) ;
#16921 = VERTEX_POINT ( 'NONE', #6493 ) ;
#16922 = VERTEX_POINT ( 'NONE', #146 ) ;
#16923 = LINE ( 'NONE', #3365, #4371 ) ;
#16924 = CIRCLE ( 'NONE', #13477, 3.999999999999976019 ) ;
#16925 = LINE ( 'NONE', #21887, #32534 ) ;
#16926 = ORIENTED_EDGE ( 'NONE', *, *, #8949, .F. ) ;
#16927 = CARTESIAN_POINT ( 'NONE',  ( -442.0000000000000000, 105.0000000000000142, -101.9999999999999858 ) ) ;
#16928 = FILL_AREA_STYLE ('',( #19765 ) ) ;
#16929 = CARTESIAN_POINT ( 'NONE',  ( -430.0000000000000000, -135.0000000000000000, 126.0000000000000000 ) ) ;
#16930 = LINE ( 'NONE', #27757, #24209 ) ;
#16931 = AXIS2_PLACEMENT_3D ( 'NONE', #24649, #16499, #30352 ) ;
#16932 = CARTESIAN_POINT ( 'NONE',  ( -102.4259574044266543, -4.432593925698492754, 11.68934397677213965 ) ) ;
#16933 = LINE ( 'NONE', #27761, #15648 ) ;
#16934 = DIRECTION ( 'NONE',  ( 0.000000000000000000, 1.000000000000000000, 0.000000000000000000 ) ) ;
#16935 = EDGE_CURVE ( 'NONE', #14860, #32635, #13294, .T. ) ;
#16936 = ORIENTED_EDGE ( 'NONE', *, *, #31141, .F. ) ;
#16937 = AXIS2_PLACEMENT_3D ( 'NONE', #32421, #8216, #26561 ) ;
#16938 = CIRCLE ( 'NONE', #8939, 11.79999999999999893 ) ;
#16939 = ORIENTED_EDGE ( 'NONE', *, *, #2238, .T. ) ;
#16940 = CARTESIAN_POINT ( 'NONE',  ( 848.5013446888283397, 1054.520109691897460, 1753.598338701303419 ) ) ;
#16941 =( REPRESENTATION_RELATIONSHIP ('NONE','NONE', #23037, #1195 ) REPRESENTATION_RELATIONSHIP_WITH_TRANSFORMATION ( #33466 )SHAPE_REPRESENTATION_RELATIONSHIP( ) );
#16942 = EDGE_CURVE ( 'NONE', #30178, #22409, #2810, .T. ) ;
#16943 = ORIENTED_EDGE ( 'NONE', *, *, #19313, .T. ) ;
#16944 = VERTEX_POINT ( 'NONE', #24174 ) ;
#16945 = EDGE_CURVE ( 'NONE', #33601, #14361, #30052, .T. ) ;
#16946 = VECTOR ( 'NONE', #7066, 1000.000000000000000 ) ;
#16947 = CARTESIAN_POINT ( 'NONE',  ( 0.02407890056655608360, -31.05158812718222450, 1.559667679918499417 ) ) ;
#16948 = EDGE_CURVE ( 'NONE', #8902, #32774, #27027, .T. ) ;
#16949 = CARTESIAN_POINT ( 'NONE',  ( 100.7111166766537735, 3.828784459365716319, 6.456053091683092049 ) ) ;
#16950 = EDGE_CURVE ( 'NONE', #6786, #20123, #24511, .T. ) ;
#16951 = SHAPE_DEFINITION_REPRESENTATION ( #11490, #8672 ) ;
#16952 = ORIENTED_EDGE ( 'NONE', *, *, #16978, .T. ) ;
#16953 = CARTESIAN_POINT ( 'NONE',  ( -442.0000000000000000, 105.0000000000000142, 194.9999999999999716 ) ) ;
#16954 = SURFACE_STYLE_USAGE ( .BOTH. , #11953 ) ;
#16956 = FACE_OUTER_BOUND ( 'NONE', #25948, .T. ) ;
#16955 = LINE ( 'NONE', #11243, #1402 ) ;
#16957 = VECTOR ( 'NONE', #11114, 1000.000000000000000 ) ;
#16958 = ORIENTED_EDGE ( 'NONE', *, *, #10853, .F. ) ;
#16959 = EDGE_LOOP ( 'NONE', ( #11926, #5663, #5841, #1420, #1330, #26149, #11261, #1274 ) ) ;
#16960 = LINE ( 'NONE', #19440, #6614 ) ;
#16961 = DIRECTION ( 'NONE',  ( -0.000000000000000000, -0.000000000000000000, 1.000000000000000000 ) ) ;
#16963 = EDGE_CURVE ( 'NONE', #17092, #25727, #21681, .T. ) ;
#16962 = DIRECTION ( 'NONE',  ( 1.000000000000000000, 0.000000000000000000, 0.000000000000000000 ) ) ;
#16964 = FACE_OUTER_BOUND ( 'NONE', #5951, .T. ) ;
#16965 = ORIENTED_EDGE ( 'NONE', *, *, #7535, .T. ) ;
#16967 = VECTOR ( 'NONE', #5888, 1000.000000000000000 ) ;
#16966 = CARTESIAN_POINT ( 'NONE',  ( 36.10877985260814427, 11.38239727801116352, 68.31122994652405112 ) ) ;
#16969 = DIRECTION ( 'NONE',  ( -1.000000000000000000, 0.000000000000000000, -1.300283923313630633E-47 ) ) ;
#16968 = CIRCLE ( 'NONE', #30415, 1.999999999999999556 ) ;
#16970 = DIRECTION ( 'NONE',  ( 0.000000000000000000, 1.836970198721029688E-16, -1.000000000000000000 ) ) ;
#16971 = ORIENTED_EDGE ( 'NONE', *, *, #22413, .F. ) ;
#16972 = CARTESIAN_POINT ( 'NONE',  ( 1.749999999999999778, 0.000000000000000000, 0.000000000000000000 ) ) ;
#16973 = DIRECTION ( 'NONE',  ( 0.000000000000000000, 2.309213040847544338E-50, 1.000000000000000000 ) ) ;
#16974 = PLANE ( 'NONE',  #5274 ) ;
#16975 = VECTOR ( 'NONE', #2218, 1000.000000000000000 ) ;
#16977 = FACE_OUTER_BOUND ( 'NONE', #3024, .T. ) ;
#16976 = LINE ( 'NONE', #11622, #6495 ) ;
#16978 = EDGE_CURVE ( 'NONE', #22599, #33196, #24694, .T. ) ;
#16979 = FACE_OUTER_BOUND ( 'NONE', #32046, .T. ) ;
#16980 = ORIENTED_EDGE ( 'NONE', *, *, #30914, .F. ) ;
#16981 = CARTESIAN_POINT ( 'NONE',  ( 145.0000000000000568, -87.50000000000000000, 51.88904920397797582 ) ) ;
#16982 = PLANE ( 'NONE',  #27946 ) ;
#16983 = VECTOR ( 'NONE', #30639, 1000.000000000000000 ) ;
#16984 = ORIENTED_EDGE ( 'NONE', *, *, #32787, .F. ) ;
#16985 = ORIENTED_EDGE ( 'NONE', *, *, #33829, .T. ) ;
#16986 = AXIS2_PLACEMENT_3D ( 'NONE', #29177, #4772, #6756 ) ;
#16987 = EDGE_CURVE ( 'NONE', #14102, #4571, #26360, .T. ) ;
#16988 = EDGE_CURVE ( 'NONE', #25253, #8062, #786, .T. ) ;
#16989 = CIRCLE ( 'NONE', #17558, 1.999999999999999556 ) ;
#16990 = ORIENTED_EDGE ( 'NONE', *, *, #6943, .F. ) ;
#16991 = CARTESIAN_POINT ( 'NONE',  ( -20.00000000000007461, 136.9999999999999432, 159.0000000000000000 ) ) ;
#16992 = EDGE_LOOP ( 'NONE', ( #11684, #14544, #13169, #3529 ) ) ;
#16993 = ORIENTED_EDGE ( 'NONE', *, *, #20853, .T. ) ;
#16994 = DIRECTION ( 'NONE',  ( 0.000000000000000000, 1.000000000000000000, 1.224646799147353207E-16 ) ) ;
#16995 = VECTOR ( 'NONE', #5700, 1000.000000000000000 ) ;
#16996 = CONTEXT_DEPENDENT_SHAPE_REPRESENTATION ( #33759, #7477 ) ;
#16997 = ORIENTED_EDGE ( 'NONE', *, *, #3993, .T. ) ;
#16998 = DIRECTION ( 'NONE',  ( -0.000000000000000000, -0.000000000000000000, 1.000000000000000000 ) ) ;
#16999 = DIRECTION ( 'NONE',  ( 1.000000000000000000, 0.000000000000000000, 0.000000000000000000 ) ) ;
#17000 = ORIENTED_EDGE ( 'NONE', *, *, #7655, .T. ) ;
#17001 = ORIENTED_EDGE ( 'NONE', *, *, #15120, .T. ) ;
#17002 = FACE_BOUND ( 'NONE', #20680, .T. ) ;
#17003 = CARTESIAN_POINT ( 'NONE',  ( -349.0000000000000000, 124.9999999999999432, 185.0000000000000000 ) ) ;
#17004 = CARTESIAN_POINT ( 'NONE',  ( 100.4462052625313646, -3.510783659749458607, -12.00105596243589723 ) ) ;
#17006 = EDGE_CURVE ( 'NONE', #33375, #32001, #226, .T. ) ;
#17005 = PLANE ( 'NONE',  #26 ) ;
#17007 = CARTESIAN_POINT ( 'NONE',  ( -262.5000000000000000, 0.000000000000000000, 0.000000000000000000 ) ) ;
#17008 = ORIENTED_EDGE ( 'NONE', *, *, #2470, .F. ) ;
#17009 = CARTESIAN_POINT ( 'NONE',  ( 212.5000000000000000, 0.000000000000000000, 10.00000000000000000 ) ) ;
#17010 = AXIS2_PLACEMENT_3D ( 'NONE', #17047, #30372, #11514 ) ;
#17011 = LINE ( 'NONE', #19671, #6771 ) ;
#17012 = VERTEX_POINT ( 'NONE', #13676 ) ;
#17013 = CARTESIAN_POINT ( 'NONE',  ( -361.0000000000000000, -125.0000000000000284, 166.9999999999999716 ) ) ;
#17015 = ADVANCED_FACE ( 'NONE', ( #22041 ), #29529, .F. ) ;
#17014 = PLANE ( 'NONE',  #12644 ) ;
#17016 = DIRECTION ( 'NONE',  ( -1.000000000000000000, 0.000000000000000000, 0.000000000000000000 ) ) ;
#17017 = EDGE_CURVE ( 'NONE', #28736, #5918, #16013, .T. ) ;
#17018 = CARTESIAN_POINT ( 'NONE',  ( 99.58104344416952358, 1.924456215511286983, -7.258046499395033102 ) ) ;
#17019 = CARTESIAN_POINT ( 'NONE',  ( -20.63749999999999574, 0.000000000000000000, 0.000000000000000000 ) ) ;
#17020 = COLOUR_RGB ( '',0.7921568627450980005, 0.8196078431372548767, 0.9333333333333333481 ) ;
#17021 = EDGE_CURVE ( 'NONE', #10430, #18467, #9324, .T. ) ;
#17022 = CARTESIAN_POINT ( 'NONE',  ( -499.9999999999999432, 112.9999999999999574, 155.0000000000000000 ) ) ;
#17023 = VERTEX_POINT ( 'NONE', #18857 ) ;
#17024 = LINE ( 'NONE', #14519, #16744 ) ;
#17026 = DIRECTION ( 'NONE',  ( -1.000000000000000000, -3.469446951953834515E-18, 0.000000000000000000 ) ) ;
#17025 = DIRECTION ( 'NONE',  ( -1.000000000000000000, 0.000000000000000000, 0.000000000000000000 ) ) ;
#17027 = EDGE_CURVE ( 'NONE', #4415, #3245, #13846, .T. ) ;
#17028=STYLED_ITEM('',(#35254),#12482);
#17029 = ORIENTED_EDGE ( 'NONE', *, *, #8508, .T. ) ;
#17030 = DIRECTION ( 'NONE',  ( -0.9868265225415260300, -0.1617819965527648174, 0.000000000000000000 ) ) ;
#17031 = CARTESIAN_POINT ( 'NONE',  ( 2.790000000000000480, -30.61407293071425428, -1.706449706642680697 ) ) ;
#17032 = EDGE_LOOP ( 'NONE', ( #16997, #5698, #26447, #8869 ) ) ;
#17033 = EDGE_LOOP ( 'NONE', ( #34509, #25946, #16905, #2833 ) ) ;
#17034 = CARTESIAN_POINT ( 'NONE',  ( -12.00000000000001066, 144.9999999999999716, -186.9999999999999716 ) ) ;
#17035 = ORIENTED_EDGE ( 'NONE', *, *, #31805, .T. ) ;
#17036 = ORIENTED_EDGE ( 'NONE', *, *, #12158, .F. ) ;
#17037 = CARTESIAN_POINT ( 'NONE',  ( -365.0000000000000000, -125.0000000000000284, 113.9999999999999858 ) ) ;
#17038 = DIRECTION ( 'NONE',  ( 0.000000000000000000, 0.000000000000000000, 1.000000000000000000 ) ) ;
#17039 = AXIS2_PLACEMENT_3D ( 'NONE', #6494, #17568, #9537 ) ;
#17040 = DIRECTION ( 'NONE',  ( -3.040835319149746528E-31, -1.000000000000000000, 0.000000000000000000 ) ) ;
#17041 = CARTESIAN_POINT ( 'NONE',  ( -0.2989565185775304723, 1.809415645740214338E-15, -14.77500000000000036 ) ) ;
#17042 = ORIENTED_EDGE ( 'NONE', *, *, #34767, .T. ) ;
#17043 = ORIENTED_EDGE ( 'NONE', *, *, #21303, .T. ) ;
#17044 = CARTESIAN_POINT ( 'NONE',  ( 0.5288002497500084997, -32.52406052302386996, 7.554116419246433622 ) ) ;
#17045 = DIRECTION ( 'NONE',  ( -1.000000000000000000, 0.000000000000000000, 0.000000000000000000 ) ) ;
#17046 = PLANE ( 'NONE',  #7224 ) ;
#17047 = CARTESIAN_POINT ( 'NONE',  ( 0.000000000000000000, 2.281310696040539424E-14, -36.68877005347592757 ) ) ;
#17048 = CARTESIAN_POINT ( 'NONE',  ( 0.000000000000000000, 2.281310696040539424E-14, -36.68877005347594178 ) ) ;
#17049 = AXIS2_PLACEMENT_3D ( 'NONE', #13974, #24807, #3965 ) ;
#17050 = CYLINDRICAL_SURFACE ( 'NONE', #30999, 34.41491905851385269 ) ;
#17051 = CYLINDRICAL_SURFACE ( 'NONE', #28358, 16.19999999999999574 ) ;
#17052 = ORIENTED_EDGE ( 'NONE', *, *, #10468, .T. ) ;
#17053 = LINE ( 'NONE', #22195, #4829 ) ;
#17054 = DIRECTION ( 'NONE',  ( 1.000000000000000000, -0.000000000000000000, -0.000000000000000000 ) ) ;
#17055 = ADVANCED_FACE ( 'NONE', ( #13342 ), #35053, .T. ) ;
#17056 = CARTESIAN_POINT ( 'NONE',  ( -414.0000000000000568, -104.9999999999999716, -187.0000000000000000 ) ) ;
#17057 = ORIENTED_EDGE ( 'NONE', *, *, #323, .T. ) ;
#17058 = EDGE_CURVE ( 'NONE', #26512, #14449, #16190, .T. ) ;
#17059 = VECTOR ( 'NONE', #27259, 1000.000000000000000 ) ;
#17060 = CARTESIAN_POINT ( 'NONE',  ( 0.02407890056655695096, 20.99477179376858871, -22.93149026599722617 ) ) ;
#17061 = VERTEX_POINT ( 'NONE', #11726 ) ;
#17062 = CARTESIAN_POINT ( 'NONE',  ( -35.00000000000000000, -4.184937238521382774, 68.31122994652405112 ) ) ;
#17063 = CARTESIAN_POINT ( 'NONE',  ( 8.927936315454010341, -31.29690601358701940, 68.31122994652405112 ) ) ;
#17064 = ORIENTED_EDGE ( 'NONE', *, *, #14084, .T. ) ;
#17065 = CARTESIAN_POINT ( 'NONE',  ( -499.9999999999999432, 112.9999999999999574, 187.0000000000000000 ) ) ;
#17066 = CYLINDRICAL_SURFACE ( 'NONE', #17950, 3.999999999999976019 ) ;
#17067 = DIRECTION ( 'NONE',  ( -0.000000000000000000, 0.000000000000000000, -1.000000000000000000 ) ) ;
#17068 = VERTEX_POINT ( 'NONE', #25226 ) ;
#17069 = AXIS2_PLACEMENT_3D ( 'NONE', #27505, #4293, #1636 ) ;
#17070 = DIRECTION ( 'NONE',  ( 0.1063910735369155841, -0.9943243633099125844, -3.335902418025060287E-15 ) ) ;
#17071 = CARTESIAN_POINT ( 'NONE',  ( 8.000000000000001776, 10.30000000000000071, 0.000000000000000000 ) ) ;
#17072 = ORIENTED_EDGE ( 'NONE', *, *, #15404, .F. ) ;
#17073 = PLANE ( 'NONE',  #18406 ) ;
#17074 = SURFACE_STYLE_USAGE ( .BOTH. , #14040 ) ;
#17075 = CARTESIAN_POINT ( 'NONE',  ( -499.9999999999999432, 136.9999999999999432, 187.0000000000000000 ) ) ;
#17076 = LINE ( 'NONE', #33957, #8550 ) ;
#17077 = CONTEXT_DEPENDENT_SHAPE_REPRESENTATION ( #34908, #20280 ) ;
#17078 = ORIENTED_EDGE ( 'NONE', *, *, #22172, .T. ) ;
#17079 = ORIENTED_EDGE ( 'NONE', *, *, #171, .T. ) ;
#17080 = ORIENTED_EDGE ( 'NONE', *, *, #3946, .T. ) ;
#17081 = CARTESIAN_POINT ( 'NONE',  ( -12.00000000000001243, 134.9999999999999432, -154.9999999999999716 ) ) ;
#17082 = DIRECTION ( 'NONE',  ( -1.000000000000000000, 0.000000000000000000, -0.000000000000000000 ) ) ;
#17083 = FACE_OUTER_BOUND ( 'NONE', #18824, .T. ) ;
#17084 = FACE_OUTER_BOUND ( 'NONE', #72, .T. ) ;
#17085 = ORIENTED_EDGE ( 'NONE', *, *, #9120, .T. ) ;
#17086 = ORIENTED_EDGE ( 'NONE', *, *, #2823, .T. ) ;
#17087 = DIRECTION ( 'NONE',  ( 0.000000000000000000, 3.606850791634946256E-15, -1.000000000000000000 ) ) ;
#17088 = ORIENTED_EDGE ( 'NONE', *, *, #3252, .T. ) ;
#17089 = EDGE_CURVE ( 'NONE', #3012, #4601, #3031, .T. ) ;
#17090 = LINE ( 'NONE', #27923, #25997 ) ;
#17091 = CARTESIAN_POINT ( 'NONE',  ( 29.82459402470852083, 33.69708579775584667, -49.43553178847298568 ) ) ;
#17092 = VERTEX_POINT ( 'NONE', #19559 ) ;
#17093 = CIRCLE ( 'NONE', #32959, 2.524999999999999467 ) ;
#17094 = ORIENTED_EDGE ( 'NONE', *, *, #25456, .T. ) ;
#17095 = DIRECTION ( 'NONE',  ( -1.232595164407831220E-32, 3.421138828918010427E-49, -1.000000000000000000 ) ) ;
#17096 = ADVANCED_FACE ( 'NONE', ( #8683 ), #17073, .T. ) ;
#17097 = LINE ( 'NONE', #27930, #31404 ) ;
#17098 = EDGE_LOOP ( 'NONE', ( #29510, #22224, #12832, #34686 ) ) ;
#17099 = LINE ( 'NONE', #14611, #28850 ) ;
#17100 = DIRECTION ( 'NONE',  ( 0.000000000000000000, 0.000000000000000000, -1.000000000000000000 ) ) ;
#17101 = CARTESIAN_POINT ( 'NONE',  ( 127.4999999999999147, 3.061616997868169163E-16, -2.499999999999825473 ) ) ;
#17102 = DIRECTION ( 'NONE',  ( 0.9941379571543594862, 0.1081190184239433083, -0.000000000000000000 ) ) ;
#17103 = AXIS2_PLACEMENT_3D ( 'NONE', #8017, #13719, #14 ) ;
#17104 = CARTESIAN_POINT ( 'NONE',  ( -109.8494042611863506, -1.661087400543260317, 12.39310421627767766 ) ) ;
#17105 = CARTESIAN_POINT ( 'NONE',  ( 1.749999999999999778, 32.09669216789253454, -12.41728656686340138 ) ) ;
#17106 = DIRECTION ( 'NONE',  ( 0.000000000000000000, 1.000000000000000000, -1.310824597558155437E-49 ) ) ;
#17107 = B_SPLINE_CURVE_WITH_KNOTS ( 'NONE', 3,
 ( #3334, #9032, #33050, #6347 ),
 .UNSPECIFIED., .F., .F.,
 ( 4, 4 ),
 ( 0.005298349496164135759, 0.005985218188604201316 ),
 .UNSPECIFIED. ) ;
#17108 = ORIENTED_EDGE ( 'NONE', *, *, #5755, .T. ) ;
#17109 = ORIENTED_EDGE ( 'NONE', *, *, #26179, .F. ) ;
#17110 = CARTESIAN_POINT ( 'NONE',  ( 854.0336774997908833, 1002.815270958697283, 1753.598338701302737 ) ) ;
#17111 = VECTOR ( 'NONE', #19486, 1000.000000000000000 ) ;
#17112 = EDGE_LOOP ( 'NONE', ( #7678, #11680, #12974, #12467 ) ) ;
#17113 = ORIENTED_EDGE ( 'NONE', *, *, #7892, .T. ) ;
#17114 = AXIS2_PLACEMENT_3D ( 'NONE', #28087, #22928, #25408 ) ;
#17115 = PLANE ( 'NONE',  #13543 ) ;
#17116 = B_SPLINE_CURVE_WITH_KNOTS ( 'NONE', 3,
 ( #28159, #9293, #20159, #31007, #6606, #17673 ),
 .UNSPECIFIED., .F., .F.,
 ( 4, 2, 4 ),
 ( 2.570076372265445214E-07, 0.001873455364168430219, 0.003746653720699633615 ),
 .UNSPECIFIED. ) ;
#17117 = DIRECTION ( 'NONE',  ( 0.000000000000000000, 1.000000000000000000, 5.145227585319922065E-49 ) ) ;
#17118 = ITEM_DEFINED_TRANSFORMATION ( 'NONE', 'NONE', #2431,  #28566 ) ;
#17119 = ORIENTED_EDGE ( 'NONE', *, *, #19494, .F. ) ;
#17120 = DIRECTION ( 'NONE',  ( 5.546364386991661285E-52, 0.000000000000000000, 1.000000000000000000 ) ) ;
#17121 = CARTESIAN_POINT ( 'NONE',  ( -414.0000000000000568, 137.0000000000000000, -155.0000000000000000 ) ) ;
#17122 = CONTEXT_DEPENDENT_SHAPE_REPRESENTATION ( #22647, #2201 ) ;
#17124 = PLANE ( 'NONE',  #2190 ) ;
#17123 = CARTESIAN_POINT ( 'NONE',  ( -12.00000000000001066, 108.9999999999999858, -155.0000000000000000 ) ) ;
#17126 = ORIENTED_EDGE ( 'NONE', *, *, #31834, .F. ) ;
#17125 = VECTOR ( 'NONE', #32592, 1000.000000000000000 ) ;
#17127 = ORIENTED_EDGE ( 'NONE', *, *, #1938, .F. ) ;
#17128 = LINE ( 'NONE', #3046, #20824 ) ;
#17129 = VECTOR ( 'NONE', #7747, 1000.000000000000000 ) ;
#17130 = B_SPLINE_CURVE_WITH_KNOTS ( 'NONE', 3,
 ( #25010, #645, #6141, #27863 ),
 .UNSPECIFIED., .F., .F.,
 ( 4, 4 ),
 ( 0.005298404680630666025, 0.005679541198217082261 ),
 .UNSPECIFIED. ) ;
#17131 = EDGE_CURVE ( 'NONE', #12639, #30526, #24874, .T. ) ;
#17132 = CARTESIAN_POINT ( 'NONE',  ( -449.9999999999999432, 105.0000000000000142, -175.0000000000000000 ) ) ;
#17133 = CARTESIAN_POINT ( 'NONE',  ( -70.00000000000000000, 75.55999999999990280, 172.9900000000000091 ) ) ;
#17134 = DIRECTION ( 'NONE',  ( 0.5611870653623829419, -0.8276889981568901211, -1.520440023423472285E-16 ) ) ;
#17135 = ORIENTED_EDGE ( 'NONE', *, *, #30865, .F. ) ;
#17136 = CARTESIAN_POINT ( 'NONE',  ( 22.89764159710611224, 17.63622956525712127, -77.50000000000000000 ) ) ;
#17137 = FACE_OUTER_BOUND ( 'NONE', #20526, .T. ) ;
#17138 = VERTEX_POINT ( 'NONE', #8863 ) ;
#17139 = CIRCLE ( 'NONE', #18248, 13.49999999999999822 ) ;
#17140 = ADVANCED_FACE ( 'NONE', ( #1035, #14579 ), #6357, .T. ) ;
#17141 = DIRECTION ( 'NONE',  ( -1.000000000000000000, -0.000000000000000000, -0.000000000000000000 ) ) ;
#17142 = FACE_OUTER_BOUND ( 'NONE', #562, .T. ) ;
#17143 = AXIS2_PLACEMENT_3D ( 'NONE', #20180, #776, #30316 ) ;
#17144 = DIRECTION ( 'NONE',  ( -1.000000000000000000, 0.000000000000000000, -0.000000000000000000 ) ) ;
#17146 = CARTESIAN_POINT ( 'NONE',  ( 0.000000000000000000, 3.004629197474321612E-15, 13.50000000000000000 ) ) ;
#17145 = DIRECTION ( 'NONE',  ( -0.000000000000000000, 0.08715574274766170471, 0.9961946980917453232 ) ) ;
#17147 = ADVANCED_FACE ( 'NONE', ( #22217 ), #27728, .T. ) ;
#17148 = UNCERTAINTY_MEASURE_WITH_UNIT (LENGTH_MEASURE( 1.000000000000000082E-05 ), #21935, 'distance_accuracy_value', 'NONE');
#17149 = CARTESIAN_POINT ( 'NONE',  ( 0.006892398596451419605, -11.06505884892015779, -28.81855237217609655 ) ) ;
#17150 = CYLINDRICAL_SURFACE ( 'NONE', #22805, 1.999999999999999112 ) ;
#17151 = VERTEX_POINT ( 'NONE', #22753 ) ;
#17152 = DIRECTION ( 'NONE',  ( -1.000000000000000000, 0.000000000000000000, 0.000000000000000000 ) ) ;
#17153 = FILL_AREA_STYLE_COLOUR ( '', #34251 ) ;
#17154 = PRODUCT_DEFINITION_SHAPE ( 'NONE', 'NONE',  #35137 ) ;
#17155 = EDGE_CURVE ( 'NONE', #12216, #33289, #25044, .T. ) ;
#17156 = EDGE_LOOP ( 'NONE', ( #10956, #34209, #20511, #3750 ) ) ;
#17157 = CIRCLE ( 'NONE', #6314, 11.22499999999999787 ) ;
#17158 = VECTOR ( 'NONE', #5160, 1000.000000000000000 ) ;
#17159 = AXIS2_PLACEMENT_3D ( 'NONE', #24941, #10562, #21413 ) ;
#17160 = VERTEX_POINT ( 'NONE', #33059 ) ;
#17161 = VERTEX_POINT ( 'NONE', #11366 ) ;
#17162 = FACE_OUTER_BOUND ( 'NONE', #15396, .T. ) ;
#17163 = ORIENTED_EDGE ( 'NONE', *, *, #3240, .F. ) ;
#17164 = VERTEX_POINT ( 'NONE', #27550 ) ;
#17165 = LINE ( 'NONE', #28528, #6541 ) ;
#17166 = AXIS2_PLACEMENT_3D ( 'NONE', #15721, #2171, #19393 ) ;
#17167 = ORIENTED_EDGE ( 'NONE', *, *, #7733, .T. ) ;
#17168 = CARTESIAN_POINT ( 'NONE',  ( 145.0000000000000568, -12.50000000000001066, 15.00000000000001243 ) ) ;
#17169 = DIRECTION ( 'NONE',  ( 0.000000000000000000, 1.836970198721029688E-16, -1.000000000000000000 ) ) ;
#17170 = VERTEX_POINT ( 'NONE', #28084 ) ;
#17171 = ORIENTED_EDGE ( 'NONE', *, *, #17332, .F. ) ;
#17172 = CARTESIAN_POINT ( 'NONE',  ( -28.23027531293552528, -10.15143121711728469, 20.00000000000000000 ) ) ;
#17173 = CARTESIAN_POINT ( 'NONE',  ( 2.719010680456189100, -0.5906890623665679296, -31.68904954958541609 ) ) ;
#17174 = B_SPLINE_CURVE_WITH_KNOTS ( 'NONE', 3,
 ( #4618, #31522, #23513, #7300, #26010, #20675 ),
 .UNSPECIFIED., .F., .F.,
 ( 4, 2, 4 ),
 ( 2.380729204601676866E-07, 0.003943479449179642000, 0.007886720825438824772 ),
 .UNSPECIFIED. ) ;
#17175 = CARTESIAN_POINT ( 'NONE',  ( 19.99999999999998224, -115.0000000000000000, -158.9999999999999716 ) ) ;
#17176 = DIRECTION ( 'NONE',  ( 0.000000000000000000, 0.000000000000000000, 1.000000000000000000 ) ) ;
#17177 = CARTESIAN_POINT ( 'NONE',  ( -6.500000000000000000, 0.000000000000000000, 0.000000000000000000 ) ) ;
#17178 = ORIENTED_EDGE ( 'NONE', *, *, #13965, .T. ) ;
#17179 = AXIS2_PLACEMENT_3D ( 'NONE', #29563, #7476, #29390 ) ;
#17180 = FACE_OUTER_BOUND ( 'NONE', #20263, .T. ) ;
#17181 = VECTOR ( 'NONE', #19358, 1000.000000000000000 ) ;
#17182 = DIRECTION ( 'NONE',  ( -1.000000000000000000, 6.792721752314501023E-48, -3.697785493223492838E-32 ) ) ;
#17183 = ORIENTED_EDGE ( 'NONE', *, *, #10963, .T. ) ;
#17184 = CIRCLE ( 'NONE', #14336, 3.999999999999989786 ) ;
#17185 = VECTOR ( 'NONE', #24553, 1000.000000000000000 ) ;
#17186 = AXIS2_PLACEMENT_3D ( 'NONE', #10116, #20978, #31817 ) ;
#17187 = DIRECTION ( 'NONE',  ( 1.000000000000000000, 0.000000000000000000, -0.000000000000000000 ) ) ;
#17188 = DIRECTION ( 'NONE',  ( -1.000000000000000000, -0.000000000000000000, -0.000000000000000000 ) ) ;
#17189 = DIRECTION ( 'NONE',  ( -1.000000000000000000, 0.000000000000000000, 0.000000000000000000 ) ) ;
#17190 = ADVANCED_FACE ( 'NONE', ( #3691 ), #11904, .F. ) ;
#17191 = CARTESIAN_POINT ( 'NONE',  ( 0.1835381243669127194, 21.48816195191864153, 24.07669289167355231 ) ) ;
#17192 = DIRECTION ( 'NONE',  ( -0.000000000000000000, -1.000000000000000000, -0.000000000000000000 ) ) ;
#17193 = EDGE_CURVE ( 'NONE', #18581, #21650, #29309, .T. ) ;
#17194 = EDGE_CURVE ( 'NONE', #10950, #10851, #1349, .T. ) ;
#17195 = CARTESIAN_POINT ( 'NONE',  ( 8.000000000000000000, 0.000000000000000000, 0.000000000000000000 ) ) ;
#17196 = EDGE_LOOP ( 'NONE', ( #1699, #23789, #19322, #4296 ) ) ;
#17197 = PLANE ( 'NONE',  #9338 ) ;
#17199 = CARTESIAN_POINT ( 'NONE',  ( -499.9999999999999432, -137.0000000000000000, -162.9999999999999716 ) ) ;
#17198 = CYLINDRICAL_SURFACE ( 'NONE', #27338, 2.000000000000001776 ) ;
#17200 = ORIENTED_EDGE ( 'NONE', *, *, #24178, .T. ) ;
#17201 =( REPRESENTATION_RELATIONSHIP ('NONE','NONE', #23037, #28231 ) REPRESENTATION_RELATIONSHIP_WITH_TRANSFORMATION ( #10889 )SHAPE_REPRESENTATION_RELATIONSHIP( ) );
#17202 = LINE ( 'NONE', #32833, #10342 ) ;
#17203 = PRODUCT_DEFINITION_SHAPE ( 'NONE', 'NONE',  #31842 ) ;
#17204 = CARTESIAN_POINT ( 'NONE',  ( -347.0000000000000000, -135.0000000000000000, 126.0000000000000000 ) ) ;
#17205 = ORIENTED_EDGE ( 'NONE', *, *, #17194, .T. ) ;
#17207 = ADVANCED_FACE ( 'NONE', ( #510 ), #338, .T. ) ;
#17206 = ORIENTED_EDGE ( 'NONE', *, *, #6166, .F. ) ;
#17208 = VECTOR ( 'NONE', #24868, 1000.000000000000000 ) ;
#17209 = AXIS2_PLACEMENT_3D ( 'NONE', #34276, #1706, #26090 ) ;
#17210 = AXIS2_PLACEMENT_3D ( 'NONE', #29862, #25024, #19360 ) ;
#17211 = ORIENTED_EDGE ( 'NONE', *, *, #6012, .T. ) ;
#17212 = CARTESIAN_POINT ( 'NONE',  ( 2.789999999999999147, -29.91351748324099091, -5.799410679710938155 ) ) ;
#17213 = ORIENTED_EDGE ( 'NONE', *, *, #3165, .T. ) ;
#17214 = ORIENTED_EDGE ( 'NONE', *, *, #6445, .T. ) ;
#17215 = DIRECTION ( 'NONE',  ( -1.300283923313630633E-47, 0.000000000000000000, -1.000000000000000000 ) ) ;
#17216 = EDGE_CURVE ( 'NONE', #10268, #8440, #20794, .T. ) ;
#17217 = DIRECTION ( 'NONE',  ( 0.000000000000000000, -1.000000000000000000, -2.132064625830773463E-16 ) ) ;
#17218 = ADVANCED_FACE ( 'NONE', ( #19732 ), #30585, .F. ) ;
#17219 = FACE_OUTER_BOUND ( 'NONE', #13357, .T. ) ;
#17220 = CARTESIAN_POINT ( 'NONE',  ( -37.71145559917817280, 3.353962854566122864, 15.81122994652406355 ) ) ;
#17221 = VERTEX_POINT ( 'NONE', #9575 ) ;
#17222 = EDGE_LOOP ( 'NONE', ( #2418, #14054, #16733, #9951 ) ) ;
#17223 = DIRECTION ( 'NONE',  ( -1.000000000000000000, -0.000000000000000000, -0.000000000000000000 ) ) ;
#17224 = DIRECTION ( 'NONE',  ( 0.000000000000000000, 1.000000000000000000, 1.934419779023891545E-16 ) ) ;
#17225 = CARTESIAN_POINT ( 'NONE',  ( -365.0000000000000000, -119.0000000000000000, 113.9999999999999858 ) ) ;
#17226 = EDGE_CURVE ( 'NONE', #23064, #17161, #25779, .T. ) ;
#17227 = DIRECTION ( 'NONE',  ( 0.000000000000000000, 0.000000000000000000, -1.000000000000000000 ) ) ;
#17228 = CYLINDRICAL_SURFACE ( 'NONE', #13139, 7.999999999999979572 ) ;
#17229 = FACE_OUTER_BOUND ( 'NONE', #13957, .T. ) ;
#17230 = CARTESIAN_POINT ( 'NONE',  ( -499.9999999999999432, 108.9999999999999858, -187.0000000000000000 ) ) ;
#17231 = ORIENTED_EDGE ( 'NONE', *, *, #32856, .T. ) ;
#17232 = CARTESIAN_POINT ( 'NONE',  ( -12.00000000000001066, -60.99999999999997158, -175.0000000000000000 ) ) ;
#17233 = CARTESIAN_POINT ( 'NONE',  ( 2.789999999999999147, -7.666252171205694133, 29.49034198003803198 ) ) ;
#17234 =( GEOMETRIC_REPRESENTATION_CONTEXT ( 3 ) GLOBAL_UNCERTAINTY_ASSIGNED_CONTEXT ( ( #17805 ) ) GLOBAL_UNIT_ASSIGNED_CONTEXT ( ( #19822, #6256, #11816 ) ) REPRESENTATION_CONTEXT ( 'NONE', 'WORKASPACE' ) );
#17235 = CARTESIAN_POINT ( 'NONE',  ( 2.789999999999999147, -25.83993731729781729, -18.77381338200996552 ) ) ;
#17236 = VERTEX_POINT ( 'NONE', #33778 ) ;
#17237=STYLED_ITEM('',(#35289),#34166);
#17238 = ADVANCED_FACE ( 'NONE', ( #9741 ), #20434, .F. ) ;
#17239 = ADVANCED_FACE ( 'NONE', ( #6711 ), #1558, .F. ) ;
#17240 = CIRCLE ( 'NONE', #7528, 32.54542015209057126 ) ;
#17241 = CARTESIAN_POINT ( 'NONE',  ( -449.9999999999999432, 104.9999999999999858, -162.9999999999999716 ) ) ;
#17242 = VERTEX_POINT ( 'NONE', #15097 ) ;
#17243 = CARTESIAN_POINT ( 'NONE',  ( 0.000000000000000000, 17.98401995359632011, 24.59729088254965035 ) ) ;
#17244 = EDGE_LOOP ( 'NONE', ( #31236, #3442, #24962, #31614 ) ) ;
#17245 = PLANE ( 'NONE',  #6346 ) ;
#17246 = CARTESIAN_POINT ( 'NONE',  ( -500.0000000000000000, -113.0000000000000000, -155.0000000000000000 ) ) ;
#17247 = DIRECTION ( 'NONE',  ( 1.000000000000000000, 0.000000000000000000, 0.000000000000000000 ) ) ;
#17248 = ORIENTED_EDGE ( 'NONE', *, *, #1651, .T. ) ;
#17249 = DIRECTION ( 'NONE',  ( -0.1148197344649410784, 0.9933863440662955568, -1.022897618519297264E-14 ) ) ;
#17250 = DIRECTION ( 'NONE',  ( -1.000000000000000000, -0.000000000000000000, -0.000000000000000000 ) ) ;
#17251 = ORIENTED_EDGE ( 'NONE', *, *, #6404, .F. ) ;
#17252 = CARTESIAN_POINT ( 'NONE',  ( -500.0000000000000000, 136.9999999999999432, -155.0000000000000000 ) ) ;
#17253 = EDGE_CURVE ( 'NONE', #33693, #2489, #16172, .T. ) ;
#17254 = AXIS2_PLACEMENT_3D ( 'NONE', #7481, #13552, #29396 ) ;
#17255 = CARTESIAN_POINT ( 'NONE',  ( -12.00000000000001066, -112.9999999999999858, -155.0000000000000284 ) ) ;
#17256 = EDGE_CURVE ( 'NONE', #7553, #18186, #12432, .T. ) ;
#17257 = VECTOR ( 'NONE', #9717, 1000.000000000000000 ) ;
#17258 = CARTESIAN_POINT ( 'NONE',  ( 0.02407890056655695096, -26.45933846664205902, 16.32596387352436551 ) ) ;
#17259 = PLANE ( 'NONE',  #17114 ) ;
#17260 = TOROIDAL_SURFACE ( 'NONE', #26318, 30.47050528711512030, 8.000000000000000000 ) ;
#17261 = VERTEX_POINT ( 'NONE', #4029 ) ;
#17262 = ORIENTED_EDGE ( 'NONE', *, *, #2309, .T. ) ;
#17263 = VECTOR ( 'NONE', #28380, 1000.000000000000000 ) ;
#17264 = ORIENTED_EDGE ( 'NONE', *, *, #27258, .F. ) ;
#17265 = DIRECTION ( 'NONE',  ( -0.5155538571770218459, 0.8568571761675891629, -0.000000000000000000 ) ) ;
#17266 = DIRECTION ( 'NONE',  ( 0.000000000000000000, 0.000000000000000000, 1.000000000000000000 ) ) ;
#17267 = CARTESIAN_POINT ( 'NONE',  ( -500.0000000000000000, -137.0000000000000000, 162.9999999999999716 ) ) ;
#17268 = ORIENTED_EDGE ( 'NONE', *, *, #26717, .F. ) ;
#17269 = ORIENTED_EDGE ( 'NONE', *, *, #6856, .T. ) ;
#17270 = LINE ( 'NONE', #4045, #3241 ) ;
#17271 = CARTESIAN_POINT ( 'NONE',  ( -6.500000000000000000, 0.000000000000000000, -0.7500000000000000000 ) ) ;
#17272 = ORIENTED_EDGE ( 'NONE', *, *, #32043, .T. ) ;
#17273 = EDGE_CURVE ( 'NONE', #33070, #35069, #23279, .T. ) ;
#17274 = CARTESIAN_POINT ( 'NONE',  ( -37.69926482250235722, 3.578808500140873150, 16.17202516343389007 ) ) ;
#17275 = LINE ( 'NONE', #11925, #4054 ) ;
#17276 = ORIENTED_EDGE ( 'NONE', *, *, #19862, .F. ) ;
#17277 = ORIENTED_EDGE ( 'NONE', *, *, #24304, .T. ) ;
#17278 = CIRCLE ( 'NONE', #15555, 32.54542015209054284 ) ;
#17279 = CARTESIAN_POINT ( 'NONE',  ( 11.99999999999999645, 108.9999999999999858, 155.0000000000000000 ) ) ;
#17280 = EDGE_LOOP ( 'NONE', ( #4784, #30450, #885, #11025 ) ) ;
#17281 = CARTESIAN_POINT ( 'NONE',  ( -35.00000000000000000, -38.34433698000722046, -36.69637551990492597 ) ) ;
#17282 = CARTESIAN_POINT ( 'NONE',  ( 11.99999999999999645, -145.0000000000000000, -162.9999999999999432 ) ) ;
#17283 = LINE ( 'NONE', #3372, #28619 ) ;
#17284 = AXIS2_PLACEMENT_3D ( 'NONE', #3510, #11541, #14400 ) ;
#17285 = AXIS2_PLACEMENT_3D ( 'NONE', #9154, #6652, #3806 ) ;
#17286 = VECTOR ( 'NONE', #30964, 1000.000000000000000 ) ;
#17287 = CARTESIAN_POINT ( 'NONE',  ( -100.8451065690243951, -2.987912174852660474, 12.13846169321888979 ) ) ;
#17288 = DIRECTION ( 'NONE',  ( -3.469446951953832974E-18, -1.000000000000000000, -7.888609052210116302E-31 ) ) ;
#17289 = ADVANCED_FACE ( 'NONE', ( #9915 ), #25577, .T. ) ;
#17290 = DIRECTION ( 'NONE',  ( -0.000000000000000000, 0.000000000000000000, 1.000000000000000000 ) ) ;
#17291 = VERTEX_POINT ( 'NONE', #25759 ) ;
#17292 = ORIENTED_EDGE ( 'NONE', *, *, #31529, .T. ) ;
#17293 = DIRECTION ( 'NONE',  ( 2.631201909438060269E-14, -5.396010391056495992E-16, 0.9999999999999998890 ) ) ;
#17294 = ORIENTED_EDGE ( 'NONE', *, *, #19414, .T. ) ;
#17295 = ORIENTED_EDGE ( 'NONE', *, *, #19368, .F. ) ;
#17296 = EDGE_CURVE ( 'NONE', #33041, #12035, #25942, .T. ) ;
#17297 = EDGE_CURVE ( 'NONE', #27275, #28991, #12258, .T. ) ;
#17298 = CARTESIAN_POINT ( 'NONE',  ( 0.000000000000000000, -33.69708579775584667, 49.43553178847298568 ) ) ;
#17299 = EDGE_CURVE ( 'NONE', #726, #8847, #12598, .T. ) ;
#17300 = AXIS2_PLACEMENT_3D ( 'NONE', #33247, #9043, #27901 ) ;
#17301 = CARTESIAN_POINT ( 'NONE',  ( 143.0000000000000568, -45.49999999999999289, 51.88904920397793319 ) ) ;
#17302 = ORIENTED_EDGE ( 'NONE', *, *, #31968, .F. ) ;
#17303 = CARTESIAN_POINT ( 'NONE',  ( -442.0000000000000000, 141.0000000000000000, -175.0000000000000000 ) ) ;
#17304 = CARTESIAN_POINT ( 'NONE',  ( 8.485274312747504766, 31.41981051364775013, 68.31122994652405112 ) ) ;
#17305 = AXIS2_PLACEMENT_3D ( 'NONE', #2329, #18736, #26184 ) ;
#17306 = B_SPLINE_CURVE_WITH_KNOTS ( 'NONE', 3,
 ( #20100, #30944, #4399, #1909, #22935, #15289 ),
 .UNSPECIFIED., .F., .F.,
 ( 4, 2, 4 ),
 ( 4.404817051633169802E-07, 0.001874269637237882926, 0.003748098792770602258 ),
 .UNSPECIFIED. ) ;
#17308 = CARTESIAN_POINT ( 'NONE',  ( -20.63749999999999574, 1.959434878635765131E-15, 16.00000000000000000 ) ) ;
#17307 = DIRECTION ( 'NONE',  ( -0.000000000000000000, 1.000000000000000000, -0.000000000000000000 ) ) ;
#17309 = VECTOR ( 'NONE', #3063, 1000.000000000000000 ) ;
#17310 = ORIENTED_EDGE ( 'NONE', *, *, #9489, .T. ) ;
#17311 = VERTEX_POINT ( 'NONE', #26283 ) ;
#17312 = AXIS2_PLACEMENT_3D ( 'NONE', #35042, #2628, #2798 ) ;
#17313 = CARTESIAN_POINT ( 'NONE',  ( -410.0000000000000568, 113.0000000000000000, -155.0000000000000000 ) ) ;
#17314 = CYLINDRICAL_SURFACE ( 'NONE', #32363, 3.999999999999948042 ) ;
#17315 = CARTESIAN_POINT ( 'NONE',  ( -418.0000000000000000, 104.9999999999999858, -175.0000000000000000 ) ) ;
#17316 = CARTESIAN_POINT ( 'NONE',  ( -418.0000000000000000, -124.9999999999999858, -77.99999999999997158 ) ) ;
#17317 = ORIENTED_EDGE ( 'NONE', *, *, #10577, .F. ) ;
#17318 = DIRECTION ( 'NONE',  ( -1.000000000000000000, 0.000000000000000000, 0.000000000000000000 ) ) ;
#17319 = FACE_OUTER_BOUND ( 'NONE', #27677, .T. ) ;
#17320 = ORIENTED_EDGE ( 'NONE', *, *, #10037, .F. ) ;
#17321 = DIRECTION ( 'NONE',  ( 0.000000000000000000, 0.000000000000000000, -1.000000000000000000 ) ) ;
#17322 = CARTESIAN_POINT ( 'NONE',  ( -347.0000000000000000, -125.0000000000000284, 168.9999999999999716 ) ) ;
#17323 = CARTESIAN_POINT ( 'NONE',  ( -28.00450684652666311, 16.58167570419054115, 68.31122994652405112 ) ) ;
#17325 = CARTESIAN_POINT ( 'NONE',  ( 11.99999999999999645, 134.9999999999999432, -194.9999999999999432 ) ) ;
#17324 = CARTESIAN_POINT ( 'NONE',  ( -12.00000000000001066, -124.9999999999999432, -154.9999999999999716 ) ) ;
#17326 = AXIS2_PLACEMENT_3D ( 'NONE', #15804, #26636, #10628 ) ;
#17327 = DIRECTION ( 'NONE',  ( 2.891205793294675368E-16, 0.000000000000000000, -1.000000000000000000 ) ) ;
#17328 = CARTESIAN_POINT ( 'NONE',  ( 0.02407890056655781832, 31.00221527374952046, -2.344426712874310148 ) ) ;
#17329 = ORIENTED_EDGE ( 'NONE', *, *, #8407, .T. ) ;
#17330 = DIRECTION ( 'NONE',  ( 0.000000000000000000, -1.000000000000000000, 0.000000000000000000 ) ) ;
#17331 = VECTOR ( 'NONE', #15769, 1000.000000000000000 ) ;
#17332 = EDGE_CURVE ( 'NONE', #11445, #1780, #13778, .T. ) ;
#17334 = ORIENTED_EDGE ( 'NONE', *, *, #17689, .T. ) ;
#17333 = VECTOR ( 'NONE', #13061, 1000.000000000000000 ) ;
#17335 = AXIS2_PLACEMENT_3D ( 'NONE', #4454, #23692, #26173 ) ;
#17336 =( NAMED_UNIT ( * ) PLANE_ANGLE_UNIT ( ) SI_UNIT ( $, .RADIAN. ) );
#17337 = EDGE_CURVE ( 'NONE', #21866, #30042, #23441, .T. ) ;
#17338 = VECTOR ( 'NONE', #33506, 1000.000000000000227 ) ;
#17339 = EDGE_LOOP ( 'NONE', ( #27742, #8477, #27793, #30665 ) ) ;
#17340 = EDGE_CURVE ( 'NONE', #23628, #35, #28611, .T. ) ;
#17341 = ADVANCED_FACE ( 'NONE', ( #4548 ), #1896, .T. ) ;
#17342 = ORIENTED_EDGE ( 'NONE', *, *, #9790, .T. ) ;
#17343 = CARTESIAN_POINT ( 'NONE',  ( -442.0000000000000000, -109.0000000000000142, -155.0000000000000000 ) ) ;
#17344 = VERTEX_POINT ( 'NONE', #20950 ) ;
#17345 = ORIENTED_EDGE ( 'NONE', *, *, #9991, .T. ) ;
#17346 = EDGE_CURVE ( 'NONE', #33253, #34878, #6538, .T. ) ;
#17347 = CARTESIAN_POINT ( 'NONE',  ( 11.99999999999999645, 144.9999999999999716, 155.0000000000000000 ) ) ;
#17348 = CIRCLE ( 'NONE', #13348, 3.999999999999948042 ) ;
#17349 = ORIENTED_EDGE ( 'NONE', *, *, #17797, .F. ) ;
#17350 = DIRECTION ( 'NONE',  ( -3.469446951953832974E-18, -1.000000000000000000, -7.888609052210116302E-31 ) ) ;
#17351 = LINE ( 'NONE', #33343, #18309 ) ;
#17352 = ORIENTED_EDGE ( 'NONE', *, *, #14271, .F. ) ;
#17353 = ORIENTED_EDGE ( 'NONE', *, *, #3680, .F. ) ;
#17354 = DIRECTION ( 'NONE',  ( -0.000000000000000000, -0.000000000000000000, 1.000000000000000000 ) ) ;
#17355 = DIRECTION ( 'NONE',  ( 0.6051742151937647973, -0.7960930657056438653, -0.000000000000000000 ) ) ;
#17356 = AXIS2_PLACEMENT_3D ( 'NONE', #19226, #24886, #5659 ) ;
#17357 = EDGE_CURVE ( 'NONE', #2971, #13032, #14754, .T. ) ;
#17358 = DIRECTION ( 'NONE',  ( 0.000000000000000000, 0.000000000000000000, -1.000000000000000000 ) ) ;
#17359 = LINE ( 'NONE', #10811, #1728 ) ;
#17360 = DIRECTION ( 'NONE',  ( -0.000000000000000000, -0.000000000000000000, 1.000000000000000000 ) ) ;
#17361 = EDGE_LOOP ( 'NONE', ( #6477, #12897, #6944, #14203 ) ) ;
#17362 = VERTEX_POINT ( 'NONE', #18596 ) ;
#17363 = PLANE ( 'NONE',  #5423 ) ;
#17364 = AXIS2_PLACEMENT_3D ( 'NONE', #27536, #31853, #18364 ) ;
#17365 = CIRCLE ( 'NONE', #10535, 4.750000000000004441 ) ;
#17366 = PLANE ( 'NONE',  #32917 ) ;
#17367 = ORIENTED_EDGE ( 'NONE', *, *, #32344, .F. ) ;
#17368 = PRODUCT_DEFINITION_SHAPE ( 'NONE', 'NONE',  #35238 ) ;
#17369 = AXIS2_PLACEMENT_3D ( 'NONE', #6882, #9407, #4214 ) ;
#17370 = FACE_OUTER_BOUND ( 'NONE', #24683, .T. ) ;
#17371 = CARTESIAN_POINT ( 'NONE',  ( -414.0000000000000568, -112.9999999999999858, -155.0000000000000000 ) ) ;
#17372 = PLANE ( 'NONE',  #32575 ) ;
#17373 = CARTESIAN_POINT ( 'NONE',  ( 104.0198594782632853, 5.657025933901884684, -4.924586583110066584 ) ) ;
#17374 = CARTESIAN_POINT ( 'NONE',  ( -12.00000000000001066, -64.99999999999997158, -154.9999999999999716 ) ) ;
#17375 = DIRECTION ( 'NONE',  ( 0.000000000000000000, 0.000000000000000000, 1.000000000000000000 ) ) ;
#17376 = VERTEX_POINT ( 'NONE', #14926 ) ;
#17377 = CARTESIAN_POINT ( 'NONE',  ( -19.99999999999998934, 112.9999999999999574, -155.0000000000000000 ) ) ;
#17379 = FACE_OUTER_BOUND ( 'NONE', #8425, .T. ) ;
#17378 = CARTESIAN_POINT ( 'NONE',  ( -12.00000000000003908, -134.9999999999999716, -194.9999999999999432 ) ) ;
#17380 = AXIS2_PLACEMENT_3D ( 'NONE', #14839, #28696, #9490 ) ;
#17381 = ORIENTED_EDGE ( 'NONE', *, *, #34882, .F. ) ;
#17382 = DIRECTION ( 'NONE',  ( 0.000000000000000000, 6.123233995736766036E-17, 1.000000000000000000 ) ) ;
#17383 = AXIS2_PLACEMENT_3D ( 'NONE', #15245, #14730, #25733 ) ;
#17384 = ORIENTED_EDGE ( 'NONE', *, *, #5480, .T. ) ;
#17385 = ORIENTED_EDGE ( 'NONE', *, *, #33137, .F. ) ;
#17386 = EDGE_CURVE ( 'NONE', #31534, #16134, #18938, .T. ) ;
#17387 = AXIS2_PLACEMENT_3D ( 'NONE', #17246, #8674, #11718 ) ;
#17388 = VECTOR ( 'NONE', #6488, 1000.000000000000000 ) ;
#17389 = ORIENTED_EDGE ( 'NONE', *, *, #19936, .F. ) ;
#17390 = CARTESIAN_POINT ( 'NONE',  ( 104.8009589134950232, -5.738006884272855324, -4.829624934769205069 ) ) ;
#17391 = ORIENTED_EDGE ( 'NONE', *, *, #29825, .T. ) ;
#17392 = ORIENTED_EDGE ( 'NONE', *, *, #10487, .T. ) ;
#17393 = ADVANCED_FACE ( 'NONE', ( #23108 ), #16329, .T. ) ;
#17394 = CARTESIAN_POINT ( 'NONE',  ( -499.9999999999999432, -113.0000000000000000, -155.0000000000000000 ) ) ;
#17395 = CLOSED_SHELL ( 'NONE', ( #15927, #34029, #21377, #32004, #25151, #29491, #20971, #30392, #5562, #6657, #24997, #8307, #20820, #27883, #15678, #30473, #21980, #14151, #8269, #656, #32649, #28967, #28307, #21969, #32578, #14025, #14975, #23242, #28890, #13860, #35013, #23309, #20730, #30979, #15290, #10079, #32519, #4839, #2808, #19593, #8630, #26565, #2591, #21644, #19943, #31121, #19581, #8249, #1201, #5685, #34578, #25801, #12587, #15274, #14734, #24200, #15118, #30173, #23378, #26341, #24764, #7403, #28335, #20880, #3768, #17055, #32825, #33248, #30366, #24599, #26625, #25383, #12841, #16161, #3801, #10231, #19950, #27827, #6411, #39, #34555, #12541, #18541, #5249, #25235, #28918, #3118, #34155, #34286, #16497, #15212, #165, #17207, #29880, #31526, #28856, #13667, #32348, #5652, #27388, #17466, #25089 ) ) ;
#17396 = ADVANCED_FACE ( 'NONE', ( #5256 ), #26458, .T. ) ;
#17397 = CARTESIAN_POINT ( 'NONE',  ( 0.1859802947979261878, -11.11575656128866463, 30.30758796111447850 ) ) ;
#17398 = DIRECTION ( 'NONE',  ( 0.000000000000000000, 0.000000000000000000, 1.000000000000000000 ) ) ;
#17399 = DIRECTION ( 'NONE',  ( 1.000000000000000000, -3.540705920434608777E-32, 2.891205793294675368E-16 ) ) ;
#17400 = EDGE_CURVE ( 'NONE', #14255, #24525, #15625, .T. ) ;
#17401 = ORIENTED_EDGE ( 'NONE', *, *, #28256, .T. ) ;
#17402 = ADVANCED_FACE ( 'NONE', ( #23795, #13299, #18816 ), #10970, .F. ) ;
#17403 = VERTEX_POINT ( 'NONE', #13640 ) ;
#17404 = CARTESIAN_POINT ( 'NONE',  ( 37.86520737902618805, 0.5181781365365116798, 68.31122994652405112 ) ) ;
#17405 = DIRECTION ( 'NONE',  ( 1.000000000000000000, 0.000000000000000000, -1.232595164407831220E-32 ) ) ;
#17406 = CARTESIAN_POINT ( 'NONE',  ( 29.44023756548695658, 13.87360028845404614, 68.31122994652405112 ) ) ;
#17407 = DIRECTION ( 'NONE',  ( 1.000000000000000000, -0.000000000000000000, -0.000000000000000000 ) ) ;
#17408 = DIRECTION ( 'NONE',  ( -1.000000000000000000, -0.000000000000000000, 0.000000000000000000 ) ) ;
#17409 = VECTOR ( 'NONE', #9787, 1000.000000000000000 ) ;
#17410 = DIRECTION ( 'NONE',  ( 1.000000000000000000, 0.000000000000000000, 0.000000000000000000 ) ) ;
#17411 = DIRECTION ( 'NONE',  ( 1.000000000000000000, 0.000000000000000000, -0.000000000000000000 ) ) ;
#17412 = ORIENTED_EDGE ( 'NONE', *, *, #21002, .F. ) ;
#17413 = VECTOR ( 'NONE', #11841, 999.9999999999998863 ) ;
#17414 = CARTESIAN_POINT ( 'NONE',  ( -99.88497961182919482, 6.264093345946821604E-16, 12.50000000000000000 ) ) ;
#17415 = PLANE ( 'NONE',  #1802 ) ;
#17416 = EDGE_CURVE ( 'NONE', #33601, #19123, #29792, .T. ) ;
#17417 = LINE ( 'NONE', #22735, #26300 ) ;
#17418 = ORIENTED_EDGE ( 'NONE', *, *, #30777, .F. ) ;
#17419 =( REPRESENTATION_RELATIONSHIP ('NONE','NONE', #23037, #28231 ) REPRESENTATION_RELATIONSHIP_WITH_TRANSFORMATION ( #13125 )SHAPE_REPRESENTATION_RELATIONSHIP( ) );
#17420 = FACE_OUTER_BOUND ( 'NONE', #5923, .T. ) ;
#17421 = EDGE_LOOP ( 'NONE', ( #973, #19497, #11942, #15188 ) ) ;
#17422 = CARTESIAN_POINT ( 'NONE',  ( -500.0000000000000000, -137.0000000000000000, 155.0000000000000000 ) ) ;
#17424 = VECTOR ( 'NONE', #1453, 1000.000000000000000 ) ;
#17423 = DIRECTION ( 'NONE',  ( 0.000000000000000000, 1.836970198721029441E-16, -1.000000000000000000 ) ) ;
#17425 = EDGE_CURVE ( 'NONE', #404, #26887, #16730, .T. ) ;
#17426 = EDGE_CURVE ( 'NONE', #16592, #32672, #26812, .T. ) ;
#17427 = VERTEX_POINT ( 'NONE', #29490 ) ;
#17428 = LINE ( 'NONE', #8854, #31900 ) ;
#17429 = LINE ( 'NONE', #3157, #11681 ) ;
#17430 = DIRECTION ( 'NONE',  ( 1.000000000000000000, 0.000000000000000000, 0.000000000000000000 ) ) ;
#17431 = ORIENTED_EDGE ( 'NONE', *, *, #2174, .T. ) ;
#17432 = VECTOR ( 'NONE', #34796, 999.9999999999998863 ) ;
#17433 = DIRECTION ( 'NONE',  ( -4.463897479543275529E-14, -4.880182949497472857E-14, 1.000000000000000000 ) ) ;
#17434 = FACE_OUTER_BOUND ( 'NONE', #23390, .T. ) ;
#17435 = VERTEX_POINT ( 'NONE', #31794 ) ;
#17436 = AXIS2_PLACEMENT_3D ( 'NONE', #31988, #7956, #7597 ) ;
#17437 = CARTESIAN_POINT ( 'NONE',  ( 2.789999999999999147, 17.11426446101236820, -24.44276559937708271 ) ) ;
#17438 = DIRECTION ( 'NONE',  ( 0.000000000000000000, 0.000000000000000000, 1.000000000000000000 ) ) ;
#17439 = DIRECTION ( 'NONE',  ( 0.000000000000000000, -1.224646799147353207E-16, 1.000000000000000000 ) ) ;
#17440 = CARTESIAN_POINT ( 'NONE',  ( -499.9999999999999432, 112.9999999999999574, 162.9999999999999716 ) ) ;
#17441 = EDGE_CURVE ( 'NONE', #34959, #26754, #7042, .T. ) ;
#17442 = ORIENTED_EDGE ( 'NONE', *, *, #22146, .T. ) ;
#17443 = EDGE_CURVE ( 'NONE', #30046, #23843, #22941, .T. ) ;
#17444 = EDGE_LOOP ( 'NONE', ( #15419, #518, #7966, #21082, #15024, #28910, #28496, #9315, #3735, #20905, #3819, #20402, #18353, #30920, #24445, #27932 ) ) ;
#17445 = ORIENTED_EDGE ( 'NONE', *, *, #29088, .T. ) ;
#17446 =( GEOMETRIC_REPRESENTATION_CONTEXT ( 3 ) GLOBAL_UNCERTAINTY_ASSIGNED_CONTEXT ( ( #18439 ) ) GLOBAL_UNIT_ASSIGNED_CONTEXT ( ( #22430, #11226, #22076 ) ) REPRESENTATION_CONTEXT ( 'NONE', 'WORKASPACE' ) );
#17447 = EDGE_CURVE ( 'NONE', #469, #28125, #8114, .T. ) ;
#17448 = DIRECTION ( 'NONE',  ( -1.000000000000000000, 0.000000000000000000, 0.000000000000000000 ) ) ;
#17449 = LINE ( 'NONE', #3874, #30974 ) ;
#17450 = DIRECTION ( 'NONE',  ( -1.000000000000000000, -0.000000000000000000, -0.000000000000000000 ) ) ;
#17451 = EDGE_LOOP ( 'NONE', ( #10048, #29165, #16289, #11038 ) ) ;
#17452 = CARTESIAN_POINT ( 'NONE',  ( 0.1859802683305686877, 19.63342256285821463, 25.62496134208834775 ) ) ;
#17453 = DIRECTION ( 'NONE',  ( 0.000000000000000000, 1.000000000000000000, 5.145227585319922065E-49 ) ) ;
#17454 = ORIENTED_EDGE ( 'NONE', *, *, #17216, .T. ) ;
#17455 = PRODUCT_DEFINITION_SHAPE ( 'NONE', 'NONE',  #35165 ) ;
#17456 = LINE ( 'NONE', #11498, #26577 ) ;
#17457 = DIRECTION ( 'NONE',  ( 0.000000000000000000, 0.000000000000000000, 1.000000000000000000 ) ) ;
#17458 = ORIENTED_EDGE ( 'NONE', *, *, #17256, .F. ) ;
#17459 = VECTOR ( 'NONE', #4437, 1000.000000000000000 ) ;
#17460 = DIRECTION ( 'NONE',  ( -0.000000000000000000, 1.000000000000000000, -0.000000000000000000 ) ) ;
#17461 = CARTESIAN_POINT ( 'NONE',  ( -19.99999999999998934, 136.9999999999999716, -175.0000000000000284 ) ) ;
#17462 = VERTEX_POINT ( 'NONE', #29317 ) ;
#17463 = CIRCLE ( 'NONE', #33331, 7.999999999999979572 ) ;
#17464 = CARTESIAN_POINT ( 'NONE',  ( 1.040000000000000258, -18.66807150955433769, 28.91175816027496381 ) ) ;
#17465 = CARTESIAN_POINT ( 'NONE',  ( -5.021133111224679091, 28.08988295778447508, -87.50000000000000000 ) ) ;
#17466 = ADVANCED_FACE ( 'NONE', ( #13121 ), #2079, .F. ) ;
#17467 = CARTESIAN_POINT ( 'NONE',  ( -442.0000000000000000, 104.9999999999999858, -162.9999999999999716 ) ) ;
#17468 = EDGE_CURVE ( 'NONE', #8951, #32109, #2597, .T. ) ;
#17469 = EDGE_CURVE ( 'NONE', #2593, #25686, #16148, .T. ) ;
#17470 = CARTESIAN_POINT ( 'NONE',  ( -99.88497961182919482, 6.264093345946821604E-16, 12.50000000000000000 ) ) ;
#17471 = CARTESIAN_POINT ( 'NONE',  ( 0.000000000000000000, 3.524919873834583163E-15, 68.31122994652405112 ) ) ;
#17472 = CARTESIAN_POINT ( 'NONE',  ( 1.749999999999999778, -1.891117961019737725, -34.36292081097834483 ) ) ;
#17473 = AXIS2_PLACEMENT_3D ( 'NONE', #9160, #12205, #6480 ) ;
#17474 = ADVANCED_FACE ( 'NONE', ( #10443 ), #4908, .F. ) ;
#17475 = ORIENTED_EDGE ( 'NONE', *, *, #24145, .T. ) ;
#17476 = EDGE_CURVE ( 'NONE', #25273, #15499, #32492, .T. ) ;
#17477 = ORIENTED_EDGE ( 'NONE', *, *, #13187, .T. ) ;
#17478 = DIRECTION ( 'NONE',  ( -0.1063910735369017202, 0.9943243633099136947, -1.000770725407181676E-14 ) ) ;
#17479 = EDGE_CURVE ( 'NONE', #16, #21237, #33765, .T. ) ;
#17480 = VERTEX_POINT ( 'NONE', #19874 ) ;
#17481 = VECTOR ( 'NONE', #12840, 1000.000000000000000 ) ;
#17482 = DIRECTION ( 'NONE',  ( -0.000000000000000000, 1.000000000000000000, -0.000000000000000000 ) ) ;
#17483 = VECTOR ( 'NONE', #16390, 1000.000000000000000 ) ;
#17484 = DIRECTION ( 'NONE',  ( 0.000000000000000000, 0.000000000000000000, -1.000000000000000000 ) ) ;
#17485 = ORIENTED_EDGE ( 'NONE', *, *, #33581, .T. ) ;
#17486 = CARTESIAN_POINT ( 'NONE',  ( -430.0000000000000000, -131.0000000000000000, 113.9999999999999858 ) ) ;
#17487 = CARTESIAN_POINT ( 'NONE',  ( -105.3361376941048064, -5.115085776248457172, -11.40552048381710115 ) ) ;
#17489 = LINE ( 'NONE', #14634, #16983 ) ;
#17488 = DIRECTION ( 'NONE',  ( 1.000000000000000000, 0.000000000000000000, 0.000000000000000000 ) ) ;
#17490 = EDGE_LOOP ( 'NONE', ( #33824, #27165, #31441, #2246 ) ) ;
#17491 = VERTEX_POINT ( 'NONE', #8471 ) ;
#17492 = CARTESIAN_POINT ( 'NONE',  ( -35.00000000000000000, 42.49491490430484220, -36.69637551990492597 ) ) ;
#17493 = AXIS2_PLACEMENT_3D ( 'NONE', #16864, #32676, #6140 ) ;
#17494 = DIRECTION ( 'NONE',  ( 0.000000000000000000, 0.000000000000000000, 1.000000000000000000 ) ) ;
#17495 = DIRECTION ( 'NONE',  ( 0.000000000000000000, 0.000000000000000000, -1.000000000000000000 ) ) ;
#17496 = EDGE_LOOP ( 'NONE', ( #12712, #20174, #27967, #22459, #23657, #25320 ) ) ;
#17497 = DIRECTION ( 'NONE',  ( 1.000000000000000000, 0.000000000000000000, 0.000000000000000000 ) ) ;
#17498 = CARTESIAN_POINT ( 'NONE',  ( -355.0000000000000000, 130.9999999999999716, 113.9999999999999858 ) ) ;
#17499 = PRODUCT_DEFINITION_SHAPE ( 'NONE', 'NONE',  #35105 ) ;
#17500 = EDGE_LOOP ( 'NONE', ( #19619, #26027, #12727, #105, #17920, #15673 ) ) ;
#17501 = DIRECTION ( 'NONE',  ( 0.000000000000000000, -1.000000000000000000, -1.836970198721029688E-16 ) ) ;
#17502 = FACE_BOUND ( 'NONE', #30186, .T. ) ;
#17503 = CARTESIAN_POINT ( 'NONE',  ( 29.63313772848249883, -13.45665341906702395, 49.43553178847298568 ) ) ;
#17504 = ADVANCED_FACE ( 'NONE', ( #6310, #19339 ), #30716, .T. ) ;
#17506 = CARTESIAN_POINT ( 'NONE',  ( -8.000000000000000000, 1.445083222993876839E-15, 11.79999999999999893 ) ) ;
#17505 = DIRECTION ( 'NONE',  ( 1.000000000000000000, 0.000000000000000000, 5.546364386991661285E-52 ) ) ;
#17507 = AXIS2_PLACEMENT_3D ( 'NONE', #24849, #484, #18831 ) ;
#17508 = AXIS2_PLACEMENT_3D ( 'NONE', #10905, #24772, #11086 ) ;
#17509 = EDGE_CURVE ( 'NONE', #1134, #22879, #27508, .T. ) ;
#17510 = CYLINDRICAL_SURFACE ( 'NONE', #15590, 9.999999999999994671 ) ;
#17511 = CARTESIAN_POINT ( 'NONE',  ( 8.927936315454026328, -31.29690601358698387, -36.68877005347593467 ) ) ;
#17512 = ORIENTED_EDGE ( 'NONE', *, *, #31300, .T. ) ;
#17513 = CARTESIAN_POINT ( 'NONE',  ( 2.789999999999999147, 7.489092610871091793, 29.53582882395389930 ) ) ;
#17514 = FACE_OUTER_BOUND ( 'NONE', #22092, .T. ) ;
#17515 = CIRCLE ( 'NONE', #29981, 44.99999999999998579 ) ;
#17516 = VERTEX_POINT ( 'NONE', #30356 ) ;
#17517 = ORIENTED_EDGE ( 'NONE', *, *, #4972, .F. ) ;
#17518 = ORIENTED_EDGE ( 'NONE', *, *, #27807, .T. ) ;
#17519 = AXIS2_PLACEMENT_3D ( 'NONE', #466, #32839, #30899 ) ;
#17520 = DIRECTION ( 'NONE',  ( 0.000000000000000000, 0.000000000000000000, -1.000000000000000000 ) ) ;
#17521 = ORIENTED_EDGE ( 'NONE', *, *, #24615, .F. ) ;
#17522 = ORIENTED_EDGE ( 'NONE', *, *, #1370, .F. ) ;
#17523 = ORIENTED_EDGE ( 'NONE', *, *, #24560, .F. ) ;
#17524 = CARTESIAN_POINT ( 'NONE',  ( -34.66645501699844090, -15.21971901163155216, 68.31122994652405112 ) ) ;
#17525 = AXIS2_PLACEMENT_3D ( 'NONE', #18692, #32009, #10671 ) ;
#17526 = AXIS2_PLACEMENT_3D ( 'NONE', #18716, #29556, #7120 ) ;
#17527 = EDGE_LOOP ( 'NONE', ( #11750, #16665 ) ) ;
#17528 = LINE ( 'NONE', #20004, #15834 ) ;
#17529 = FACE_BOUND ( 'NONE', #23802, .T. ) ;
#17530 = VERTEX_POINT ( 'NONE', #11686 ) ;
#17531 = VERTEX_POINT ( 'NONE', #11502 ) ;
#17532 = CARTESIAN_POINT ( 'NONE',  ( 8.485274312747499437, 31.41981051364775013, 68.31122994652405112 ) ) ;
#17533 = DIRECTION ( 'NONE',  ( -0.000000000000000000, 0.000000000000000000, -1.000000000000000000 ) ) ;
#17534 = DIRECTION ( 'NONE',  ( -1.000000000000000000, 0.000000000000000000, 0.000000000000000000 ) ) ;
#17535 = CARTESIAN_POINT ( 'NONE',  ( 11.99999999999999645, 124.9999999999999716, 155.0000000000000000 ) ) ;
#17536 = CARTESIAN_POINT ( 'NONE',  ( 1.040000000000000036, 14.40815186467775533, 31.25366880301323746 ) ) ;
#17537 = VERTEX_POINT ( 'NONE', #32843 ) ;
#17538 = CARTESIAN_POINT ( 'NONE',  ( -20.00000000000007461, 104.9999999999999858, 162.9999999999999716 ) ) ;
#17539 = DIRECTION ( 'NONE',  ( 0.000000000000000000, 0.000000000000000000, -1.000000000000000000 ) ) ;
#17540 = LINE ( 'NONE', #28375, #30696 ) ;
#17541 = ORIENTED_EDGE ( 'NONE', *, *, #28995, .F. ) ;
#17542 = DIRECTION ( 'NONE',  ( 1.300283923313630633E-47, 0.000000000000000000, 1.000000000000000000 ) ) ;
#17543 = DIRECTION ( 'NONE',  ( -1.000000000000000000, 0.000000000000000000, 0.000000000000000000 ) ) ;
#17544 = EDGE_CURVE ( 'NONE', #10934, #16746, #19172, .T. ) ;
#17545 = DIRECTION ( 'NONE',  ( 0.000000000000000000, -1.000000000000000000, 6.123233995736766036E-17 ) ) ;
#17546 = CARTESIAN_POINT ( 'NONE',  ( -442.0000000000000000, -125.0000000000000000, 159.0000000000000000 ) ) ;
#17548 = DIRECTION ( 'NONE',  ( 1.000000000000000000, 0.000000000000000000, 0.000000000000000000 ) ) ;
#17547 = CARTESIAN_POINT ( 'NONE',  ( 30.98406361983695234, 9.959526819984926505, 68.31122994652405112 ) ) ;
#17549 = EDGE_CURVE ( 'NONE', #7713, #23102, #1940, .T. ) ;
#17550 = AXIS2_PLACEMENT_3D ( 'NONE', #7144, #24045, #7497 ) ;
#17551 = CARTESIAN_POINT ( 'NONE',  ( -15.99999999999998579, -145.0000000000000000, -162.9999999999999432 ) ) ;
#17552 = VERTEX_POINT ( 'NONE', #33201 ) ;
#17553 = EDGE_CURVE ( 'NONE', #31542, #16320, #16503, .T. ) ;
#17554 = CARTESIAN_POINT ( 'NONE',  ( 0.000000000000000000, 0.000000000000000000, 0.000000000000000000 ) ) ;
#17556 = LINE ( 'NONE', #6296, #24822 ) ;
#17555 = CARTESIAN_POINT ( 'NONE',  ( -449.9999999999999432, -125.0000000000000000, 162.9999999999999716 ) ) ;
#17557 = ORIENTED_EDGE ( 'NONE', *, *, #1104, .T. ) ;
#17558 = AXIS2_PLACEMENT_3D ( 'NONE', #18697, #29539, #5132 ) ;
#17559 = DIRECTION ( 'NONE',  ( 1.000000000000000000, 0.000000000000000000, 0.000000000000000000 ) ) ;
#17560 = ORIENTED_EDGE ( 'NONE', *, *, #19213, .T. ) ;
#17561 = VECTOR ( 'NONE', #19924, 1000.000000000000227 ) ;
#17562 = ORIENTED_EDGE ( 'NONE', *, *, #17468, .F. ) ;
#17563 = PLANE ( 'NONE',  #2011 ) ;
#17564 = ORIENTED_EDGE ( 'NONE', *, *, #18230, .F. ) ;
#17565 = EDGE_LOOP ( 'NONE', ( #20929, #24541, #17334, #3653 ) ) ;
#17566 = DIRECTION ( 'NONE',  ( 0.000000000000000000, 0.000000000000000000, 1.000000000000000000 ) ) ;
#17567 = AXIS2_PLACEMENT_3D ( 'NONE', #24365, #19231, #30074 ) ;
#17568 = DIRECTION ( 'NONE',  ( 0.000000000000000000, 0.000000000000000000, 1.000000000000000000 ) ) ;
#17569 = CIRCLE ( 'NONE', #14174, 2.085824230283342740 ) ;
#17570 = DIRECTION ( 'NONE',  ( -0.000000000000000000, 1.000000000000000000, -0.000000000000000000 ) ) ;
#17571 = DIRECTION ( 'NONE',  ( 0.000000000000000000, 0.000000000000000000, -1.000000000000000000 ) ) ;
#17572 = ORIENTED_EDGE ( 'NONE', *, *, #14026, .T. ) ;
#17573 = ORIENTED_EDGE ( 'NONE', *, *, #15750, .T. ) ;
#17574 = DIRECTION ( 'NONE',  ( 1.000000000000000000, 0.000000000000000000, 0.000000000000000000 ) ) ;
#17575 = DIRECTION ( 'NONE',  ( 0.000000000000000000, 0.000000000000000000, -1.000000000000000000 ) ) ;
#17576 = DIRECTION ( 'NONE',  ( 0.000000000000000000, 0.000000000000000000, 1.000000000000000000 ) ) ;
#17577 = CARTESIAN_POINT ( 'NONE',  ( -19.99999999999998934, 124.9999999999999716, 187.0000000000000000 ) ) ;
#17578 = DIRECTION ( 'NONE',  ( 0.000000000000000000, -1.000000000000000000, -1.541976423090495633E-16 ) ) ;
#17579 = DIRECTION ( 'NONE',  ( 0.000000000000000000, 1.131431318426415506E-52, 1.000000000000000000 ) ) ;
#17580 = LINE ( 'NONE', #28416, #22704 ) ;
#17581 = ORIENTED_EDGE ( 'NONE', *, *, #3208, .F. ) ;
#17582 = CARTESIAN_POINT ( 'NONE',  ( -12.00000000000001066, -112.9999999999999858, 174.9999999999999432 ) ) ;
#17583 = DIRECTION ( 'NONE',  ( 0.000000000000000000, 0.000000000000000000, -1.000000000000000000 ) ) ;
#17584 = EDGE_CURVE ( 'NONE', #11839, #34323, #26944, .T. ) ;
#17585 = CIRCLE ( 'NONE', #6750, 1.155000000000000027 ) ;
#17586 = FACE_OUTER_BOUND ( 'NONE', #18729, .T. ) ;
#17587 = VERTEX_POINT ( 'NONE', #470 ) ;
#17588 = LINE ( 'NONE', #11889, #34279 ) ;
#17589 = ORIENTED_EDGE ( 'NONE', *, *, #16790, .T. ) ;
#17590 = EDGE_CURVE ( 'NONE', #33889, #26771, #13896, .T. ) ;
#17591 = LINE ( 'NONE', #24862, #20195 ) ;
#17592 = CARTESIAN_POINT ( 'NONE',  ( -109.5852389964325369, 2.273103392716669724, 12.29250028061669120 ) ) ;
#17593 = EDGE_CURVE ( 'NONE', #24798, #17629, #8642, .T. ) ;
#17594 = VECTOR ( 'NONE', #12743, 1000.000000000000000 ) ;
#17595 = VERTEX_POINT ( 'NONE', #3126 ) ;
#17596 = EDGE_CURVE ( 'NONE', #2751, #29867, #27859, .T. ) ;
#17597 = EDGE_CURVE ( 'NONE', #10465, #10319, #21817, .T. ) ;
#17598 = DIRECTION ( 'NONE',  ( 0.000000000000000000, 1.000000000000000000, 5.053935297177146739E-49 ) ) ;
#17599 = DIRECTION ( 'NONE',  ( -0.000000000000000000, -0.000000000000000000, 1.000000000000000000 ) ) ;
#17600 = DIRECTION ( 'NONE',  ( -1.000000000000000000, 0.000000000000000000, 0.000000000000000000 ) ) ;
#17601 = EDGE_CURVE ( 'NONE', #12010, #22497, #14180, .T. ) ;
#17602 = ORIENTED_EDGE ( 'NONE', *, *, #15479, .F. ) ;
#17603 = VECTOR ( 'NONE', #13819, 1000.000000000000000 ) ;
#17604 = DIRECTION ( 'NONE',  ( -0.1063910735369225230, 0.9943243633099118073, -1.000770725407345128E-14 ) ) ;
#17605 = CARTESIAN_POINT ( 'NONE',  ( -37.58721499952019940, -4.609089608337744615, 15.81122994652406355 ) ) ;
#17606 = VERTEX_POINT ( 'NONE', #8819 ) ;
#17607 = DIRECTION ( 'NONE',  ( 1.097052971696008773E-16, -0.8958117331950891105, -0.4444337280967887160 ) ) ;
#17608 = CIRCLE ( 'NONE', #18742, 4.000000000000003553 ) ;
#17609 = FACE_OUTER_BOUND ( 'NONE', #24389, .T. ) ;
#17610 = DIRECTION ( 'NONE',  ( -1.000000000000000000, 0.000000000000000000, 0.000000000000000000 ) ) ;
#17611 = LINE ( 'NONE', #22399, #4569 ) ;
#17612 = ITEM_DEFINED_TRANSFORMATION ( 'NONE', 'NONE', #2455,  #28566 ) ;
#17613 = ORIENTED_EDGE ( 'NONE', *, *, #27808, .F. ) ;
#17614 = ORIENTED_EDGE ( 'NONE', *, *, #11059, .F. ) ;
#17615 = VERTEX_POINT ( 'NONE', #22536 ) ;
#17616 = CARTESIAN_POINT ( 'NONE',  ( 5.021133111224265200, -11.61907005722761177, -87.50000000000000000 ) ) ;
#17617 = CARTESIAN_POINT ( 'NONE',  ( 11.99999999999999645, -124.9999999999999432, -154.9999999999999716 ) ) ;
#17618 = CARTESIAN_POINT ( 'NONE',  ( -37.85301660235036536, 0.7430237821112573027, 68.31122994652405112 ) ) ;
#17619 = CIRCLE ( 'NONE', #2240, 9.999999999999994671 ) ;
#17620 = FACE_OUTER_BOUND ( 'NONE', #23146, .T. ) ;
#17622 = LINE ( 'NONE', #1576, #25392 ) ;
#17621 =( REPRESENTATION_RELATIONSHIP ('NONE','NONE', #23037, #47 ) REPRESENTATION_RELATIONSHIP_WITH_TRANSFORMATION ( #5690 )SHAPE_REPRESENTATION_RELATIONSHIP( ) );
#17623 = CARTESIAN_POINT ( 'NONE',  ( -8.000000000000001776, 1.261386203121773722E-15, 10.30000000000000071 ) ) ;
#17624 = VERTEX_POINT ( 'NONE', #8294 ) ;
#17625 = CARTESIAN_POINT ( 'NONE',  ( 102.4375534982951592, 5.148005685260262254, 11.39183432441182653 ) ) ;
#17626 = ORIENTED_EDGE ( 'NONE', *, *, #14778, .T. ) ;
#17627 = CARTESIAN_POINT ( 'NONE',  ( 5.021133111224576062, 18.16264470403145026, -67.50000000000000000 ) ) ;
#17628 = CARTESIAN_POINT ( 'NONE',  ( 14.14940496480368815, 33.69708579775584667, 49.43553178847298568 ) ) ;
#17629 = VERTEX_POINT ( 'NONE', #11328 ) ;
#17630 = CARTESIAN_POINT ( 'NONE',  ( 2.790000000000081304, -11.08290750742965436, -28.58973358960031774 ) ) ;
#17631 = CARTESIAN_POINT ( 'NONE',  ( -5.491809612354312087, 32.07872192057773475, 68.31122994652405112 ) ) ;
#17632 = EDGE_CURVE ( 'NONE', #12833, #29646, #22967, .T. ) ;
#17633 = CARTESIAN_POINT ( 'NONE',  ( 12.46788440507149787, 30.06253867087536946, 49.43553178847298568 ) ) ;
#17634 = CIRCLE ( 'NONE', #31251, 34.41491905851385269 ) ;
#17635 = EDGE_CURVE ( 'NONE', #30234, #23829, #30012, .T. ) ;
#17636 = ADVANCED_FACE ( 'NONE', ( #3469 ), #16677, .T. ) ;
#17637 = CARTESIAN_POINT ( 'NONE',  ( -20.02113311122498729, -1.691831803474591833, -67.50000000000000000 ) ) ;
#17638 = CARTESIAN_POINT ( 'NONE',  ( 7.700000000000000178, 0.000000000000000000, 0.000000000000000000 ) ) ;
#17639 = DIRECTION ( 'NONE',  ( 0.000000000000000000, 1.836970198721029441E-16, -1.000000000000000000 ) ) ;
#17640 = ORIENTED_EDGE ( 'NONE', *, *, #19656, .T. ) ;
#17641 = ORIENTED_EDGE ( 'NONE', *, *, #27386, .T. ) ;
#17642 = DIRECTION ( 'NONE',  ( -7.051230422235582818E-14, -2.803991727424994432E-14, 0.9999999999999998890 ) ) ;
#17643 = VERTEX_POINT ( 'NONE', #11157 ) ;
#17644 = ADVANCED_FACE ( 'NONE', ( #13998 ), #24837, .T. ) ;
#17645 = CARTESIAN_POINT ( 'NONE',  ( -499.9999999999999432, 112.9999999999999574, -162.9999999999999716 ) ) ;
#17646 = CARTESIAN_POINT ( 'NONE',  ( -442.0000000000000000, -124.9999999999999858, -73.99999999999998579 ) ) ;
#17647 = CONTEXT_DEPENDENT_SHAPE_REPRESENTATION ( #34644, #28842 ) ;
#17648 = ORIENTED_EDGE ( 'NONE', *, *, #31303, .T. ) ;
#17649 = CARTESIAN_POINT ( 'NONE',  ( -5.614556921127968003, -37.45022281665699637, 68.31122994652405112 ) ) ;
#17650 = CARTESIAN_POINT ( 'NONE',  ( -449.9999999999999432, 137.0000000000000000, -155.0000000000000000 ) ) ;
#17651 = EDGE_CURVE ( 'NONE', #9440, #1712, #33520, .T. ) ;
#17652 = AXIS2_PLACEMENT_3D ( 'NONE', #9819, #33008, #5956 ) ;
#17653 = ADVANCED_FACE ( 'NONE', ( #26070 ), #25722, .T. ) ;
#17654 = EDGE_CURVE ( 'NONE', #20922, #18325, #12218, .T. ) ;
#17656 = CARTESIAN_POINT ( 'NONE',  ( -499.9999999999999432, 136.9999999999999432, 190.9999999999999716 ) ) ;
#17655 = DIRECTION ( 'NONE',  ( 1.000000000000000000, 0.000000000000000000, 5.546364386991661285E-52 ) ) ;
#17657 = VERTEX_POINT ( 'NONE', #28399 ) ;
#17658 = ORIENTED_EDGE ( 'NONE', *, *, #4200, .T. ) ;
#17659 = CARTESIAN_POINT ( 'NONE',  ( -18.07349068442144358, -27.06572199953721736, 68.31122994652405112 ) ) ;
#17660 = EDGE_CURVE ( 'NONE', #25758, #14377, #19570, .T. ) ;
#17661 = FACE_OUTER_BOUND ( 'NONE', #633, .T. ) ;
#17662 = DIRECTION ( 'NONE',  ( 0.000000000000000000, -1.224646799147353454E-16, 1.000000000000000000 ) ) ;
#17663 = ORIENTED_EDGE ( 'NONE', *, *, #15735, .F. ) ;
#17664 = LINE ( 'NONE', #15333, #406 ) ;
#17665 =( REPRESENTATION_RELATIONSHIP ('NONE','NONE', #23037, #28231 ) REPRESENTATION_RELATIONSHIP_WITH_TRANSFORMATION ( #9311 )SHAPE_REPRESENTATION_RELATIONSHIP( ) );
#17666 = ORIENTED_EDGE ( 'NONE', *, *, #593, .T. ) ;
#17667 = DIRECTION ( 'NONE',  ( 0.000000000000000000, 0.000000000000000000, 1.000000000000000000 ) ) ;
#17668 = DIRECTION ( 'NONE',  ( -1.232595164407831220E-32, 3.421138828918010427E-49, -1.000000000000000000 ) ) ;
#17669 = DIRECTION ( 'NONE',  ( -0.000000000000000000, 1.836970198721029688E-16, -1.000000000000000000 ) ) ;
#17671 = CARTESIAN_POINT ( 'NONE',  ( -418.0000000000000000, -125.0000000000000000, 190.9999999999999716 ) ) ;
#17670 = CARTESIAN_POINT ( 'NONE',  ( -5.527271473480783293, -1.747512292859696226, 3.930000000000000160 ) ) ;
#17672 = ADVANCED_FACE ( 'NONE', ( #33552 ), #1167, .F. ) ;
#17673 = CARTESIAN_POINT ( 'NONE',  ( 1.040000000000001368, 14.40815186467820652, -31.25366880301302785 ) ) ;
#17674 = DIRECTION ( 'NONE',  ( 1.000000000000000000, 0.000000000000000000, 0.000000000000000000 ) ) ;
#17675 = VERTEX_POINT ( 'NONE', #6838 ) ;
#17676 = DIRECTION ( 'NONE',  ( 0.6051742151937647973, -0.7960930657056438653, -0.000000000000000000 ) ) ;
#17677 = AXIS2_PLACEMENT_3D ( 'NONE', #26121, #1737, #28968 ) ;
#17678 = DIRECTION ( 'NONE',  ( 1.000000000000000000, 0.000000000000000000, 0.000000000000000000 ) ) ;
#17679 = AXIS2_PLACEMENT_3D ( 'NONE', #32495, #16680, #10630 ) ;
#17680 = VERTEX_POINT ( 'NONE', #1516 ) ;
#17681 = ORIENTED_EDGE ( 'NONE', *, *, #13222, .F. ) ;
#17682 = VECTOR ( 'NONE', #11466, 1000.000000000000000 ) ;
#17683 = CARTESIAN_POINT ( 'NONE',  ( 2.789999999999999147, 30.61125888652961891, 5.439165181699118889 ) ) ;
#17684 = AXIS2_PLACEMENT_3D ( 'NONE', #7390, #28426, #31266 ) ;
#17685 = ORIENTED_EDGE ( 'NONE', *, *, #2321, .F. ) ;
#17686 = ORIENTED_EDGE ( 'NONE', *, *, #9526, .T. ) ;
#17687 = EDGE_LOOP ( 'NONE', ( #26020, #22668, #20866, #24926 ) ) ;
#17688 = DIRECTION ( 'NONE',  ( 1.000000000000000000, 3.040835319149746090E-31, 1.232595164407830946E-32 ) ) ;
#17689 = EDGE_CURVE ( 'NONE', #9096, #30302, #30888, .T. ) ;
#17690 = ADVANCED_FACE ( 'NONE', ( #7015 ), #12039, .F. ) ;
#17691 = VERTEX_POINT ( 'NONE', #9355 ) ;
#17692 = DIRECTION ( 'NONE',  ( -0.000000000000000000, 1.000000000000000000, -0.000000000000000000 ) ) ;
#17693 = CARTESIAN_POINT ( 'NONE',  ( 11.99999999999999645, 136.9999999999999716, 155.0000000000000000 ) ) ;
#17694 = ORIENTED_EDGE ( 'NONE', *, *, #1691, .F. ) ;
#17695 = ORIENTED_EDGE ( 'NONE', *, *, #12271, .F. ) ;
#17696 = DIRECTION ( 'NONE',  ( 1.000000000000000000, 0.000000000000000000, 0.000000000000000000 ) ) ;
#17698 = CARTESIAN_POINT ( 'NONE',  ( -20.72055270933793736, 25.09707290294328885, 68.31122994652405112 ) ) ;
#17697 = CIRCLE ( 'NONE', #14849, 3.999999999999976019 ) ;
#17699 = CARTESIAN_POINT ( 'NONE',  ( -12.00000000000001066, -24.99999999999999289, 154.9999999999999716 ) ) ;
#17700 = DIRECTION ( 'NONE',  ( -0.000000000000000000, -1.000000000000000000, -0.000000000000000000 ) ) ;
#17701 = CARTESIAN_POINT ( 'NONE',  ( 1.749999999999999778, -34.41385771548412720, -0.2702793785573802121 ) ) ;
#17702 = VERTEX_POINT ( 'NONE', #20223 ) ;
#17703 = AXIS2_PLACEMENT_3D ( 'NONE', #31586, #28919, #4510 ) ;
#17704 = DIRECTION ( 'NONE',  ( 1.000000000000000000, 0.000000000000000000, 0.000000000000000000 ) ) ;
#17705 = CARTESIAN_POINT ( 'NONE',  ( -37.85301660235036536, 0.7430237821112727348, -15.81122994652406355 ) ) ;
#17706 = DIRECTION ( 'NONE',  ( -5.546364386991661285E-52, 0.000000000000000000, -1.000000000000000000 ) ) ;
#17707 = ORIENTED_EDGE ( 'NONE', *, *, #13190, .F. ) ;
#17708 = CARTESIAN_POINT ( 'NONE',  ( 0.07098933019551863233, -30.32061017160053495, 9.230676164041856424 ) ) ;
#17709 = DIRECTION ( 'NONE',  ( -1.000000000000000000, 0.000000000000000000, 0.000000000000000000 ) ) ;
#17710 = DIRECTION ( 'NONE',  ( 0.000000000000000000, 1.000000000000000000, 1.224646799147353207E-16 ) ) ;
#17711 = CARTESIAN_POINT ( 'NONE',  ( -442.0000000000000000, 104.9999999999999858, -187.0000000000000000 ) ) ;
#17713 = DIRECTION ( 'NONE',  ( 0.000000000000000000, 1.000000000000000000, 0.000000000000000000 ) ) ;
#17712 = LINE ( 'NONE', #9677, #25221 ) ;
#17714 = TOROIDAL_SURFACE ( 'NONE', #15437, 10.30000000000000071, 0.3000000000000025424 ) ;
#17715 = LINE ( 'NONE', #17022, #11006 ) ;
#17716 = ORIENTED_EDGE ( 'NONE', *, *, #2145, .T. ) ;
#17717 = CARTESIAN_POINT ( 'NONE',  ( -442.0000000000000000, 137.0000000000000000, 154.9999999999999716 ) ) ;
#17719 = CARTESIAN_POINT ( 'NONE',  ( -70.00000000000000000, 75.55999999999990280, -177.7400000000000091 ) ) ;
#17718 = DIRECTION ( 'NONE',  ( -1.000000000000000000, 0.000000000000000000, 0.000000000000000000 ) ) ;
#17720 = ORIENTED_EDGE ( 'NONE', *, *, #34504, .T. ) ;
#17721 = CARTESIAN_POINT ( 'NONE',  ( 19.99999999999998224, -115.0000000000000000, -158.9999999999999716 ) ) ;
#17723 = EDGE_CURVE ( 'NONE', #797, #17061, #19041, .T. ) ;
#17722 = AXIS2_PLACEMENT_3D ( 'NONE', #19101, #16256, #21225 ) ;
#17724 = VERTEX_POINT ( 'NONE', #20736 ) ;
#17725 = VECTOR ( 'NONE', #34745, 1000.000000000000000 ) ;
#17726 = ORIENTED_EDGE ( 'NONE', *, *, #7207, .F. ) ;
#17727 = CARTESIAN_POINT ( 'NONE',  ( 100.0742843969711231, -2.949151772667967020, -6.898053038626237310 ) ) ;
#17728 = ORIENTED_EDGE ( 'NONE', *, *, #14727, .T. ) ;
#17729 = ORIENTED_EDGE ( 'NONE', *, *, #8772, .T. ) ;
#17730 = CARTESIAN_POINT ( 'NONE',  ( -414.0000000000000568, -124.9999999999999716, 132.0000000000000000 ) ) ;
#17731 = PRODUCT_DEFINITION_SHAPE ( 'NONE', 'NONE',  #35146 ) ;
#17732 = EDGE_CURVE ( 'NONE', #10757, #23038, #1970, .T. ) ;
#17733 = DIRECTION ( 'NONE',  ( -1.000000000000000000, -0.000000000000000000, -0.000000000000000000 ) ) ;
#17734 = EDGE_CURVE ( 'NONE', #31513, #31845, #6671, .T. ) ;
#17735 = EDGE_CURVE ( 'NONE', #9803, #24429, #4508, .T. ) ;
#17736 = CARTESIAN_POINT ( 'NONE',  ( -418.0000000000000000, 105.0000000000000142, 187.0000000000000000 ) ) ;
#17737 = CARTESIAN_POINT ( 'NONE',  ( 2.765921099433441555, 4.286445725888036407, 30.79383171238946204 ) ) ;
#17738 = ORIENTED_EDGE ( 'NONE', *, *, #3369, .F. ) ;
#17739 = ORIENTED_EDGE ( 'NONE', *, *, #6523, .T. ) ;
#17740 = AXIS2_PLACEMENT_3D ( 'NONE', #140, #10998, #32706 ) ;
#17741 = CARTESIAN_POINT ( 'NONE',  ( 0.02407890056655781832, 7.350529080603967813, -30.20932655202929595 ) ) ;
#17742 = CARTESIAN_POINT ( 'NONE',  ( 11.99999999999999645, -115.0000000000000000, 162.9999999999999716 ) ) ;
#17743 = CIRCLE ( 'NONE', #9736, 5.738084889453667792 ) ;
#17744 = CIRCLE ( 'NONE', #22269, 3.999999999999976019 ) ;
#17745 = CARTESIAN_POINT ( 'NONE',  ( -29.68486519896224962, 23.49918569563713078, -36.68877005347593467 ) ) ;
#17746 = LINE ( 'NONE', #23249, #10168 ) ;
#17747 = DIRECTION ( 'NONE',  ( -0.000000000000000000, 1.000000000000000000, -0.000000000000000000 ) ) ;
#17748 = CARTESIAN_POINT ( 'NONE',  ( -20.00000000000004619, 136.9999999999999432, -194.9999999999999432 ) ) ;
#17749 = PLANE ( 'NONE',  #20435 ) ;
#17750 = EDGE_LOOP ( 'NONE', ( #2984, #6653, #14456, #23705 ) ) ;
#17751 = CARTESIAN_POINT ( 'NONE',  ( -442.0000000000000000, -104.9999999999999858, -159.0000000000000000 ) ) ;
#17752 = CARTESIAN_POINT ( 'NONE',  ( 2.765921099433443775, -11.07880054387241664, 29.04985141099759360 ) ) ;
#17753 = AXIS2_PLACEMENT_3D ( 'NONE', #31463, #23965, #24141 ) ;
#17754 = DIRECTION ( 'NONE',  ( -1.000000000000000000, -0.000000000000000000, 0.000000000000000000 ) ) ;
#17755 = ORIENTED_EDGE ( 'NONE', *, *, #15255, .T. ) ;
#17756 = LINE ( 'NONE', #34101, #17257 ) ;
#17757 = VERTEX_POINT ( 'NONE', #15231 ) ;
#17758 = CARTESIAN_POINT ( 'NONE',  ( 2.789999999999999147, 3.909681563761668421, 30.21863799912384962 ) ) ;
#17759 = CARTESIAN_POINT ( 'NONE',  ( 0.000000000000000000, 23.53611639059712601, 19.35207786518996897 ) ) ;
#17760 = CIRCLE ( 'NONE', #10339, 7.999999999999952038 ) ;
#17761 = EDGE_LOOP ( 'NONE', ( #25233, #899, #14770, #20926 ) ) ;
#17762 = AXIS2_PLACEMENT_3D ( 'NONE', #7424, #18320, #9465 ) ;
#17763 = CYLINDRICAL_SURFACE ( 'NONE', #16591, 7.999999999999979572 ) ;
#17764 = CARTESIAN_POINT ( 'NONE',  ( 0.006892446353074978965, -30.82736387488653307, 1.618073722873083486 ) ) ;
#17765 = AXIS2_PLACEMENT_3D ( 'NONE', #8849, #25211, #33407 ) ;
#17766 = ORIENTED_EDGE ( 'NONE', *, *, #2134, .T. ) ;
#17767 = CARTESIAN_POINT ( 'NONE',  ( 849.5613458659236130, 971.5493010698733087, 1753.598338701303874 ) ) ;
#17768 = EDGE_CURVE ( 'NONE', #25058, #26696, #279, .T. ) ;
#17769 = CARTESIAN_POINT ( 'NONE',  ( 100.1355683589712271, -3.049149995829645743, 12.12344935835687387 ) ) ;
#17770 = ORIENTED_EDGE ( 'NONE', *, *, #11960, .F. ) ;
#17771 = DIRECTION ( 'NONE',  ( -1.000000000000000000, -3.040835319149746528E-31, -1.232595164407830946E-32 ) ) ;
#17772 = EDGE_CURVE ( 'NONE', #11839, #32731, #3988, .T. ) ;
#17773 = CYLINDRICAL_SURFACE ( 'NONE', #19825, 3.999999999999976019 ) ;
#17774 = CARTESIAN_POINT ( 'NONE',  ( 20.62763069236413926, -31.74750072459299588, 68.31122994652405112 ) ) ;
#17775 = FACE_OUTER_BOUND ( 'NONE', #19292, .T. ) ;
#17776 = CONTEXT_DEPENDENT_SHAPE_REPRESENTATION ( #6452, #15172 ) ;
#17777 = ORIENTED_EDGE ( 'NONE', *, *, #34221, .T. ) ;
#17778 = ORIENTED_EDGE ( 'NONE', *, *, #9911, .F. ) ;
#17779 = ORIENTED_EDGE ( 'NONE', *, *, #34524, .F. ) ;
#17780 = PRODUCT_DEFINITION_SHAPE ( 'NONE', 'NONE',  #18183 ) ;
#17781 = CLOSED_SHELL ( 'NONE', ( #24297, #22782, #16560, #24480, #18931, #10238, #16205, #13314, #12026, #13384, #30055, #24549, #15551, #32530, #31766, #14964, #1733, #25128 ) ) ;
#17782 = EDGE_CURVE ( 'NONE', #31630, #14082, #23567, .T. ) ;
#17783 = CARTESIAN_POINT ( 'NONE',  ( 0.5248941002295058889, 27.45362965837519909, 18.98707279867261377 ) ) ;
#17784 = FACE_OUTER_BOUND ( 'NONE', #25775, .T. ) ;
#17785 = AXIS2_PLACEMENT_3D ( 'NONE', #20081, #14748, #15391 ) ;
#17786 = CARTESIAN_POINT ( 'NONE',  ( -418.0000000000000000, 105.0000000000000000, 139.9999999999999716 ) ) ;
#17787 = DIRECTION ( 'NONE',  ( 0.000000000000000000, 0.000000000000000000, -1.000000000000000000 ) ) ;
#17788 = VECTOR ( 'NONE', #34322, 1000.000000000000000 ) ;
#17789 = ADVANCED_FACE ( 'NONE', ( #26235 ), #2527, .T. ) ;
#17790 = AXIS2_PLACEMENT_3D ( 'NONE', #26751, #16091, #18766 ) ;
#17791 = CARTESIAN_POINT ( 'NONE',  ( -1.307386931792819285, 37.83772838912472025, -36.68877005347593467 ) ) ;
#17792 = AXIS2_PLACEMENT_3D ( 'NONE', #12933, #2231, #2061 ) ;
#17793 = LINE ( 'NONE', #28626, #23807 ) ;
#17794 = VERTEX_POINT ( 'NONE', #9173 ) ;
#17795 = EDGE_CURVE ( 'NONE', #20178, #23878, #10585, .T. ) ;
#17796 = CARTESIAN_POINT ( 'NONE',  ( 100.4456562794407404, 3.510468032099187230, 12.00123740321143728 ) ) ;
#17797 = EDGE_CURVE ( 'NONE', #14255, #10121, #21862, .T. ) ;
#17798 = ORIENTED_EDGE ( 'NONE', *, *, #5037, .F. ) ;
#17799 = DIRECTION ( 'NONE',  ( -1.000000000000000000, -0.000000000000000000, -0.000000000000000000 ) ) ;
#17800 = EDGE_LOOP ( 'NONE', ( #10212, #22876, #12959, #21682, #2131, #18702, #16719, #30620 ) ) ;
#17801 = CARTESIAN_POINT ( 'NONE',  ( -500.0000000000000000, -137.0000000000000000, 194.9999999999999716 ) ) ;
#17802 = CARTESIAN_POINT ( 'NONE',  ( 12.00000000000001066, -24.99999999999999289, -154.9999999999999716 ) ) ;
#17803 = ADVANCED_BREP_SHAPE_REPRESENTATION ( '', ( #33586, #28566 ), #10954 ) ;
#17804 = CARTESIAN_POINT ( 'NONE',  ( 0.006892411738745651655, 7.365885187734036776, 29.97812926094526631 ) ) ;
#17805 = UNCERTAINTY_MEASURE_WITH_UNIT (LENGTH_MEASURE( 1.000000000000000082E-05 ), #19822, 'distance_accuracy_value', 'NONE');
#17806 = DIRECTION ( 'NONE',  ( -3.040835319149746090E-31, -1.000000000000000000, 0.000000000000000000 ) ) ;
#17807 = CARTESIAN_POINT ( 'NONE',  ( -410.0000000000000568, 113.0000000000000000, -175.0000000000000000 ) ) ;
#17808 = ORIENTED_EDGE ( 'NONE', *, *, #32870, .T. ) ;
#17809 = AXIS2_PLACEMENT_3D ( 'NONE', #19600, #30623, #24740 ) ;
#17810 = ORIENTED_EDGE ( 'NONE', *, *, #8899, .T. ) ;
#17811 = AXIS2_PLACEMENT_3D ( 'NONE', #27534, #8846, #5464 ) ;
#17812 =( GEOMETRIC_REPRESENTATION_CONTEXT ( 3 ) GLOBAL_UNCERTAINTY_ASSIGNED_CONTEXT ( ( #20292 ) ) GLOBAL_UNIT_ASSIGNED_CONTEXT ( ( #22824, #12678, #6957 ) ) REPRESENTATION_CONTEXT ( 'NONE', 'WORKASPACE' ) );
#17813 = CARTESIAN_POINT ( 'NONE',  ( 794.7823015743225596, 984.2911726958192276, 1753.598338701303646 ) ) ;
#17814 = VECTOR ( 'NONE', #21754, 1000.000000000000000 ) ;
#17815 = ORIENTED_EDGE ( 'NONE', *, *, #18334, .T. ) ;
#17816 = DIRECTION ( 'NONE',  ( -0.8276889981568904542, 0.5611870653623824978, -0.000000000000000000 ) ) ;
#17817 = LINE ( 'NONE', #17301, #10827 ) ;
#17818 = ITEM_DEFINED_TRANSFORMATION ( 'NONE', 'NONE', #13249,  #28566 ) ;
#17819 = ORIENTED_EDGE ( 'NONE', *, *, #10691, .F. ) ;
#17820 = FACE_OUTER_BOUND ( 'NONE', #22930, .T. ) ;
#17821 = FACE_OUTER_BOUND ( 'NONE', #18546, .T. ) ;
#17822 = EDGE_CURVE ( 'NONE', #22648, #7666, #21289, .T. ) ;
#17823 = VECTOR ( 'NONE', #21624, 1000.000000000000000 ) ;
#17825 = DIRECTION ( 'NONE',  ( 0.000000000000000000, 0.000000000000000000, -1.000000000000000000 ) ) ;
#17824 = LINE ( 'NONE', #20997, #3090 ) ;
#17826 = ORIENTED_EDGE ( 'NONE', *, *, #33745, .F. ) ;
#17827 = ORIENTED_EDGE ( 'NONE', *, *, #22191, .F. ) ;
#17828 = EDGE_CURVE ( 'NONE', #19084, #31987, #34786, .T. ) ;
#17829 = ADVANCED_FACE ( 'NONE', ( #24084 ), #24711, .F. ) ;
#17830 = CARTESIAN_POINT ( 'NONE',  ( -19.99999999999998934, -32.99999999999997158, -175.0000000000000000 ) ) ;
#17831 = DIRECTION ( 'NONE',  ( -1.000000000000000000, 0.000000000000000000, 0.000000000000000000 ) ) ;
#17832 = CARTESIAN_POINT ( 'NONE',  ( 3.235562306570555532E-30, -5.758675521474011738, -87.50000000000000000 ) ) ;
#17833 = VERTEX_POINT ( 'NONE', #5212 ) ;
#17834 = AXIS2_PLACEMENT_3D ( 'NONE', #34876, #10667, #31826 ) ;
#17835 = PLANE ( 'NONE',  #2653 ) ;
#17836 = CIRCLE ( 'NONE', #1336, 2.525000000000000799 ) ;
#17837 = VECTOR ( 'NONE', #26878, 1000.000000000000000 ) ;
#17838 = ORIENTED_EDGE ( 'NONE', *, *, #27854, .T. ) ;
#17839 = LINE ( 'NONE', #12321, #27117 ) ;
#17840 = DIRECTION ( 'NONE',  ( 1.000000000000000000, 0.000000000000000000, 0.000000000000000000 ) ) ;
#17841 = ADVANCED_FACE ( 'NONE', ( #2210, #26766 ), #31917, .T. ) ;
#17842 = CYLINDRICAL_SURFACE ( 'NONE', #14987, 3.999999999999976019 ) ;
#17844 = DIRECTION ( 'NONE',  ( 0.000000000000000000, 3.374343856708137958E-53, -1.000000000000000000 ) ) ;
#17843 = CARTESIAN_POINT ( 'NONE',  ( 2.783107600408745164, -7.987299431473431355, -29.81857704081753369 ) ) ;
#17845 = DIRECTION ( 'NONE',  ( 0.000000000000000000, 0.000000000000000000, -1.000000000000000000 ) ) ;
#17846 = CARTESIAN_POINT ( 'NONE',  ( -22.50000000000000355, 0.000000000000000000, 20.00000000000000000 ) ) ;
#17847 = CARTESIAN_POINT ( 'NONE',  ( 44.94043929807611448, -32.65143121711728469, 20.00000000000000000 ) ) ;
#17848 = FACE_OUTER_BOUND ( 'NONE', #33435, .T. ) ;
#17849 = EDGE_CURVE ( 'NONE', #34805, #16028, #32278, .T. ) ;
#17850 = EDGE_CURVE ( 'NONE', #1771, #21781, #26407, .T. ) ;
#17851 = AXIS2_PLACEMENT_3D ( 'NONE', #25466, #1094, #14101 ) ;
#17852 = ORIENTED_EDGE ( 'NONE', *, *, #17596, .F. ) ;
#17853 = EDGE_CURVE ( 'NONE', #33874, #33898, #26267, .T. ) ;
#17854 =( NAMED_UNIT ( * ) PLANE_ANGLE_UNIT ( ) SI_UNIT ( $, .RADIAN. ) );
#17855 = ORIENTED_EDGE ( 'NONE', *, *, #8968, .T. ) ;
#17856 = ORIENTED_EDGE ( 'NONE', *, *, #23181, .T. ) ;
#17857 = AXIS2_PLACEMENT_3D ( 'NONE', #15970, #34471, #23616 ) ;
#17858 = AXIS2_PLACEMENT_3D ( 'NONE', #4892, #13284, #10609 ) ;
#17859 = CARTESIAN_POINT ( 'NONE',  ( -8.346024214154725512E-14, 18.20059223136345139, 24.67675383855258175 ) ) ;
#17860 = AXIS2_PLACEMENT_3D ( 'NONE', #28811, #20290, #6743 ) ;
#17861 = VERTEX_POINT ( 'NONE', #31749 ) ;
#17862 = ORIENTED_EDGE ( 'NONE', *, *, #11305, .F. ) ;
#17863 = ORIENTED_EDGE ( 'NONE', *, *, #13615, .F. ) ;
#17864 = LINE ( 'NONE', #22672, #28148 ) ;
#17865 = VERTEX_POINT ( 'NONE', #4863 ) ;
#17866 = CARTESIAN_POINT ( 'NONE',  ( 14.14940496480368992, 33.69708579775584667, 68.31122994652405112 ) ) ;
#17867 = DIRECTION ( 'NONE',  ( 1.000000000000000000, 0.000000000000000000, 0.000000000000000000 ) ) ;
#17868 = EDGE_LOOP ( 'NONE', ( #27198, #13185, #10070, #20481 ) ) ;
#17869 = EDGE_LOOP ( 'NONE', ( #26045, #31975, #19829, #6091, #2497, #20814, #8997, #14741 ) ) ;
#17870 = EDGE_CURVE ( 'NONE', #18461, #29867, #18460, .T. ) ;
#17871 = EDGE_CURVE ( 'NONE', #11374, #26985, #26943, .T. ) ;
#17872 =( REPRESENTATION_RELATIONSHIP ('NONE','NONE', #23037, #15767 ) REPRESENTATION_RELATIONSHIP_WITH_TRANSFORMATION ( #31456 )SHAPE_REPRESENTATION_RELATIONSHIP( ) );
#17873 = FACE_OUTER_BOUND ( 'NONE', #15357, .T. ) ;
#17874 = CARTESIAN_POINT ( 'NONE',  ( -20.00000000000007461, 136.9999999999999432, 190.9999999999999716 ) ) ;
#17875 = CARTESIAN_POINT ( 'NONE',  ( 3.235562306570555532E-30, -5.758675521474015291, -67.50000000000000000 ) ) ;
#17876 = EDGE_CURVE ( 'NONE', #9042, #14283, #2553, .T. ) ;
#17877 = CARTESIAN_POINT ( 'NONE',  ( 5.713835024271039842, 32.03991982186467880, -36.68877005347593467 ) ) ;
#17878 = LINE ( 'NONE', #28710, #10300 ) ;
#17879 = ORIENTED_EDGE ( 'NONE', *, *, #18340, .T. ) ;
#17880 = CARTESIAN_POINT ( 'NONE',  ( -5.210000000000000853, 0.000000000000000000, 0.000000000000000000 ) ) ;
#17881 = CARTESIAN_POINT ( 'NONE',  ( 1.155000000000000027, 1.414467053015192904E-16, 3.930000000000000160 ) ) ;
#17882 = AXIS2_PLACEMENT_3D ( 'NONE', #1725, #18133, #31448 ) ;
#17883 = B_SPLINE_CURVE_WITH_KNOTS ( 'NONE', 3,
 ( #34056, #17708, #20201, #9144, #15031, #28717 ),
 .UNSPECIFIED., .F., .F.,
 ( 4, 2, 4 ),
 ( 1.974571759321709208E-07, 0.001873395748763636952, 0.003746594040351341418 ),
 .UNSPECIFIED. ) ;
#17884 = DIRECTION ( 'NONE',  ( -1.000000000000000000, 0.000000000000000000, 0.000000000000000000 ) ) ;
#17885 = ORIENTED_EDGE ( 'NONE', *, *, #20299, .F. ) ;
#17886 = AXIS2_PLACEMENT_3D ( 'NONE', #10846, #21873, #167 ) ;
#17887 = DIRECTION ( 'NONE',  ( -0.000000000000000000, 1.836970198721029934E-16, -1.000000000000000000 ) ) ;
#17888 = DIRECTION ( 'NONE',  ( 0.000000000000000000, 0.000000000000000000, 1.000000000000000000 ) ) ;
#17889 = DIRECTION ( 'NONE',  ( 0.000000000000000000, -1.000000000000000000, 0.000000000000000000 ) ) ;
#17890 = CARTESIAN_POINT ( 'NONE',  ( 1.749999999999999778, -33.39989884085085237, -8.296590337300626672 ) ) ;
#17891 = CARTESIAN_POINT ( 'NONE',  ( -418.0000000000000000, 105.0000000000000142, -175.0000000000000000 ) ) ;
#17893 = CYLINDRICAL_SURFACE ( 'NONE', #27594, 7.999999999999979572 ) ;
#17892 = FACE_OUTER_BOUND ( 'NONE', #21310, .T. ) ;
#17894 = VECTOR ( 'NONE', #9645, 1000.000000000000000 ) ;
#17895 = CARTESIAN_POINT ( 'NONE',  ( -20.00000000000001776, -113.0000000000000000, 159.0000000000000000 ) ) ;
#17896 = ORIENTED_EDGE ( 'NONE', *, *, #30326, .T. ) ;
#17897 = CARTESIAN_POINT ( 'NONE',  ( 99.85295625471279379, 2.564129753321951366, -12.23925059504672497 ) ) ;
#17899 = CARTESIAN_POINT ( 'NONE',  ( 19.99999999999998934, -124.9999999999999432, -162.9999999999999432 ) ) ;
#17898 = FACE_OUTER_BOUND ( 'NONE', #33671, .T. ) ;
#17900 = TOROIDAL_SURFACE ( 'NONE', #19590, 15.69999999999999929, 0.3000000000000007661 ) ;
#17901 = EDGE_CURVE ( 'NONE', #29621, #4287, #24261, .T. ) ;
#17902 = EDGE_CURVE ( 'NONE', #4330, #2635, #32447, .T. ) ;
#17903 = ORIENTED_EDGE ( 'NONE', *, *, #32337, .F. ) ;
#17904 = DIRECTION ( 'NONE',  ( 0.000000000000000000, 1.000000000000000000, -1.224646799147353207E-16 ) ) ;
#17905 = EDGE_CURVE ( 'NONE', #20006, #16672, #26412, .T. ) ;
#17906 = EDGE_LOOP ( 'NONE', ( #19348, #33291, #607, #15803, #5431, #994, #28229, #9191, #21012 ) ) ;
#17907 = VECTOR ( 'NONE', #22887, 1000.000000000000000 ) ;
#17908 = EDGE_CURVE ( 'NONE', #2780, #31630, #23909, .T. ) ;
#17909 = EDGE_CURVE ( 'NONE', #26816, #8431, #34612, .T. ) ;
#17910 = ORIENTED_EDGE ( 'NONE', *, *, #18951, .F. ) ;
#17911 = DIRECTION ( 'NONE',  ( 1.000000000000000000, 0.000000000000000000, 0.000000000000000000 ) ) ;
#17912 = ORIENTED_EDGE ( 'NONE', *, *, #13869, .F. ) ;
#17913 = EDGE_LOOP ( 'NONE', ( #7455, #17294 ) ) ;
#17914 = DIRECTION ( 'NONE',  ( 3.469446951953832974E-18, 1.000000000000000000, 7.888609052210116302E-31 ) ) ;
#17915 = VECTOR ( 'NONE', #31128, 1000.000000000000000 ) ;
#17916 = VERTEX_POINT ( 'NONE', #7890 ) ;
#17917 = AXIS2_PLACEMENT_3D ( 'NONE', #12532, #34238, #9849 ) ;
#17918 = CARTESIAN_POINT ( 'NONE',  ( 0.000000000000000000, 0.000000000000000000, -0.7500000000000000000 ) ) ;
#17919 = CARTESIAN_POINT ( 'NONE',  ( -499.9999999999999432, 112.9999999999999574, -187.0000000000000000 ) ) ;
#17920 = ORIENTED_EDGE ( 'NONE', *, *, #33789, .F. ) ;
#17921 = VERTEX_POINT ( 'NONE', #5043 ) ;
#17922 = CARTESIAN_POINT ( 'NONE',  ( 0.07094834059292320916, 7.308651292220183393, -30.83982692225020017 ) ) ;
#17923 = CARTESIAN_POINT ( 'NONE',  ( -499.9999999999999432, 112.9999999999999574, 155.0000000000000000 ) ) ;
#17924 = DIRECTION ( 'NONE',  ( 1.000000000000000000, 3.469446951953834515E-18, 0.000000000000000000 ) ) ;
#17925 = VECTOR ( 'NONE', #9743, 1000.000000000000000 ) ;
#17926 = CARTESIAN_POINT ( 'NONE',  ( -418.0000000000000000, 105.0000000000000142, -101.9999999999999858 ) ) ;
#17927 = CARTESIAN_POINT ( 'NONE',  ( -418.0000000000000000, -105.0000000000000142, 190.9999999999999716 ) ) ;
#17928 = ORIENTED_EDGE ( 'NONE', *, *, #25667, .F. ) ;
#17929 = FACE_BOUND ( 'NONE', #22601, .T. ) ;
#17930 = CARTESIAN_POINT ( 'NONE',  ( 8.000000000000000000, 0.000000000000000000, 0.000000000000000000 ) ) ;
#17931 = ORIENTED_EDGE ( 'NONE', *, *, #10774, .T. ) ;
#17932 = EDGE_CURVE ( 'NONE', #6669, #9466, #15940, .T. ) ;
#17933 = DIRECTION ( 'NONE',  ( 0.6876994588534234287, 0.7259954919231307313, 1.333632083068605180E-16 ) ) ;
#17934 = DIRECTION ( 'NONE',  ( 1.000000000000000000, 0.000000000000000000, 0.000000000000000000 ) ) ;
#17935 = CARTESIAN_POINT ( 'NONE',  ( 34.14795412574902400, 16.36947364650383818, 68.31122994652405112 ) ) ;
#17936 = ORIENTED_EDGE ( 'NONE', *, *, #10693, .T. ) ;
#17937 = AXIS2_PLACEMENT_3D ( 'NONE', #26372, #1989, #19611 ) ;
#17938 = LINE ( 'NONE', #31097, #4158 ) ;
#17939 = ORIENTED_EDGE ( 'NONE', *, *, #11762, .F. ) ;
#17941 = DIRECTION ( 'NONE',  ( 0.000000000000000000, 0.000000000000000000, 1.000000000000000000 ) ) ;
#17940 = CARTESIAN_POINT ( 'NONE',  ( -5.527271473480783293, -1.747512292859696226, -0.7500000000000000000 ) ) ;
#17942 = VECTOR ( 'NONE', #13094, 1000.000000000000000 ) ;
#17943 = CARTESIAN_POINT ( 'NONE',  ( 11.99999999999999645, -124.9999999999999432, -162.9999999999999432 ) ) ;
#17944 = EDGE_CURVE ( 'NONE', #27831, #20735, #27469, .T. ) ;
#17945 = CIRCLE ( 'NONE', #511, 32.54542015209054284 ) ;
#17946 = EDGE_CURVE ( 'NONE', #192, #12145, #16756, .T. ) ;
#17948 = EDGE_CURVE ( 'NONE', #31845, #32751, #31520, .T. ) ;
#17947 = B_SPLINE_CURVE_WITH_KNOTS ( 'NONE', 3,
 ( #10564, #32603, #24415, #15739 ),
 .UNSPECIFIED., .F., .F.,
 ( 4, 4 ),
 ( 2.335573237707780769E-07, 0.0006879695513619300427 ),
 .UNSPECIFIED. ) ;
#17949 = VERTEX_POINT ( 'NONE', #11640 ) ;
#17950 = AXIS2_PLACEMENT_3D ( 'NONE', #5993, #11896, #27720 ) ;
#17951 = DIRECTION ( 'NONE',  ( 0.000000000000000000, -1.000000000000000000, -3.083952846180992253E-16 ) ) ;
#17952 = CARTESIAN_POINT ( 'NONE',  ( 2.783128873642846113, -15.15173253686525001, 26.89521541643887304 ) ) ;
#17953 = CLOSED_SHELL ( 'NONE', ( #14440, #11716, #8676, #6332, #1324, #21461, #33107, #28896, #26535, #5083, #6298, #14957, #13282, #13113, #30975, #34813, #22552, #33299 ) ) ;
#17954 = ORIENTED_EDGE ( 'NONE', *, *, #19153, .F. ) ;
#17955 = CARTESIAN_POINT ( 'NONE',  ( 839.9572555280482220, 962.8983482718184632, 1753.598338701303192 ) ) ;
#17956 = ORIENTED_EDGE ( 'NONE', *, *, #6366, .F. ) ;
#17957 = CARTESIAN_POINT ( 'NONE',  ( 1.205771365940041306, -7.794228634059936489, 13.50000000000000000 ) ) ;
#17958 = ORIENTED_EDGE ( 'NONE', *, *, #14621, .T. ) ;
#17959 = DIRECTION ( 'NONE',  ( -0.000000000000000000, -1.000000000000000000, -0.000000000000000000 ) ) ;
#17960 = SURFACE_STYLE_FILL_AREA ( #28785 ) ;
#17961 = VECTOR ( 'NONE', #6319, 1000.000000000000000 ) ;
#17962 = LINE ( 'NONE', #9219, #33819 ) ;
#17963 = CARTESIAN_POINT ( 'NONE',  ( 11.99999999999999645, 112.9999999999999574, -155.0000000000000000 ) ) ;
#17964 = ITEM_DEFINED_TRANSFORMATION ( 'NONE', 'NONE', #30304,  #28566 ) ;
#17965 = ORIENTED_EDGE ( 'NONE', *, *, #68, .T. ) ;
#17966 = ORIENTED_EDGE ( 'NONE', *, *, #6002, .F. ) ;
#17967 = EDGE_LOOP ( 'NONE', ( #31309, #12681, #27639, #32244 ) ) ;
#17968 = VECTOR ( 'NONE', #32075, 1000.000000000000000 ) ;
#17969 = DIRECTION ( 'NONE',  ( -0.000000000000000000, -1.836970198721029688E-16, 1.000000000000000000 ) ) ;
#17970 = VECTOR ( 'NONE', #29982, 1000.000000000000000 ) ;
#17971 = DIRECTION ( 'NONE',  ( 0.000000000000000000, 0.000000000000000000, -1.000000000000000000 ) ) ;
#17972 = CARTESIAN_POINT ( 'NONE',  ( -12.00000000000001066, 124.9999999999999716, 187.0000000000000000 ) ) ;
#17973 = DIRECTION ( 'NONE',  ( 0.000000000000000000, -0.000000000000000000, 1.000000000000000000 ) ) ;
#17974 = CARTESIAN_POINT ( 'NONE',  ( 20.89386240318430055, 24.95297350523386015, 49.43553178847298568 ) ) ;
#17975 = LINE ( 'NONE', #4402, #25496 ) ;
#17976 = VERTEX_POINT ( 'NONE', #246 ) ;
#17977 = VECTOR ( 'NONE', #25304, 1000.000000000000000 ) ;
#17978 = CARTESIAN_POINT ( 'NONE',  ( 109.6574619143216580, 3.356865266134899439, 12.04189187465341959 ) ) ;
#17979 = EDGE_LOOP ( 'NONE', ( #2721, #505, #11959 ) ) ;
#17980 = CARTESIAN_POINT ( 'NONE',  ( 2.033800785574606085, -25.08322906883849512, 22.82697412903067757 ) ) ;
#17981 = VERTEX_POINT ( 'NONE', #6093 ) ;
#17982 = CARTESIAN_POINT ( 'NONE',  ( 0.000000000000000000, 10.87635688602997597, 87.50000000000000000 ) ) ;
#17983 = ADVANCED_FACE ( 'NONE', ( #6263 ), #21777, .T. ) ;
#17984 = DIRECTION ( 'NONE',  ( -1.000000000000000000, -3.040835319149746528E-31, -1.232595164407830946E-32 ) ) ;
#17985 = VECTOR ( 'NONE', #2905, 1000.000000000000114 ) ;
#17986 = EDGE_CURVE ( 'NONE', #984, #404, #22491, .T. ) ;
#17987 = CARTESIAN_POINT ( 'NONE',  ( -262.5000000000000000, 0.000000000000000000, 0.000000000000000000 ) ) ;
#17988 = CARTESIAN_POINT ( 'NONE',  ( 0.02407890056655738464, -11.07880054387241664, 29.04985141099759360 ) ) ;
#17990 = EDGE_CURVE ( 'NONE', #5282, #26863, #11287, .T. ) ;
#17989 =( NAMED_UNIT ( * ) PLANE_ANGLE_UNIT ( ) SI_UNIT ( $, .RADIAN. ) );
#17991 = ORIENTED_EDGE ( 'NONE', *, *, #28078, .F. ) ;
#17992 = EDGE_LOOP ( 'NONE', ( #5159, #28757, #34361, #9552 ) ) ;
#17993 = DIRECTION ( 'NONE',  ( -7.893605728314050488E-14, 1.618803117314786135E-15, 0.9999999999999998890 ) ) ;
#17994 = ORIENTED_EDGE ( 'NONE', *, *, #23931, .F. ) ;
#17996 = VECTOR ( 'NONE', #23265, 1000.000000000000000 ) ;
#17995 = B_SPLINE_CURVE_WITH_KNOTS ( 'NONE', 3,
 ( #4238, #12457, #137, #13662, #2447, #31994, #8139, #19199, #30040, #21332, #13329, #2797, #29341, #32702, #24160, #21669, #16357, #7605, #15832, #35040, #10653, #5110, #18676, #18507, #24496, #19024, #21841, #7963, #13845, #21505, #13494, #5631, #16528, #5466, #24680, #26839, #32347, #15998 ),
 .UNSPECIFIED., .F., .F.,
 ( 4, 2, 2, 2, 2, 2, 2, 2, 2, 2, 2, 2, 2, 2, 2, 2, 2, 2, 4 ),
 ( 6.964173773746940579E-19, 0.001010717872208370584, 0.002021435744416740302, 0.003032153616625109585, 0.004042871488833478869, 0.005053589361041847285, 0.006064307233250216568, 0.006569666169354382128, 0.007075025105458547688, 0.008085742977666834572, 0.009096460849875124058, 0.01010717872208341354, 0.01111789659429170130, 0.01212861446649999078, 0.01313933233870828200, 0.01364469127481241460, 0.01415005021091654720, 0.01516076808312482802, 0.01617148595533311056 ),
 .UNSPECIFIED. ) ;
#17997 = EDGE_CURVE ( 'NONE', #8985, #32701, #21959, .T. ) ;
#17998 = CARTESIAN_POINT ( 'NONE',  ( 2.789999999999999147, 20.79173593595263014, 22.27454621808771762 ) ) ;
#17999 = CARTESIAN_POINT ( 'NONE',  ( 0.000000000000000000, 2.281310696040539424E-14, -36.68877005347594178 ) ) ;
#18000 = CARTESIAN_POINT ( 'NONE',  ( 0.02407890056655608360, -27.96208973699893008, -13.59246946040217630 ) ) ;
#18001 = ORIENTED_EDGE ( 'NONE', *, *, #21553, .F. ) ;
#18002 = DIRECTION ( 'NONE',  ( -0.000000000000000000, -1.836970198721029688E-16, 1.000000000000000000 ) ) ;
#18003 = CARTESIAN_POINT ( 'NONE',  ( -355.0000000000000000, 130.9999999999999716, 130.0000000000000000 ) ) ;
#18004 = CONTEXT_DEPENDENT_SHAPE_REPRESENTATION ( #26261, #26935 ) ;
#18005 = VECTOR ( 'NONE', #7111, 1000.000000000000000 ) ;
#18007 = LINE ( 'NONE', #2130, #29516 ) ;
#18006 = DIRECTION ( 'NONE',  ( 1.000000000000000000, -0.000000000000000000, -0.000000000000000000 ) ) ;
#18008 = ORIENTED_EDGE ( 'NONE', *, *, #33673, .T. ) ;
#18009 = ORIENTED_EDGE ( 'NONE', *, *, #5517, .T. ) ;
#18010 = CARTESIAN_POINT ( 'NONE',  ( -347.0000000000000000, -135.0000000000000000, 126.0000000000000000 ) ) ;
#18011 = ORIENTED_EDGE ( 'NONE', *, *, #32890, .F. ) ;
#18012 = VECTOR ( 'NONE', #4885, 1000.000000000000000 ) ;
#18013 = CARTESIAN_POINT ( 'NONE',  ( 2.604019731669432680, 19.63342256285856990, -25.62496134208807064 ) ) ;
#18014 = DIRECTION ( 'NONE',  ( 0.000000000000000000, 1.836970198721029934E-16, -1.000000000000000000 ) ) ;
#18015 = ORIENTED_EDGE ( 'NONE', *, *, #33722, .F. ) ;
#18016 = DIRECTION ( 'NONE',  ( -1.000000000000000000, 0.000000000000000000, 0.000000000000000000 ) ) ;
#18017 = ORIENTED_EDGE ( 'NONE', *, *, #29169, .F. ) ;
#18018 = DIRECTION ( 'NONE',  ( 0.000000000000000000, 0.000000000000000000, 1.000000000000000000 ) ) ;
#18019 = CARTESIAN_POINT ( 'NONE',  ( -6.500000000000000000, 0.000000000000000000, 3.180000000000000160 ) ) ;
#18020 = EDGE_CURVE ( 'NONE', #16015, #1917, #17348, .T. ) ;
#18021 = CARTESIAN_POINT ( 'NONE',  ( -29.72561944762171393, -13.25111019240559251, 68.31122994652405112 ) ) ;
#18023 = CARTESIAN_POINT ( 'NONE',  ( 2.789819856565905809, -25.83993731729781373, -16.24881338200996694 ) ) ;
#18022 = DIRECTION ( 'NONE',  ( 1.000000000000000000, 0.000000000000000000, 0.000000000000000000 ) ) ;
#18024 = CARTESIAN_POINT ( 'NONE',  ( 10.00000000000000000, 0.000000000000000000, 8.000000000000000000 ) ) ;
#18025 = FACE_OUTER_BOUND ( 'NONE', #31954, .T. ) ;
#18026 = FACE_OUTER_BOUND ( 'NONE', #5829, .T. ) ;
#18028 = EDGE_CURVE ( 'NONE', #11449, #7721, #19654, .T. ) ;
#18027 = CARTESIAN_POINT ( 'NONE',  ( 110.7380848894536598, 7.027127293105233764E-16, 60.00000000000000000 ) ) ;
#18029 = PRODUCT_DEFINITION_SHAPE ( 'NONE', 'NONE',  #35156 ) ;
#18030 = CIRCLE ( 'NONE', #5487, 2.524999999999999467 ) ;
#18031 = EDGE_CURVE ( 'NONE', #6803, #28782, #592, .T. ) ;
#18032 = AXIS2_PLACEMENT_3D ( 'NONE', #10320, #15327, #29547 ) ;
#18033 = VERTEX_POINT ( 'NONE', #11110 ) ;
#18034 = EDGE_CURVE ( 'NONE', #27889, #19582, #34943, .T. ) ;
#18035 = EDGE_CURVE ( 'NONE', #9940, #24880, #22134, .T. ) ;
#18036 = ORIENTED_EDGE ( 'NONE', *, *, #33383, .T. ) ;
#18037 = EDGE_LOOP ( 'NONE', ( #8112, #8942, #19917, #28588, #4687, #23830 ) ) ;
#18038 = EDGE_CURVE ( 'NONE', #9316, #9953, #32624, .T. ) ;
#18039 = DIRECTION ( 'NONE',  ( 0.000000000000000000, 0.000000000000000000, 1.000000000000000000 ) ) ;
#18040 = ORIENTED_EDGE ( 'NONE', *, *, #23622, .T. ) ;
#18041 = EDGE_LOOP ( 'NONE', ( #19866, #27748, #12164, #1980, #13980, #4719, #15793, #20112 ) ) ;
#18042 = ORIENTED_EDGE ( 'NONE', *, *, #33985, .T. ) ;
#18043 = LINE ( 'NONE', #24040, #23019 ) ;
#18044 = EDGE_CURVE ( 'NONE', #33196, #22205, #34367, .T. ) ;
#18045 = ITEM_DEFINED_TRANSFORMATION ( 'NONE', 'NONE', #3624,  #28566 ) ;
#18046 = ORIENTED_EDGE ( 'NONE', *, *, #17346, .F. ) ;
#18047 = CARTESIAN_POINT ( 'NONE',  ( 1.040000000000000924, 0.000000000000000000, 0.000000000000000000 ) ) ;
#18048 = DIRECTION ( 'NONE',  ( -1.000000000000000000, -0.000000000000000000, -0.000000000000000000 ) ) ;
#18049 = VERTEX_POINT ( 'NONE', #14131 ) ;
#18050 = ORIENTED_EDGE ( 'NONE', *, *, #9076, .F. ) ;
#18051 = DIRECTION ( 'NONE',  ( 1.000000000000000000, 0.000000000000000000, 0.000000000000000000 ) ) ;
#18052 = FACE_OUTER_BOUND ( 'NONE', #12731, .T. ) ;
#18053 = AXIS2_PLACEMENT_3D ( 'NONE', #4887, #31942, #7556 ) ;
#18054 = DIRECTION ( 'NONE',  ( 1.000000000000000000, 0.000000000000000000, 0.000000000000000000 ) ) ;
#18055 = CARTESIAN_POINT ( 'NONE',  ( 8.485274312747499437, 31.41981051364776789, -36.68877005347593467 ) ) ;
#18056 = LINE ( 'NONE', #4649, #23939 ) ;
#18057 = VERTEX_POINT ( 'NONE', #11453 ) ;
#18059 = DIRECTION ( 'NONE',  ( -0.000000000000000000, 0.000000000000000000, 1.000000000000000000 ) ) ;
#18058 = VECTOR ( 'NONE', #15732, 1000.000000000000000 ) ;
#18061 = LINE ( 'NONE', #23543, #32161 ) ;
#18060 = VECTOR ( 'NONE', #13368, 1000.000000000000000 ) ;
#18062 = DIRECTION ( 'NONE',  ( -1.000000000000000000, 0.000000000000000000, 0.000000000000000000 ) ) ;
#18063 = ORIENTED_EDGE ( 'NONE', *, *, #35049, .T. ) ;
#18064 = DIRECTION ( 'NONE',  ( 0.000000000000000000, 0.000000000000000000, 1.000000000000000000 ) ) ;
#18065 = CARTESIAN_POINT ( 'NONE',  ( -430.0000000000000000, -117.0000000000000000, 126.0000000000000000 ) ) ;
#18066 = CARTESIAN_POINT ( 'NONE',  ( 107.9034705589754140, 4.962255517573300523, -5.629655879752474057 ) ) ;
#18067 = AXIS2_PLACEMENT_3D ( 'NONE', #14007, #28050, #25015 ) ;
#18069 = CARTESIAN_POINT ( 'NONE',  ( 129.3530333899765594, -6.000000000000000000, 62.49999999999999289 ) ) ;
#18068 = CARTESIAN_POINT ( 'NONE',  ( -1.030735741678193484, 1.713938105891546826, -0.7500000000000000000 ) ) ;
#18070 = DIRECTION ( 'NONE',  ( 0.000000000000000000, 0.000000000000000000, -1.000000000000000000 ) ) ;
#18071 = ORIENTED_EDGE ( 'NONE', *, *, #22404, .F. ) ;
#18072 = CARTESIAN_POINT ( 'NONE',  ( 103.4959697225922923, 5.540701522433005621, -11.20510851329257918 ) ) ;
#18074 = CARTESIAN_POINT ( 'NONE',  ( 0.000000000000000000, 29.94779062842788164, 5.619744560739158068 ) ) ;
#18073 = FILL_AREA_STYLE ('',( #28387 ) ) ;
#18075 = VECTOR ( 'NONE', #29278, 1000.000000000000000 ) ;
#18076 = ORIENTED_EDGE ( 'NONE', *, *, #24364, .T. ) ;
#18077 = EDGE_CURVE ( 'NONE', #2729, #22127, #8774, .T. ) ;
#18078 = EDGE_CURVE ( 'NONE', #6435, #15089, #33157, .T. ) ;
#18079 = PRODUCT_DEFINITION_SHAPE ( 'NONE', 'NONE',  #35124 ) ;
#18080 = LINE ( 'NONE', #12379, #20569 ) ;
#18081 = ORIENTED_EDGE ( 'NONE', *, *, #34320, .T. ) ;
#18082 = CIRCLE ( 'NONE', #2703, 8.000000000000007105 ) ;
#18083 = AXIS2_PLACEMENT_3D ( 'NONE', #23852, #34718, #15876 ) ;
#18084 = APPLICATION_CONTEXT ( 'automotive_design' ) ;
#18085 = ORIENTED_EDGE ( 'NONE', *, *, #17850, .T. ) ;
#18086 = DIRECTION ( 'NONE',  ( -1.000000000000000000, -0.000000000000000000, -0.000000000000000000 ) ) ;
#18087 = ORIENTED_EDGE ( 'NONE', *, *, #7254, .T. ) ;
#18088 = ORIENTED_EDGE ( 'NONE', *, *, #3992, .F. ) ;
#18089 = DIRECTION ( 'NONE',  ( 3.697785493223492838E-32, 1.934419779023891545E-16, -1.000000000000000000 ) ) ;
#18090 = ADVANCED_FACE ( 'NONE', ( #14312 ), #65, .F. ) ;
#18091 = CIRCLE ( 'NONE', #26591, 2.525000000000001243 ) ;
#18092 = CARTESIAN_POINT ( 'NONE',  ( -500.0000000000000000, -145.0000000000000000, 187.0000000000000000 ) ) ;
#18093 = DIRECTION ( 'NONE',  ( 1.000000000000000000, 3.040835319149746528E-31, 1.232595164407830946E-32 ) ) ;
#18094 = ORIENTED_EDGE ( 'NONE', *, *, #3992, .T. ) ;
#18095 = ORIENTED_EDGE ( 'NONE', *, *, #18916, .T. ) ;
#18096 = CARTESIAN_POINT ( 'NONE',  ( 0.1859802947476339452, 7.229557500019326177, -31.46177729073534124 ) ) ;
#18097 = CARTESIAN_POINT ( 'NONE',  ( -6.500000000000000000, 0.000000000000000000, -0.7520000000000004459 ) ) ;
#18098 = DIRECTION ( 'NONE',  ( 0.000000000000000000, 0.000000000000000000, 1.000000000000000000 ) ) ;
#18099 = ADVANCED_FACE ( 'NONE', ( #26022 ), #20175, .T. ) ;
#18100 = DIRECTION ( 'NONE',  ( 0.000000000000000000, 0.000000000000000000, -1.000000000000000000 ) ) ;
#18101 = DIRECTION ( 'NONE',  ( 0.000000000000000000, 1.836970198721029688E-16, -1.000000000000000000 ) ) ;
#18102 = EDGE_LOOP ( 'NONE', ( #25536, #2565 ) ) ;
#18103 = ADVANCED_FACE ( 'NONE', ( #9655 ), #3604, .F. ) ;
#18104 = VERTEX_POINT ( 'NONE', #20692 ) ;
#18105 = ADVANCED_FACE ( 'NONE', ( #3783 ), #1641, .T. ) ;
#18106 = CARTESIAN_POINT ( 'NONE',  ( -499.9999999999999432, 112.9999999999999574, -194.9999999999999716 ) ) ;
#18107 = CARTESIAN_POINT ( 'NONE',  ( 0.006892381172647100117, -21.36453267519092591, 22.28230728413997852 ) ) ;
#18108 = VERTEX_POINT ( 'NONE', #9126 ) ;
#18109 = DIRECTION ( 'NONE',  ( 0.000000000000000000, 1.000000000000000000, -3.374343856708137958E-53 ) ) ;
#18110 = EDGE_CURVE ( 'NONE', #20352, #32641, #12791, .T. ) ;
#18111 = CARTESIAN_POINT ( 'NONE',  ( 0.000000000000000000, 3.524919873834583163E-15, 68.31122994652405112 ) ) ;
#18112 = CARTESIAN_POINT ( 'NONE',  ( 50.00050000000000239, 1.224646799147353256E-15, -10.00000000000000000 ) ) ;
#18113 = ORIENTED_EDGE ( 'NONE', *, *, #18677, .T. ) ;
#18114 = VECTOR ( 'NONE', #32029, 1000.000000000000000 ) ;
#18115 = AXIS2_PLACEMENT_3D ( 'NONE', #32854, #13648, #30189 ) ;
#18116 = DIRECTION ( 'NONE',  ( 0.000000000000000000, 1.836970198721029441E-16, -1.000000000000000000 ) ) ;
#18117 = ORIENTED_EDGE ( 'NONE', *, *, #14604, .T. ) ;
#18119 = CARTESIAN_POINT ( 'NONE',  ( 143.0000000000000568, -89.01471862576147487, 43.40376782973931569 ) ) ;
#18118 = DIRECTION ( 'NONE',  ( 1.000000000000000000, 0.000000000000000000, 0.000000000000000000 ) ) ;
#18120 = CARTESIAN_POINT ( 'NONE',  ( -110.0817944407243374, 0.6742432172868401130, 12.48628981526124981 ) ) ;
#18121 = AXIS2_PLACEMENT_3D ( 'NONE', #26905, #7682, #34750 ) ;
#18122 = ORIENTED_EDGE ( 'NONE', *, *, #3213, .T. ) ;
#18123 = EDGE_CURVE ( 'NONE', #13351, #34071, #20514, .T. ) ;
#18124 = DIRECTION ( 'NONE',  ( 0.000000000000000000, 1.000000000000000000, 5.053935297177146739E-49 ) ) ;
#18125 = CARTESIAN_POINT ( 'NONE',  ( -449.9999999999999432, 113.0000000000000000, 154.9999999999999716 ) ) ;
#18126 = VERTEX_POINT ( 'NONE', #31027 ) ;
#18127 = VECTOR ( 'NONE', #13011, 1000.000000000000000 ) ;
#18128 = VECTOR ( 'NONE', #21396, 1000.000000000000000 ) ;
#18129 = CARTESIAN_POINT ( 'NONE',  ( 762.2250564232294892, 1288.051025380799047, 1753.598338701303419 ) ) ;
#18130 = ORIENTED_EDGE ( 'NONE', *, *, #23713, .F. ) ;
#18131 = CARTESIAN_POINT ( 'NONE',  ( 99.26191511054632599, -4.118294838564020743E-16, -7.500000000000000000 ) ) ;
#18132 = VERTEX_POINT ( 'NONE', #28177 ) ;
#18133 = DIRECTION ( 'NONE',  ( 2.736911063134582149E-48, -7.888609052210118054E-31, -1.000000000000000000 ) ) ;
#18134 = CARTESIAN_POINT ( 'NONE',  ( 11.99999999999999645, 124.9999999999999716, 162.9999999999999716 ) ) ;
#18135 = LINE ( 'NONE', #2084, #7792 ) ;
#18136 = CYLINDRICAL_SURFACE ( 'NONE', #31295, 16.19999999999999574 ) ;
#18137 = CONTEXT_DEPENDENT_SHAPE_REPRESENTATION ( #6919, #25365 ) ;
#18138 = ORIENTED_EDGE ( 'NONE', *, *, #27179, .T. ) ;
#18139 = ORIENTED_EDGE ( 'NONE', *, *, #6752, .F. ) ;
#18140 = PRODUCT_DEFINITION_SHAPE ( 'NONE', 'NONE',  #35214 ) ;
#18141 = EDGE_LOOP ( 'NONE', ( #15397, #8451, #34092, #8364, #29283, #4093, #1393, #4988 ) ) ;
#18142 = LINE ( 'NONE', #4221, #27129 ) ;
#18143 = CARTESIAN_POINT ( 'NONE',  ( -19.99999999999996092, 125.0000000000000568, 155.0000000000000000 ) ) ;
#18144 = AXIS2_PLACEMENT_3D ( 'NONE', #24148, #18832, #2788 ) ;
#18145 = ADVANCED_FACE ( 'NONE', ( #25321 ), #12512, .T. ) ;
#18146 = EDGE_CURVE ( 'NONE', #22205, #4014, #23353, .T. ) ;
#18147 = CARTESIAN_POINT ( 'NONE',  ( -499.9999999999999432, 136.9999999999999432, 194.9999999999999716 ) ) ;
#18148 = LINE ( 'NONE', #32165, #14337 ) ;
#18149 = LINE ( 'NONE', #7071, #28806 ) ;
#18150 = SURFACE_SIDE_STYLE ('',( #23294 ) ) ;
#18151 = ORIENTED_EDGE ( 'NONE', *, *, #29038, .T. ) ;
#18152 = FACE_OUTER_BOUND ( 'NONE', #17244, .T. ) ;
#18153 = FACE_OUTER_BOUND ( 'NONE', #128, .T. ) ;
#18154 = DIRECTION ( 'NONE',  ( 0.000000000000000000, -1.000000000000000000, 6.842277657836020854E-49 ) ) ;
#18155 = VERTEX_POINT ( 'NONE', #6624 ) ;
#18156 = CIRCLE ( 'NONE', #23239, 7.999999999999979572 ) ;
#18157 = CARTESIAN_POINT ( 'NONE',  ( 212.5000000000000000, 0.000000000000000000, 10.00000000000000000 ) ) ;
#18158 = ORIENTED_EDGE ( 'NONE', *, *, #16852, .F. ) ;
#18159 = DIRECTION ( 'NONE',  ( 0.000000000000000000, 0.000000000000000000, -1.000000000000000000 ) ) ;
#18160 = CARTESIAN_POINT ( 'NONE',  ( -8.267476927982267298, 31.47782073335735831, 68.31122994652405112 ) ) ;
#18161 = DIRECTION ( 'NONE',  ( -1.000000000000000000, -0.000000000000000000, -0.000000000000000000 ) ) ;
#18162 = LINE ( 'NONE', #4578, #21329 ) ;
#18163 = CARTESIAN_POINT ( 'NONE',  ( -355.0000000000000000, 134.9999999999999716, 113.9999999999999858 ) ) ;
#18164 = ORIENTED_EDGE ( 'NONE', *, *, #2568, .T. ) ;
#18165 = AXIS2_PLACEMENT_3D ( 'NONE', #5057, #443, #5747 ) ;
#18166 = ORIENTED_EDGE ( 'NONE', *, *, #4516, .F. ) ;
#18167 = DIRECTION ( 'NONE',  ( -0.1063910735369017202, 0.9943243633099136947, -1.000770725407181676E-14 ) ) ;
#18168 = EDGE_LOOP ( 'NONE', ( #35022, #33508, #400, #27642, #7784, #30570 ) ) ;
#18169 = LINE ( 'NONE', #4588, #15840 ) ;
#18170 = VECTOR ( 'NONE', #24617, 1000.000000000000000 ) ;
#18171 = DIRECTION ( 'NONE',  ( -0.000000000000000000, -0.000000000000000000, -1.000000000000000000 ) ) ;
#18172 = FACE_OUTER_BOUND ( 'NONE', #14089, .T. ) ;
#18173 = EDGE_LOOP ( 'NONE', ( #5039, #26554, #33341, #22378 ) ) ;
#18174 = LINE ( 'NONE', #9621, #18689 ) ;
#18175 = EDGE_CURVE ( 'NONE', #20191, #13441, #31364, .T. ) ;
#18176 = EDGE_CURVE ( 'NONE', #639, #9452, #17165, .T. ) ;
#18178 = PLANE ( 'NONE',  #28374 ) ;
#18177 = CARTESIAN_POINT ( 'NONE',  ( 2.719010684783665699, 24.79335165344823366, 19.74422662903628023 ) ) ;
#18179 = ORIENTED_EDGE ( 'NONE', *, *, #32786, .T. ) ;
#18180 = ORIENTED_EDGE ( 'NONE', *, *, #33747, .F. ) ;
#18181 = DIRECTION ( 'NONE',  ( -1.000000000000000000, 0.000000000000000000, 0.000000000000000000 ) ) ;
#18182 = ORIENTED_EDGE ( 'NONE', *, *, #4155, .F. ) ;
#18183 = PRODUCT_DEFINITION ( 'UNKNOWN', '', #30925, #18560 ) ;
#18184 = DIRECTION ( 'NONE',  ( -0.000000000000000000, 1.836970198721029688E-16, -1.000000000000000000 ) ) ;
#18185 = CARTESIAN_POINT ( 'NONE',  ( -442.0000000000000000, -105.0000000000000142, 104.0000000000000142 ) ) ;
#18186 = VERTEX_POINT ( 'NONE', #17524 ) ;
#18187 = AXIS2_PLACEMENT_3D ( 'NONE', #24834, #25000, #17520 ) ;
#18188 = DIRECTION ( 'NONE',  ( 1.000000000000000000, 0.000000000000000000, 0.000000000000000000 ) ) ;
#18189 = ORIENTED_EDGE ( 'NONE', *, *, #23719, .F. ) ;
#18190 = DIRECTION ( 'NONE',  ( 0.000000000000000000, 0.000000000000000000, 1.000000000000000000 ) ) ;
#18191 = DIRECTION ( 'NONE',  ( 1.000000000000000000, 0.000000000000000000, 0.000000000000000000 ) ) ;
#18192 = CARTESIAN_POINT ( 'NONE',  ( 2.789999999999999147, 30.27116788629744804, 13.00174666746673147 ) ) ;
#18194 = CARTESIAN_POINT ( 'NONE',  ( -442.0000000000000000, -105.0000000000000142, 104.0000000000000142 ) ) ;
#18193 = CARTESIAN_POINT ( 'NONE',  ( 3.235562306570555532E-30, -15.68591377522703745, -67.50000000000000000 ) ) ;
#18195 = CIRCLE ( 'NONE', #21019, 32.54542015209057126 ) ;
#18196 = CARTESIAN_POINT ( 'NONE',  ( 11.99999999999995559, -134.9999999999999716, -194.9999999999999432 ) ) ;
#18197 = CARTESIAN_POINT ( 'NONE',  ( 0.02407890056655695096, 26.03801215795542134, -16.98986790278583570 ) ) ;
#18198 = CARTESIAN_POINT ( 'NONE',  ( 0.1835380586958561544, -8.814691041839493479, 31.04399216667567529 ) ) ;
#18199 = CARTESIAN_POINT ( 'NONE',  ( -7.700000000000000178, 0.000000000000000000, -15.69999999999999929 ) ) ;
#18200 = ORIENTED_EDGE ( 'NONE', *, *, #13428, .F. ) ;
#18201 = VERTEX_POINT ( 'NONE', #15012 ) ;
#18202 = EDGE_LOOP ( 'NONE', ( #33009, #14423, #1208, #15096 ) ) ;
#18203 = VECTOR ( 'NONE', #18344, 1000.000000000000000 ) ;
#18204 = CARTESIAN_POINT ( 'NONE',  ( 10.00000000000000000, -1.505030548027689319, 3.180000000000000160 ) ) ;
#18205 = CARTESIAN_POINT ( 'NONE',  ( 821.0922591381170150, 1310.683720351004240, 1753.598338701302964 ) ) ;
#18206 = ADVANCED_FACE ( 'NONE', ( #952 ), #19999, .F. ) ;
#18207 = VERTEX_POINT ( 'NONE', #33684 ) ;
#18208 = VERTEX_POINT ( 'NONE', #28357 ) ;
#18209 = ORIENTED_EDGE ( 'NONE', *, *, #8348, .F. ) ;
#18210 = FACE_OUTER_BOUND ( 'NONE', #29371, .T. ) ;
#18211 = ADVANCED_FACE ( 'NONE', ( #30844 ), #33509, .F. ) ;
#18212 = EDGE_LOOP ( 'NONE', ( #30673, #26263, #25820, #6818 ) ) ;
#18213 = DIRECTION ( 'NONE',  ( 1.000000000000000000, 0.000000000000000000, 0.000000000000000000 ) ) ;
#18214 = DIRECTION ( 'NONE',  ( -0.000000000000000000, 0.000000000000000000, 1.000000000000000000 ) ) ;
#18215 = ORIENTED_EDGE ( 'NONE', *, *, #15652, .F. ) ;
#18216 = VERTEX_POINT ( 'NONE', #25852 ) ;
#18217 = LINE ( 'NONE', #16071, #383 ) ;
#18218 = CARTESIAN_POINT ( 'NONE',  ( 10.00000000000000000, 7.794228634059932048, -13.49999999999999822 ) ) ;
#18219 = EDGE_CURVE ( 'NONE', #25754, #28711, #14523, .T. ) ;
#18220 = CARTESIAN_POINT ( 'NONE',  ( 2.789999999999999147, 0.000000000000000000, 0.000000000000000000 ) ) ;
#18221 = CARTESIAN_POINT ( 'NONE',  ( 1.224646799147352862E-15, -49.99999999999999289, 9.999999999999998224 ) ) ;
#18222 = CARTESIAN_POINT ( 'NONE',  ( -499.9999999999999432, -113.0000000000000000, -194.9999999999999716 ) ) ;
#18223 = ORIENTED_EDGE ( 'NONE', *, *, #10313, .T. ) ;
#18224 = DIRECTION ( 'NONE',  ( -0.000000000000000000, 1.000000000000000000, 0.000000000000000000 ) ) ;
#18225 = CARTESIAN_POINT ( 'NONE',  ( -35.00000000000000000, -4.831299144296466785, -15.81122994652406355 ) ) ;
#18226 = EDGE_CURVE ( 'NONE', #27398, #24475, #26439, .T. ) ;
#18227 = VERTEX_POINT ( 'NONE', #17347 ) ;
#18228 = CARTESIAN_POINT ( 'NONE',  ( 5.713835024271038954, 32.03991982186465748, 49.43553178847298568 ) ) ;
#18229 = FACE_OUTER_BOUND ( 'NONE', #14139, .T. ) ;
#18230 = EDGE_CURVE ( 'NONE', #7322, #18350, #17864, .T. ) ;
#18231 = VECTOR ( 'NONE', #33016, 1000.000000000000000 ) ;
#18232 = ADVANCED_FACE ( 'NONE', ( #18210 ), #21568, .T. ) ;
#18233 = DIRECTION ( 'NONE',  ( 1.000000000000000000, 0.000000000000000000, -1.232595164407831220E-32 ) ) ;
#18234 = DIRECTION ( 'NONE',  ( -0.000000000000000000, 0.000000000000000000, 1.000000000000000000 ) ) ;
#18235 = CARTESIAN_POINT ( 'NONE',  ( 1.749999999999999778, 0.000000000000000000, 0.000000000000000000 ) ) ;
#18236 = ORIENTED_EDGE ( 'NONE', *, *, #15465, .F. ) ;
#18237 = CARTESIAN_POINT ( 'NONE',  ( 110.1417579324062217, 2.553994279224888420, -12.23746534924524987 ) ) ;
#18239 = DIRECTION ( 'NONE',  ( -1.300283923313630633E-47, 0.000000000000000000, 1.000000000000000000 ) ) ;
#18238 = CARTESIAN_POINT ( 'NONE',  ( -22.50000000000000355, 0.000000000000000000, 0.000000000000000000 ) ) ;
#18240 = ORIENTED_EDGE ( 'NONE', *, *, #22146, .F. ) ;
#18241 = AXIS2_PLACEMENT_3D ( 'NONE', #25772, #6553, #31129 ) ;
#18242 = DIRECTION ( 'NONE',  ( 1.000000000000000000, 0.000000000000000000, 0.000000000000000000 ) ) ;
#18243 = ORIENTED_EDGE ( 'NONE', *, *, #23285, .F. ) ;
#18244 = ORIENTED_EDGE ( 'NONE', *, *, #29347, .T. ) ;
#18245 = CARTESIAN_POINT ( 'NONE',  ( -20.00000000000007461, 112.9999999999999574, -187.0000000000000000 ) ) ;
#18246 = VERTEX_POINT ( 'NONE', #12867 ) ;
#18247 = ORIENTED_EDGE ( 'NONE', *, *, #10516, .T. ) ;
#18248 = AXIS2_PLACEMENT_3D ( 'NONE', #1532, #29099, #26081 ) ;
#18249 = DIRECTION ( 'NONE',  ( 0.000000000000000000, 1.000000000000000000, 0.000000000000000000 ) ) ;
#18250 = CONICAL_SURFACE ( 'NONE', #33553, 32.54542015209054995, 1.389864428407444175 ) ;
#18251 = CARTESIAN_POINT ( 'NONE',  ( 11.99999999999999645, 144.9999999999999716, 190.9999999999999716 ) ) ;
#18252 = ORIENTED_EDGE ( 'NONE', *, *, #1127, .T. ) ;
#18253 = EDGE_LOOP ( 'NONE', ( #20773, #10608, #12473, #13948 ) ) ;
#18254 = DIRECTION ( 'NONE',  ( -1.000000000000000000, 0.000000000000000000, -0.000000000000000000 ) ) ;
#18255 = DIRECTION ( 'NONE',  ( 1.000000000000000000, 0.000000000000000000, 0.000000000000000000 ) ) ;
#18256 = LINE ( 'NONE', #34089, #3297 ) ;
#18257 = EDGE_CURVE ( 'NONE', #18794, #5262, #34564, .T. ) ;
#18258 = CARTESIAN_POINT ( 'NONE',  ( 60.00000000000000000, -33.69708579775584667, -49.43553178847298568 ) ) ;
#18259 = DIRECTION ( 'NONE',  ( 0.000000000000000000, 0.000000000000000000, 1.000000000000000000 ) ) ;
#18260 = ORIENTED_EDGE ( 'NONE', *, *, #10923, .F. ) ;
#18261 = EDGE_LOOP ( 'NONE', ( #3349, #21859, #23269, #22946, #1266, #2064, #18215, #19219 ) ) ;
#18262 = DIRECTION ( 'NONE',  ( -1.000000000000000000, 0.000000000000000000, -0.000000000000000000 ) ) ;
#18263 = CIRCLE ( 'NONE', #14274, 3.999999999999976019 ) ;
#18264 = EDGE_CURVE ( 'NONE', #2764, #30924, #5000, .T. ) ;
#18265 = EDGE_CURVE ( 'NONE', #2234, #28134, #7596, .T. ) ;
#18266 = DIRECTION ( 'NONE',  ( 1.000000000000000000, 0.000000000000000000, 0.000000000000000000 ) ) ;
#18267 = ORIENTED_EDGE ( 'NONE', *, *, #31144, .F. ) ;
#18268 =( GEOMETRIC_REPRESENTATION_CONTEXT ( 3 ) GLOBAL_UNCERTAINTY_ASSIGNED_CONTEXT ( ( #19639 ) ) GLOBAL_UNIT_ASSIGNED_CONTEXT ( ( #32474, #21286, #4894 ) ) REPRESENTATION_CONTEXT ( 'NONE', 'WORKASPACE' ) );
#18269 = LINE ( 'NONE', #18964, #16303 ) ;
#18270 = CARTESIAN_POINT ( 'NONE',  ( -430.0000000000000000, -119.0000000000000000, 111.9999999999999858 ) ) ;
#18271 = CARTESIAN_POINT ( 'NONE',  ( 2.789999999999999147, -16.83127206196758152, 25.36297913013168426 ) ) ;
#18272 = ORIENTED_EDGE ( 'NONE', *, *, #8464, .T. ) ;
#18273 = PLANE ( 'NONE',  #12123 ) ;
#18274 = ORIENTED_EDGE ( 'NONE', *, *, #22391, .F. ) ;
#18275 = PLANE ( 'NONE',  #16691 ) ;
#18276 = ORIENTED_EDGE ( 'NONE', *, *, #31894, .T. ) ;
#18277 = AXIS2_PLACEMENT_3D ( 'NONE', #32773, #27087, #32594 ) ;
#18279 = DIRECTION ( 'NONE',  ( -0.000000000000000000, -1.836970198721029688E-16, 1.000000000000000000 ) ) ;
#18278 = LINE ( 'NONE', #9562, #19964 ) ;
#18280 = DIRECTION ( 'NONE',  ( -1.000000000000000000, 0.000000000000000000, 0.000000000000000000 ) ) ;
#18281 = EDGE_CURVE ( 'NONE', #23168, #25561, #16066, .T. ) ;
#18282 = AXIS2_PLACEMENT_3D ( 'NONE', #24087, #24123, #8077 ) ;
#18283 = EDGE_LOOP ( 'NONE', ( #29994, #20093, #6378, #2658 ) ) ;
#18284 =( REPRESENTATION_RELATIONSHIP ('NONE','NONE', #23037, #18474 ) REPRESENTATION_RELATIONSHIP_WITH_TRANSFORMATION ( #10881 )SHAPE_REPRESENTATION_RELATIONSHIP( ) );
#18285 = DIRECTION ( 'NONE',  ( 0.000000000000000000, 1.000000000000000000, 1.224646799147353207E-16 ) ) ;
#18286 = CARTESIAN_POINT ( 'NONE',  ( -34.04247984038124031, 16.56841925338180488, 68.31122994652405112 ) ) ;
#18287 = EDGE_CURVE ( 'NONE', #28687, #22784, #16788, .T. ) ;
#18288 = EDGE_LOOP ( 'NONE', ( #2976, #9529, #19653, #30309 ) ) ;
#18289 = EDGE_CURVE ( 'NONE', #25102, #27224, #23706, .T. ) ;
#18290 = EDGE_CURVE ( 'NONE', #11221, #15121, #2334, .T. ) ;
#18291 = AXIS2_PLACEMENT_3D ( 'NONE', #30075, #24720, #11214 ) ;
#18292 = CARTESIAN_POINT ( 'NONE',  ( 777.4389716533775072, 1145.862718864489352, 1753.598338701303192 ) ) ;
#18293 = AXIS2_PLACEMENT_3D ( 'NONE', #31856, #10336, #21196 ) ;
#18294 = EDGE_LOOP ( 'NONE', ( #27414, #11109, #1163, #21888 ) ) ;
#18295 = CARTESIAN_POINT ( 'NONE',  ( 109.3188951714813157, -3.796349414716898796, 11.91283353888524310 ) ) ;
#18296 = ORIENTED_EDGE ( 'NONE', *, *, #34835, .F. ) ;
#18297 = COLOUR_RGB ( '',0.7921568627450980005, 0.8196078431372548767, 0.9333333333333333481 ) ;
#18298 = CARTESIAN_POINT ( 'NONE',  ( 2.789999999999999147, -14.75935258146392570, -26.65732927035534772 ) ) ;
#18299 = ADVANCED_FACE ( 'NONE', ( #15714 ), #31873, .F. ) ;
#18300 = DIRECTION ( 'NONE',  ( -3.040835319149746528E-31, -1.000000000000000000, 0.000000000000000000 ) ) ;
#18301 = DIRECTION ( 'NONE',  ( 0.000000000000000000, 0.000000000000000000, -1.000000000000000000 ) ) ;
#18302 = CARTESIAN_POINT ( 'NONE',  ( -20.02113311122488781, 4.168562732279007754, -87.50000000000000000 ) ) ;
#18303 = ITEM_DEFINED_TRANSFORMATION ( 'NONE', 'NONE', #11003,  #28566 ) ;
#18304 = ORIENTED_EDGE ( 'NONE', *, *, #24953, .T. ) ;
#18305 = ORIENTED_EDGE ( 'NONE', *, *, #20872, .F. ) ;
#18306 = ORIENTED_EDGE ( 'NONE', *, *, #2646, .F. ) ;
#18307 = CYLINDRICAL_SURFACE ( 'NONE', #31134, 15.00000000000000000 ) ;
#18309 = VECTOR ( 'NONE', #33161, 1000.000000000000000 ) ;
#18308 = DIRECTION ( 'NONE',  ( -1.000000000000000000, -0.000000000000000000, -0.000000000000000000 ) ) ;
#18310 = DIRECTION ( 'NONE',  ( 0.000000000000000000, 1.000000000000000000, 0.000000000000000000 ) ) ;
#18311 = ADVANCED_FACE ( 'NONE', ( #33772 ), #28867, .F. ) ;
#18312 = EDGE_CURVE ( 'NONE', #9284, #27942, #7142, .T. ) ;
#18313 = CARTESIAN_POINT ( 'NONE',  ( 3.235562306570555532E-30, -15.68591377522703745, -67.50000000000000000 ) ) ;
#18314 = DIRECTION ( 'NONE',  ( 1.000000000000000000, 0.000000000000000000, 0.000000000000000000 ) ) ;
#18315 = VERTEX_POINT ( 'NONE', #34741 ) ;
#18316 = PRODUCT_DEFINITION_SHAPE ( 'NONE', 'NONE',  #35160 ) ;
#18317 = PLANE ( 'NONE',  #21394 ) ;
#18318 = CARTESIAN_POINT ( 'NONE',  ( 0.02407890056655695096, 26.03801215795542134, -16.98986790278583570 ) ) ;
#18319 = VECTOR ( 'NONE', #29694, 1000.000000000000000 ) ;
#18320 = DIRECTION ( 'NONE',  ( -0.000000000000000000, 1.000000000000000000, -0.000000000000000000 ) ) ;
#18321 = ORIENTED_EDGE ( 'NONE', *, *, #30261, .T. ) ;
#18322 = VECTOR ( 'NONE', #31256, 1000.000000000000000 ) ;
#18323 = VECTOR ( 'NONE', #20253, 1000.000000000000000 ) ;
#18324 = CARTESIAN_POINT ( 'NONE',  ( 0.000000000000000000, 0.000000000000000000, -13.49999999999999822 ) ) ;
#18325 = VERTEX_POINT ( 'NONE', #26722 ) ;
#18326 = VECTOR ( 'NONE', #32558, 1000.000000000000000 ) ;
#18327 = CARTESIAN_POINT ( 'NONE',  ( 2.033589660297129065, -25.08336923281130026, -22.82737131378450357 ) ) ;
#18328 = FACE_OUTER_BOUND ( 'NONE', #14358, .T. ) ;
#18329 = ORIENTED_EDGE ( 'NONE', *, *, #6102, .T. ) ;
#18330 = CARTESIAN_POINT ( 'NONE',  ( 2.789999999999999147, -29.69698570178010755, -11.75786841620047163 ) ) ;
#18331 = CARTESIAN_POINT ( 'NONE',  ( -18.07349068442141515, -27.06572199953722446, 68.31122994652405112 ) ) ;
#18332 = DIRECTION ( 'NONE',  ( -0.8835120444460228262, 0.4684084406997903183, 0.000000000000000000 ) ) ;
#18333 = ORIENTED_EDGE ( 'NONE', *, *, #18146, .F. ) ;
#18334 = EDGE_CURVE ( 'NONE', #23700, #7091, #18043, .T. ) ;
#18335 = EDGE_CURVE ( 'NONE', #13338, #34601, #9406, .T. ) ;
#18336 = ORIENTED_EDGE ( 'NONE', *, *, #22907, .T. ) ;
#18337 = CARTESIAN_POINT ( 'NONE',  ( 762.9165980246000345, 1281.587920539148399, 1753.598338701303419 ) ) ;
#18338 =( REPRESENTATION_RELATIONSHIP ('NONE','NONE', #23037, #28231 ) REPRESENTATION_RELATIONSHIP_WITH_TRANSFORMATION ( #2169 )SHAPE_REPRESENTATION_RELATIONSHIP( ) );
#18339 = ORIENTED_EDGE ( 'NONE', *, *, #1161, .F. ) ;
#18340 = EDGE_CURVE ( 'NONE', #21426, #13149, #7494, .T. ) ;
#18341 = CARTESIAN_POINT ( 'NONE',  ( 2.783107595519907829, -29.45646641510990804, -9.233692607046043221 ) ) ;
#18342 = VECTOR ( 'NONE', #22329, 1000.000000000000000 ) ;
#18343 = CARTESIAN_POINT ( 'NONE',  ( 129.3530333899765594, -6.000000000000000000, 62.49999999999999289 ) ) ;
#18344 = DIRECTION ( 'NONE',  ( -0.000000000000000000, -1.000000000000000000, -0.000000000000000000 ) ) ;
#18346 = EDGE_CURVE ( 'NONE', #26887, #10822, #10351, .T. ) ;
#18345 = ORIENTED_EDGE ( 'NONE', *, *, #10774, .F. ) ;
#18347 = LINE ( 'NONE', #13000, #15283 ) ;
#18349 = PLANE ( 'NONE',  #19819 ) ;
#18348 = DIRECTION ( 'NONE',  ( -0.000000000000000000, -0.000000000000000000, 1.000000000000000000 ) ) ;
#18350 = VERTEX_POINT ( 'NONE', #34388 ) ;
#18351 = ORIENTED_EDGE ( 'NONE', *, *, #18466, .F. ) ;
#18352 = CARTESIAN_POINT ( 'NONE',  ( -36.04853892210774546, 11.59936550071286909, 29.04209251724894614 ) ) ;
#18353 = ORIENTED_EDGE ( 'NONE', *, *, #21355, .T. ) ;
#18354 = LINE ( 'NONE', #10510, #18127 ) ;
#18355 = LINE ( 'NONE', #18185, #8020 ) ;
#18356 = ORIENTED_EDGE ( 'NONE', *, *, #9871, .F. ) ;
#18357 = CARTESIAN_POINT ( 'NONE',  ( -499.9999999999999432, 136.9999999999999432, 155.0000000000000000 ) ) ;
#18358 = ORIENTED_EDGE ( 'NONE', *, *, #25662, .F. ) ;
#18359 = ADVANCED_FACE ( 'NONE', ( #15360 ), #26190, .T. ) ;
#18360 = DIRECTION ( 'NONE',  ( 0.000000000000000000, 0.000000000000000000, 1.000000000000000000 ) ) ;
#18361 = PLANE ( 'NONE',  #4603 ) ;
#18362 = CARTESIAN_POINT ( 'NONE',  ( 19.99999999999996092, -134.9999999999999716, 162.9999999999999716 ) ) ;
#18365 = CARTESIAN_POINT ( 'NONE',  ( 5.021133111224576062, 16.12922284503173742, -67.50000000000000000 ) ) ;
#18364 = DIRECTION ( 'NONE',  ( 1.000000000000000000, 0.000000000000000000, 0.000000000000000000 ) ) ;
#18363 = AXIS2_PLACEMENT_3D ( 'NONE', #13720, #18377, #32570 ) ;
#18366 = CIRCLE ( 'NONE', #16081, 7.999999999999979572 ) ;
#18367 = AXIS2_PLACEMENT_3D ( 'NONE', #11275, #583, #3416 ) ;
#18368 = CIRCLE ( 'NONE', #23455, 3.999999999999976019 ) ;
#18369 = DIRECTION ( 'NONE',  ( 0.000000000000000000, 2.309213040847544338E-50, 1.000000000000000000 ) ) ;
#18370 = DIRECTION ( 'NONE',  ( -1.000000000000000000, 0.000000000000000000, -0.000000000000000000 ) ) ;
#18371 = CARTESIAN_POINT ( 'NONE',  ( 19.99999999999998934, -145.0000000000000000, 187.0000000000000000 ) ) ;
#18372 = FACE_OUTER_BOUND ( 'NONE', #12171, .T. ) ;
#18373 = EDGE_CURVE ( 'NONE', #29267, #13790, #21894, .T. ) ;
#18374 = ADVANCED_FACE ( 'NONE', ( #13561 ), #27075, .F. ) ;
#18375 = EDGE_CURVE ( 'NONE', #13276, #11080, #11067, .T. ) ;
#18376 = ORIENTED_EDGE ( 'NONE', *, *, #4536, .T. ) ;
#18377 = DIRECTION ( 'NONE',  ( 0.9999999999999998890, 1.035282970462958947E-14, -6.982962677686263555E-15 ) ) ;
#18378 = ORIENTED_EDGE ( 'NONE', *, *, #33134, .T. ) ;
#18379 = EDGE_LOOP ( 'NONE', ( #15600, #9718, #4820, #21160 ) ) ;
#18380 = AXIS2_PLACEMENT_3D ( 'NONE', #31560, #29424, #12529 ) ;
#18381 = EDGE_LOOP ( 'NONE', ( #22216, #9968, #2931, #13914 ) ) ;
#18382 = ORIENTED_EDGE ( 'NONE', *, *, #23686, .T. ) ;
#18383 = VERTEX_POINT ( 'NONE', #29749 ) ;
#18384 = DIRECTION ( 'NONE',  ( 0.000000000000000000, 1.836970198721029441E-16, -1.000000000000000000 ) ) ;
#18385 = FACE_OUTER_BOUND ( 'NONE', #9488, .T. ) ;
#18386 = AXIS2_PLACEMENT_3D ( 'NONE', #12818, #29174, #29354 ) ;
#18387 = CARTESIAN_POINT ( 'NONE',  ( 0.000000000000000000, 0.000000000000000000, -0.7500000000000000000 ) ) ;
#18388 = AXIS2_PLACEMENT_3D ( 'NONE', #18839, #5284, #16174 ) ;
#18389 = FACE_OUTER_BOUND ( 'NONE', #18764, .T. ) ;
#18390 = ORIENTED_EDGE ( 'NONE', *, *, #18340, .F. ) ;
#18391 = VERTEX_POINT ( 'NONE', #24564 ) ;
#18392 = AXIS2_PLACEMENT_3D ( 'NONE', #13755, #16085, #2535 ) ;
#18393 = CYLINDRICAL_SURFACE ( 'NONE', #30488, 7.999999999999979572 ) ;
#18394 = CARTESIAN_POINT ( 'NONE',  ( -7.700000000000000178, 0.000000000000000000, 0.000000000000000000 ) ) ;
#18395 = DIRECTION ( 'NONE',  ( -1.000000000000000000, -0.000000000000000000, -0.000000000000000000 ) ) ;
#18396 = DIRECTION ( 'NONE',  ( -1.000000000000000000, 0.000000000000000000, -5.546364386991661285E-52 ) ) ;
#18397 = DIRECTION ( 'NONE',  ( -1.000000000000000000, 0.000000000000000000, 0.000000000000000000 ) ) ;
#18398 = VERTEX_POINT ( 'NONE', #5522 ) ;
#18399 = FACE_OUTER_BOUND ( 'NONE', #32064, .T. ) ;
#18400 = PLANE ( 'NONE',  #9439 ) ;
#18401 = FACE_OUTER_BOUND ( 'NONE', #15684, .T. ) ;
#18402 = DIRECTION ( 'NONE',  ( 0.000000000000000000, 1.000000000000000000, 1.224646799147353207E-16 ) ) ;
#18403 = CARTESIAN_POINT ( 'NONE',  ( 110.6976704948526020, 0.7843626702862538380, -7.468944954497490407 ) ) ;
#18405 = CARTESIAN_POINT ( 'NONE',  ( -110.0793211855294658, 0.6938560566811355912, -7.475525031754234995 ) ) ;
#18404 = CARTESIAN_POINT ( 'NONE',  ( 2.719010716928600857, 19.10423307544339622, 25.28978101402055145 ) ) ;
#18406 = AXIS2_PLACEMENT_3D ( 'NONE', #19911, #33418, #22577 ) ;
#18407 = EDGE_CURVE ( 'NONE', #13218, #29274, #16242, .T. ) ;
#18408 = DIRECTION ( 'NONE',  ( 1.000000000000000000, 0.000000000000000000, -1.232595164407831220E-32 ) ) ;
#18409 = ORIENTED_EDGE ( 'NONE', *, *, #19013, .F. ) ;
#18410 = CARTESIAN_POINT ( 'NONE',  ( -442.0000000000000000, 124.9999999999999432, -155.0000000000000000 ) ) ;
#18412 = DIRECTION ( 'NONE',  ( 1.000000000000000000, 0.000000000000000000, -1.232595164407831220E-32 ) ) ;
#18411 = DIRECTION ( 'NONE',  ( 0.000000000000000000, -1.000000000000000000, 0.000000000000000000 ) ) ;
#18413 = EDGE_CURVE ( 'NONE', #16274, #12217, #18515, .T. ) ;
#18414 = AXIS2_PLACEMENT_3D ( 'NONE', #4024, #3688, #15094 ) ;
#18415 = EDGE_CURVE ( 'NONE', #10097, #7307, #11410, .T. ) ;
#18417 = VERTEX_POINT ( 'NONE', #14090 ) ;
#18416 = VECTOR ( 'NONE', #28024, 1000.000000000000000 ) ;
#18418 = CIRCLE ( 'NONE', #12168, 4.306175033202026547 ) ;
#18419 = PLANE ( 'NONE',  #8660 ) ;
#18420 = PRODUCT_DEFINITION_SHAPE ( 'NONE', 'NONE',  #35222 ) ;
#18421 = EDGE_CURVE ( 'NONE', #33196, #8817, #21, .T. ) ;
#18422 = EDGE_LOOP ( 'NONE', ( #31903, #27595, #33467, #2289 ) ) ;
#18423 = ORIENTED_EDGE ( 'NONE', *, *, #7584, .T. ) ;
#18424 = LINE ( 'NONE', #31580, #32642 ) ;
#18425 = ORIENTED_EDGE ( 'NONE', *, *, #14831, .T. ) ;
#18426 = VERTEX_POINT ( 'NONE', #27248 ) ;
#18427 = DIRECTION ( 'NONE',  ( -0.000000000000000000, -1.131431318426415506E-52, -1.000000000000000000 ) ) ;
#18428 = EDGE_CURVE ( 'NONE', #18484, #18104, #22270, .T. ) ;
#18429 = VECTOR ( 'NONE', #17215, 1000.000000000000000 ) ;
#18430 = CARTESIAN_POINT ( 'NONE',  ( -19.99999999999998934, -112.9999999999999858, 155.0000000000000000 ) ) ;
#18431 = CARTESIAN_POINT ( 'NONE',  ( -355.0000000000000000, 114.9999999999999716, 126.0000000000000000 ) ) ;
#18432 = VERTEX_POINT ( 'NONE', #200 ) ;
#18433 = ORIENTED_EDGE ( 'NONE', *, *, #9965, .T. ) ;
#18434 = DIRECTION ( 'NONE',  ( -1.000000000000000000, 0.000000000000000000, 0.000000000000000000 ) ) ;
#18435 = CARTESIAN_POINT ( 'NONE',  ( 0.000000000000000000, -29.91351748324100512, -5.799410679710955030 ) ) ;
#18436 = PLANE ( 'NONE',  #31694 ) ;
#18437 = CARTESIAN_POINT ( 'NONE',  ( 8.000000000000000000, 15.69999999999999929, 0.000000000000000000 ) ) ;
#18438 = LINE ( 'NONE', #34801, #27909 ) ;
#18439 = UNCERTAINTY_MEASURE_WITH_UNIT (LENGTH_MEASURE( 1.000000000000000082E-05 ), #22430, 'distance_accuracy_value', 'NONE');
#18440 = VERTEX_POINT ( 'NONE', #30457 ) ;
#18441 = CARTESIAN_POINT ( 'NONE',  ( 22.89764159710613001, 8.346743312457579833, -77.50000000000000000 ) ) ;
#18442 = CARTESIAN_POINT ( 'NONE',  ( -500.0000000000000000, -109.0000000000000142, 162.9999999999999716 ) ) ;
#18443 = VECTOR ( 'NONE', #8578, 1000.000000000000000 ) ;
#18444 = CIRCLE ( 'NONE', #12200, 3.999999999999948042 ) ;
#18445 = FACE_OUTER_BOUND ( 'NONE', #49, .T. ) ;
#18446 = VERTEX_POINT ( 'NONE', #10886 ) ;
#18447 = CIRCLE ( 'NONE', #29810, 4.750000000000004441 ) ;
#18448 = LINE ( 'NONE', #29288, #18012 ) ;
#18449 = DIRECTION ( 'NONE',  ( 1.000000000000000000, 0.000000000000000000, 0.000000000000000000 ) ) ;
#18450 = FACE_OUTER_BOUND ( 'NONE', #2570, .T. ) ;
#18451 = ORIENTED_EDGE ( 'NONE', *, *, #27373, .T. ) ;
#18452 = LINE ( 'NONE', #18112, #3553 ) ;
#18453 = ORIENTED_EDGE ( 'NONE', *, *, #17908, .T. ) ;
#18454 = DIRECTION ( 'NONE',  ( 0.000000000000000000, 0.000000000000000000, 1.000000000000000000 ) ) ;
#18455 = VERTEX_POINT ( 'NONE', #33114 ) ;
#18457 = CARTESIAN_POINT ( 'NONE',  ( -20.00000000000007461, 140.9999999999999716, 162.9999999999999716 ) ) ;
#18456 = CARTESIAN_POINT ( 'NONE',  ( -499.9999999999999432, 112.9999999999999574, 155.0000000000000000 ) ) ;
#18458 = DIRECTION ( 'NONE',  ( -0.000000000000000000, -1.000000000000000000, -0.000000000000000000 ) ) ;
#18459 = EDGE_CURVE ( 'NONE', #32641, #21769, #25293, .T. ) ;
#18460 = CIRCLE ( 'NONE', #11083, 2.033421858999711951 ) ;
#18461 = VERTEX_POINT ( 'NONE', #3036 ) ;
#18462 = FACE_OUTER_BOUND ( 'NONE', #10381, .T. ) ;
#18463 = FACE_OUTER_BOUND ( 'NONE', #18975, .T. ) ;
#18464 = EDGE_CURVE ( 'NONE', #15074, #10505, #8730, .T. ) ;
#18465 = VECTOR ( 'NONE', #7451, 1000.000000000000000 ) ;
#18466 = EDGE_CURVE ( 'NONE', #15452, #19731, #8027, .T. ) ;
#18467 = VERTEX_POINT ( 'NONE', #16953 ) ;
#18468 = CARTESIAN_POINT ( 'NONE',  ( 2.013160256205026144, 31.37535259441678903, 12.97259700501048840 ) ) ;
#18469 = VECTOR ( 'NONE', #45, 1000.000000000000000 ) ;
#18470 = EDGE_CURVE ( 'NONE', #15934, #20393, #14267, .T. ) ;
#18471 = EDGE_CURVE ( 'NONE', #10892, #6969, #28698, .T. ) ;
#18472 = CARTESIAN_POINT ( 'NONE',  ( 764.9912228287111020, 1262.198606014197139, 1753.598338701303874 ) ) ;
#18473 = AXIS2_PLACEMENT_3D ( 'NONE', #29773, #16270, #8414 ) ;
#18474 = SHAPE_REPRESENTATION ( 'shaft', ( #28566 ), #32533 ) ;
#18475 = VERTEX_POINT ( 'NONE', #30271 ) ;
#18476 = CARTESIAN_POINT ( 'NONE',  ( 106.8634821253765637, -5.440007577125886229, 11.25529792293082032 ) ) ;
#18477 = EDGE_LOOP ( 'NONE', ( #2361, #26654, #8165, #26874 ) ) ;
#18478 = DIRECTION ( 'NONE',  ( 0.000000000000000000, -1.000000000000000000, -2.309213040847544338E-50 ) ) ;
#18479 = VECTOR ( 'NONE', #11197, 1000.000000000000000 ) ;
#18480 = CARTESIAN_POINT ( 'NONE',  ( 0.000000000000000000, -5.984944020945660803, -31.37417528048448645 ) ) ;
#18481 = CARTESIAN_POINT ( 'NONE',  ( -106.3678849252397640, -4.940539628404770234, -5.643550520051347164 ) ) ;
#18482 = DIRECTION ( 'NONE',  ( 0.000000000000000000, 0.000000000000000000, -1.000000000000000000 ) ) ;
#18483 = ITEM_DEFINED_TRANSFORMATION ( 'NONE', 'NONE', #23498,  #28566 ) ;
#18484 = VERTEX_POINT ( 'NONE', #13730 ) ;
#18485 = ORIENTED_EDGE ( 'NONE', *, *, #4792, .T. ) ;
#18486 = VERTEX_POINT ( 'NONE', #11598 ) ;
#18487 = CARTESIAN_POINT ( 'NONE',  ( -355.0000000000000000, -117.0000000000000000, 113.9999999999999858 ) ) ;
#18488 = EDGE_CURVE ( 'NONE', #31361, #16565, #24995, .T. ) ;
#18489 = CYLINDRICAL_SURFACE ( 'NONE', #29592, 7.500000000000000000 ) ;
#18490 = AXIS2_PLACEMENT_3D ( 'NONE', #12732, #18427, #34435 ) ;
#18491 = LINE ( 'NONE', #10459, #12247 ) ;
#18492 = CYLINDRICAL_SURFACE ( 'NONE', #29655, 3.999999999999976019 ) ;
#18493 = LINE ( 'NONE', #29331, #26006 ) ;
#18494 = FACE_OUTER_BOUND ( 'NONE', #4947, .T. ) ;
#18495 = ORIENTED_EDGE ( 'NONE', *, *, #21380, .F. ) ;
#18496 = VECTOR ( 'NONE', #6370, 1000.000000000000000 ) ;
#18497 = DIRECTION ( 'NONE',  ( 1.848892746611746419E-32, 6.842277657836020854E-49, -1.000000000000000000 ) ) ;
#18498 = DIRECTION ( 'NONE',  ( 0.000000000000000000, -1.000000000000000000, 1.131431318426415506E-52 ) ) ;
#18499 = CARTESIAN_POINT ( 'NONE',  ( -355.0000000000000000, 135.0000000000000000, 130.0000000000000000 ) ) ;
#18501 = EDGE_CURVE ( 'NONE', #3150, #23862, #2857, .T. ) ;
#18500 = VERTEX_POINT ( 'NONE', #29929 ) ;
#18502 = CIRCLE ( 'NONE', #21328, 4.750000000000004441 ) ;
#18503 = EDGE_CURVE ( 'NONE', #35039, #10023, #13372, .T. ) ;
#18504 = AXIS2_PLACEMENT_3D ( 'NONE', #9075, #25078, #11764 ) ;
#18505 = CARTESIAN_POINT ( 'NONE',  ( 1.205771365940050854, -7.794228634059966687, -13.49999999999999822 ) ) ;
#18506 = ORIENTED_EDGE ( 'NONE', *, *, #7857, .F. ) ;
#18508 = CLOSED_SHELL ( 'NONE', ( #22171, #11133, #20628, #27601, #21842, #30706, #29494, #26831, #10666, #22042, #16315, #2974, #22477, #13281, #1794, #31461, #16001, #29594 ) ) ;
#18507 = CARTESIAN_POINT ( 'NONE',  ( -102.7184718528696692, 4.590414103366520671, -11.62745871345765458 ) ) ;
#18509 = PLANE ( 'NONE',  #29782 ) ;
#18510 = ORIENTED_EDGE ( 'NONE', *, *, #9484, .T. ) ;
#18511 = DIRECTION ( 'NONE',  ( 1.000000000000000000, 0.000000000000000000, -0.000000000000000000 ) ) ;
#18512 = CARTESIAN_POINT ( 'NONE',  ( 22.50000000000000355, 2.755455298081545172E-15, 20.00000000000000000 ) ) ;
#18513 = DIRECTION ( 'NONE',  ( -1.000000000000000000, 0.000000000000000000, 0.000000000000000000 ) ) ;
#18514 = ORIENTED_EDGE ( 'NONE', *, *, #4792, .F. ) ;
#18515 = CIRCLE ( 'NONE', #22464, 32.54542015209055705 ) ;
#18516 = ORIENTED_EDGE ( 'NONE', *, *, #23509, .T. ) ;
#18517 = EDGE_CURVE ( 'NONE', #1469, #5175, #8912, .T. ) ;
#18518 = ADVANCED_FACE ( 'NONE', ( #3745 ), #20475, .F. ) ;
#18519 = CARTESIAN_POINT ( 'NONE',  ( 758.7673484163781268, 1320.366549589051601, 1753.598338701303419 ) ) ;
#18520 = VECTOR ( 'NONE', #32466, 999.9999999999998863 ) ;
#18521 = EDGE_LOOP ( 'NONE', ( #20096, #9365, #26954, #24804 ) ) ;
#18522 = CIRCLE ( 'NONE', #3143, 1.649999999999999467 ) ;
#18523 = CARTESIAN_POINT ( 'NONE',  ( -15.99999999999998579, 75.55999999999990280, -172.9900000000000091 ) ) ;
#18524 = DIRECTION ( 'NONE',  ( 0.000000000000000000, 1.000000000000000000, 5.145227585319922065E-49 ) ) ;
#18525 = DIRECTION ( 'NONE',  ( -1.000000000000000000, 0.000000000000000000, 0.000000000000000000 ) ) ;
#18526 = CYLINDRICAL_SURFACE ( 'NONE', #21880, 5.115020388170798959 ) ;
#18527 = CARTESIAN_POINT ( 'NONE',  ( 106.5474496464479728, -5.538930788889586232, 5.058095442343715220 ) ) ;
#18528 = ITEM_DEFINED_TRANSFORMATION ( 'NONE', 'NONE', #21189,  #28566 ) ;
#18529 = ORIENTED_EDGE ( 'NONE', *, *, #9275, .T. ) ;
#18530 = DIRECTION ( 'NONE',  ( 1.000000000000000000, -0.000000000000000000, -0.000000000000000000 ) ) ;
#18532 = FACE_OUTER_BOUND ( 'NONE', #22493, .T. ) ;
#18531 = DIRECTION ( 'NONE',  ( 1.000000000000000000, 0.000000000000000000, 0.000000000000000000 ) ) ;
#18533 = ORIENTED_EDGE ( 'NONE', *, *, #22869, .T. ) ;
#18534 = ORIENTED_EDGE ( 'NONE', *, *, #15750, .F. ) ;
#18535 = LINE ( 'NONE', #26692, #11206 ) ;
#18536 = VERTEX_POINT ( 'NONE', #17649 ) ;
#18537 = EDGE_CURVE ( 'NONE', #5880, #31793, #31320, .T. ) ;
#18538 = CARTESIAN_POINT ( 'NONE',  ( 2.789999999999999147, -20.35927063852789232, -24.61013060777193218 ) ) ;
#18539 = CARTESIAN_POINT ( 'NONE',  ( 2.789999999999999147, -5.984944020945660803, -31.37417528048448645 ) ) ;
#18540 = ORIENTED_EDGE ( 'NONE', *, *, #24210, .F. ) ;
#18541 = ADVANCED_FACE ( 'NONE', ( #4078 ), #6930, .T. ) ;
#18542 = ADVANCED_FACE ( 'NONE', ( #17820 ), #25626, .T. ) ;
#18543 = VECTOR ( 'NONE', #6680, 1000.000000000000000 ) ;
#18544 = DIRECTION ( 'NONE',  ( -0.000000000000000000, 1.000000000000000000, -0.000000000000000000 ) ) ;
#18545 = DIRECTION ( 'NONE',  ( 1.000000000000000000, 0.000000000000000000, 0.000000000000000000 ) ) ;
#18546 = EDGE_LOOP ( 'NONE', ( #16112, #13783, #12456, #18247 ) ) ;
#18547 = CIRCLE ( 'NONE', #34426, 44.99999999999997158 ) ;
#18548 = CARTESIAN_POINT ( 'NONE',  ( -442.0000000000000000, 105.0000000000000142, 155.0000000000000000 ) ) ;
#18549 = ADVANCED_FACE ( 'NONE', ( #11952 ), #14973, .F. ) ;
#18550 = CARTESIAN_POINT ( 'NONE',  ( 2.033589656297370318, -29.46130761496106842, 16.80165608683625678 ) ) ;
#18552 = LINE ( 'NONE', #15882, #1482 ) ;
#18551 = CARTESIAN_POINT ( 'NONE',  ( 10.17231796313409298, 8.346743312457579833, -77.50000000000000000 ) ) ;
#18553 = EDGE_CURVE ( 'NONE', #13770, #14420, #23156, .T. ) ;
#18554 =( REPRESENTATION_RELATIONSHIP ('NONE','NONE', #23037, #15767 ) REPRESENTATION_RELATIONSHIP_WITH_TRANSFORMATION ( #18528 )SHAPE_REPRESENTATION_RELATIONSHIP( ) );
#18555 = FACE_OUTER_BOUND ( 'NONE', #7664, .T. ) ;
#18556 = CARTESIAN_POINT ( 'NONE',  ( 0.000000000000000000, 17.11426446101236820, -26.96776559937708129 ) ) ;
#18557 = CARTESIAN_POINT ( 'NONE',  ( 11.99999999999999645, 144.9999999999999716, -194.9999999999999432 ) ) ;
#18558 = VECTOR ( 'NONE', #12763, 1000.000000000000227 ) ;
#18559 = ORIENTED_EDGE ( 'NONE', *, *, #24746, .T. ) ;
#18560 = PRODUCT_DEFINITION_CONTEXT ( 'detailed design', #29647, 'design' ) ;
#18561 = VERTEX_POINT ( 'NONE', #14450 ) ;
#18562 = VERTEX_POINT ( 'NONE', #31161 ) ;
#18563 = CARTESIAN_POINT ( 'NONE',  ( 8.000000000000000000, 0.000000000000000000, 0.000000000000000000 ) ) ;
#18564 = DIRECTION ( 'NONE',  ( 0.9985951607324108359, 0.05298778125012505030, 1.957465783887502089E-14 ) ) ;
#18565 = ORIENTED_EDGE ( 'NONE', *, *, #26666, .T. ) ;
#18566 = VERTEX_POINT ( 'NONE', #4260 ) ;
#18567 = CARTESIAN_POINT ( 'NONE',  ( 0.006892381754031734996, 20.89684813776007388, 22.72149230800640751 ) ) ;
#18568 = VECTOR ( 'NONE', #28329, 1000.000000000000000 ) ;
#18569 = CARTESIAN_POINT ( 'NONE',  ( 0.000000000000000000, 0.000000000000000000, 0.000000000000000000 ) ) ;
#18570 = CONTEXT_DEPENDENT_SHAPE_REPRESENTATION ( #3759, #33528 ) ;
#18571 = PLANE ( 'NONE',  #17550 ) ;
#18572 = DIRECTION ( 'NONE',  ( 0.000000000000000000, 0.000000000000000000, 1.000000000000000000 ) ) ;
#18573 = ORIENTED_EDGE ( 'NONE', *, *, #29386, .T. ) ;
#18574 = ORIENTED_EDGE ( 'NONE', *, *, #19067, .F. ) ;
#18575 = CARTESIAN_POINT ( 'NONE',  ( -143.0000000000000568, -175.8248315648716016, -46.05325008164005851 ) ) ;
#18576 = CARTESIAN_POINT ( 'NONE',  ( -41.91706493227329133, 16.36947364650383818, -36.69637551990492597 ) ) ;
#18577 = AXIS2_PLACEMENT_3D ( 'NONE', #27669, #625, #11486 ) ;
#18578 = CARTESIAN_POINT ( 'NONE',  ( 0.000000000000000000, 3.524919873834583163E-15, 68.31122994652405112 ) ) ;
#18579 = CARTESIAN_POINT ( 'NONE',  ( -12.00000000000001243, 144.9999999999999716, -154.9999999999999716 ) ) ;
#18580 = CARTESIAN_POINT ( 'NONE',  ( 0.000000000000000000, 0.000000000000000000, 13.00000000000000000 ) ) ;
#18581 = VERTEX_POINT ( 'NONE', #28484 ) ;
#18582 = ADVANCED_FACE ( 'NONE', ( #30984 ), #27003, .T. ) ;
#18583 = PLANE ( 'NONE',  #16937 ) ;
#18584 = DIRECTION ( 'NONE',  ( -0.8854131517428557308, 0.2458337514780905841, 0.3944734685057932899 ) ) ;
#18585 = EDGE_CURVE ( 'NONE', #5208, #169, #864, .T. ) ;
#18586 = CARTESIAN_POINT ( 'NONE',  ( 31.73435513276361775, 7.220462394039765641, 49.43553178847298568 ) ) ;
#18587 = DIRECTION ( 'NONE',  ( -1.000000000000000000, 0.000000000000000000, 0.000000000000000000 ) ) ;
#18589 = DIRECTION ( 'NONE',  ( 1.000000000000000000, 0.000000000000000000, 0.000000000000000000 ) ) ;
#18588 = CARTESIAN_POINT ( 'NONE',  ( -12.25939112814508825, 30.14816249862101927, 68.31122994652405112 ) ) ;
#18590 = CARTESIAN_POINT ( 'NONE',  ( -20.00000000000007461, 136.9999999999999432, 187.0000000000000000 ) ) ;
#18591 = EDGE_LOOP ( 'NONE', ( #7427, #10732, #22606, #30710 ) ) ;
#18592 = CARTESIAN_POINT ( 'NONE',  ( 102.1149735546430435, 4.974089543361916554, -11.46991629550682035 ) ) ;
#18594 = CARTESIAN_POINT ( 'NONE',  ( 0.1387913946425707035, 10.37119081301007739, -9.036570576874957794 ) ) ;
#18593 = DIRECTION ( 'NONE',  ( -1.000000000000000000, -3.469446951953834515E-18, 0.000000000000000000 ) ) ;
#18595 = ORIENTED_EDGE ( 'NONE', *, *, #12244, .F. ) ;
#18596 = CARTESIAN_POINT ( 'NONE',  ( 12.00000000000003730, -115.0000000000000000, -154.9999999999999716 ) ) ;
#18597 = VERTEX_POINT ( 'NONE', #1431 ) ;
#18598 = ORIENTED_EDGE ( 'NONE', *, *, #16889, .F. ) ;
#18599 = FACE_BOUND ( 'NONE', #23922, .T. ) ;
#18600 = VERTEX_POINT ( 'NONE', #28316 ) ;
#18601 = ORIENTED_EDGE ( 'NONE', *, *, #19901, .T. ) ;
#18602 = CARTESIAN_POINT ( 'NONE',  ( -442.0000000000000000, -105.0000000000000142, 155.0000000000000000 ) ) ;
#18603 = VECTOR ( 'NONE', #5756, 1000.000000000000000 ) ;
#18604 = AXIS2_PLACEMENT_3D ( 'NONE', #14055, #2659, #22063 ) ;
#18605=STYLED_ITEM('',(#35254),#11180);
#18606 = DIRECTION ( 'NONE',  ( 0.000000000000000000, 1.000000000000000000, 1.224646799147353207E-16 ) ) ;
#18607 = FACE_OUTER_BOUND ( 'NONE', #12855, .T. ) ;
#18608 = ORIENTED_EDGE ( 'NONE', *, *, #17216, .F. ) ;
#18609 = ORIENTED_EDGE ( 'NONE', *, *, #29387, .T. ) ;
#18610 = LINE ( 'NONE', #7908, #14000 ) ;
#18611 = CARTESIAN_POINT ( 'NONE',  ( -19.99999999999998934, -134.9999999999999716, 162.9999999999999716 ) ) ;
#18612 = FACE_OUTER_BOUND ( 'NONE', #13614, .T. ) ;
#18613 = EDGE_CURVE ( 'NONE', #21072, #26369, #28172, .T. ) ;
#18614 = CARTESIAN_POINT ( 'NONE',  ( 0.000000000000000000, 0.000000000000000000, 0.000000000000000000 ) ) ;
#18615 = DIRECTION ( 'NONE',  ( 0.000000000000000000, 1.000000000000000000, 0.000000000000000000 ) ) ;
#18616 = ORIENTED_EDGE ( 'NONE', *, *, #13711, .F. ) ;
#18617 = LINE ( 'NONE', #1868, #24176 ) ;
#18618 = EDGE_CURVE ( 'NONE', #25432, #30178, #6222, .T. ) ;
#18619 = CYLINDRICAL_SURFACE ( 'NONE', #18165, 4.000000000000003553 ) ;
#18620 = ORIENTED_EDGE ( 'NONE', *, *, #34751, .T. ) ;
#18621 = VECTOR ( 'NONE', #19913, 1000.000000000000000 ) ;
#18622 = PRODUCT_RELATED_PRODUCT_CATEGORY ( 'part', '', ( #985 ) ) ;
#18623 = DIRECTION ( 'NONE',  ( 1.000000000000000000, 0.000000000000000000, -1.232595164407831220E-32 ) ) ;
#18624 = CARTESIAN_POINT ( 'NONE',  ( -19.99999999999998934, -134.9999999999999716, 162.9999999999999716 ) ) ;
#18625 = DIRECTION ( 'NONE',  ( 0.000000000000000000, 1.310824597558155437E-49, 1.000000000000000000 ) ) ;
#18626 = ORIENTED_EDGE ( 'NONE', *, *, #16173, .F. ) ;
#18627 = LINE ( 'NONE', #10246, #9259 ) ;
#18628 = ORIENTED_EDGE ( 'NONE', *, *, #33674, .T. ) ;
#18629 = AXIS2_PLACEMENT_3D ( 'NONE', #21919, #7724, #5050 ) ;
#18630 = CARTESIAN_POINT ( 'NONE',  ( -442.0000000000000000, -105.0000000000000142, -77.99999999999997158 ) ) ;
#18631 = ORIENTED_EDGE ( 'NONE', *, *, #8888, .T. ) ;
#18633 = DIRECTION ( 'NONE',  ( 0.3193015301359802827, 0.9476531711828023452, 1.740810634186286145E-16 ) ) ;
#18632 = DIRECTION ( 'NONE',  ( 0.000000000000000000, 0.000000000000000000, 1.000000000000000000 ) ) ;
#18634 = CARTESIAN_POINT ( 'NONE',  ( 11.99999999999999645, 124.9999999999999716, 155.0000000000000000 ) ) ;
#18635 = AXIS2_PLACEMENT_3D ( 'NONE', #17880, #15198, #1656 ) ;
#18636 = VECTOR ( 'NONE', #21410, 1000.000000000000000 ) ;
#18637 = VERTEX_POINT ( 'NONE', #27953 ) ;
#18638 = PLANE ( 'NONE',  #20044 ) ;
#18639 = FACE_OUTER_BOUND ( 'NONE', #19230, .T. ) ;
#18640 = VERTEX_POINT ( 'NONE', #1260 ) ;
#18641 = AXIS2_PLACEMENT_3D ( 'NONE', #5970, #11166, #8829 ) ;
#18642 = DIRECTION ( 'NONE',  ( -7.893605728314051750E-14, 1.618803117314786530E-15, 1.000000000000000000 ) ) ;
#18643 = EDGE_LOOP ( 'NONE', ( #8762, #7011, #17349, #6269 ) ) ;
#18644 = CARTESIAN_POINT ( 'NONE',  ( -104.8247140911428374, 5.114965439436505612, 5.485173521317548762 ) ) ;
#18645 = VERTEX_POINT ( 'NONE', #33996 ) ;
#18646 = DIRECTION ( 'NONE',  ( 0.000000000000000000, -0.000000000000000000, 1.000000000000000000 ) ) ;
#18647 = CARTESIAN_POINT ( 'NONE',  ( -9.978866888775527855, 4.168562732279004202, -67.50000000000000000 ) ) ;
#18648 = AXIS2_PLACEMENT_3D ( 'NONE', #14495, #25856, #33342 ) ;
#18649 = CARTESIAN_POINT ( 'NONE',  ( -108.3784044661085773, -3.854070255762958919, -6.439229133474692723 ) ) ;
#18650 = CARTESIAN_POINT ( 'NONE',  ( 2.789999999999999147, -30.46391896562403190, -6.211548095912885259 ) ) ;
#18651 = VERTEX_POINT ( 'NONE', #12129 ) ;
#18652 = ORIENTED_EDGE ( 'NONE', *, *, #26906, .F. ) ;
#18653 = ORIENTED_EDGE ( 'NONE', *, *, #20098, .F. ) ;
#18654 = CARTESIAN_POINT ( 'NONE',  ( -28.23027531293552528, -17.65143121711728469, 20.00000000000000000 ) ) ;
#18655 = DIRECTION ( 'NONE',  ( 1.000000000000000000, 0.000000000000000000, -1.232595164407831220E-32 ) ) ;
#18656 = ADVANCED_FACE ( 'NONE', ( #22970 ), #33825, .T. ) ;
#18657 = DIRECTION ( 'NONE',  ( 1.000000000000000000, 0.000000000000000000, 0.000000000000000000 ) ) ;
#18658 = AXIS2_PLACEMENT_3D ( 'NONE', #18523, #29357, #4952 ) ;
#18659 = VECTOR ( 'NONE', #33091, 1000.000000000000000 ) ;
#18660 = DIRECTION ( 'NONE',  ( -0.000000000000000000, -0.000000000000000000, -1.000000000000000000 ) ) ;
#18661 = CARTESIAN_POINT ( 'NONE',  ( -418.0000000000000568, 105.0000000000000142, -105.9999999999999574 ) ) ;
#18662 = LINE ( 'NONE', #18313, #9527 ) ;
#18663 = CARTESIAN_POINT ( 'NONE',  ( -418.0000000000000000, -112.9999999999999858, 155.0000000000000000 ) ) ;
#18664 = ORIENTED_EDGE ( 'NONE', *, *, #2322, .T. ) ;
#18665 = EDGE_CURVE ( 'NONE', #29588, #22009, #23082, .T. ) ;
#18666 = FACE_OUTER_BOUND ( 'NONE', #5245, .T. ) ;
#18667 = EDGE_CURVE ( 'NONE', #33325, #29191, #15099, .T. ) ;
#18668 = CARTESIAN_POINT ( 'NONE',  ( 12.00000000000001066, -105.0000000000000142, -155.0000000000000000 ) ) ;
#18669 = VECTOR ( 'NONE', #780, 1000.000000000000000 ) ;
#18670 = CARTESIAN_POINT ( 'NONE',  ( 2.033589655658247342, 31.33480229261830630, -12.97668906163614189 ) ) ;
#18671 = ORIENTED_EDGE ( 'NONE', *, *, #34523, .T. ) ;
#18672 = ADVANCED_FACE ( 'NONE', ( #5094 ), #13883, .F. ) ;
#18673 = EDGE_CURVE ( 'NONE', #11377, #13666, #29844, .T. ) ;
#18674 = DIRECTION ( 'NONE',  ( -0.000000000000000000, -0.000000000000000000, -1.000000000000000000 ) ) ;
#18675 = ORIENTED_EDGE ( 'NONE', *, *, #34982, .F. ) ;
#18676 = CARTESIAN_POINT ( 'NONE',  ( -103.3412076437314369, 4.850327849261240054, -11.52145900171629833 ) ) ;
#18677 = EDGE_CURVE ( 'NONE', #4598, #20852, #34165, .T. ) ;
#18678 = FACE_OUTER_BOUND ( 'NONE', #32444, .T. ) ;
#18679 = CIRCLE ( 'NONE', #29484, 13.50000000000000178 ) ;
#18680 = ORIENTED_EDGE ( 'NONE', *, *, #12341, .F. ) ;
#18681 = DIRECTION ( 'NONE',  ( 0.000000000000000000, 0.000000000000000000, 1.000000000000000000 ) ) ;
#18682 = CARTESIAN_POINT ( 'NONE',  ( 29.63313772848250238, -13.45665341906703816, 68.31122994652405112 ) ) ;
#18683 = FACE_OUTER_BOUND ( 'NONE', #3655, .T. ) ;
#18684 = VERTEX_POINT ( 'NONE', #18654 ) ;
#18685 = AXIS2_PLACEMENT_3D ( 'NONE', #9261, #30799, #19952 ) ;
#18686 = B_SPLINE_CURVE_WITH_KNOTS ( 'NONE', 3,
 ( #2154, #15704, #13028, #34726 ),
 .UNSPECIFIED., .F., .F.,
 ( 4, 4 ),
 ( 2.436748180515292673E-07, 0.0006879797535939334791 ),
 .UNSPECIFIED. ) ;
#18687 = ORIENTED_EDGE ( 'NONE', *, *, #24378, .F. ) ;
#18688 = CARTESIAN_POINT ( 'NONE',  ( 756.8406557442693838, 1346.255075337097423, 1753.598338701303192 ) ) ;
#18689 = VECTOR ( 'NONE', #26507, 1000.000000000000114 ) ;
#18690 = DIRECTION ( 'NONE',  ( 1.000000000000000000, 0.000000000000000000, 0.000000000000000000 ) ) ;
#18691 = VERTEX_POINT ( 'NONE', #10975 ) ;
#18692 = CARTESIAN_POINT ( 'NONE',  ( 2.789999999999999147, -26.36977540154997257, -15.20550475489965514 ) ) ;
#18693 = DIRECTION ( 'NONE',  ( 0.000000000000000000, 0.000000000000000000, -1.000000000000000000 ) ) ;
#18694 = CARTESIAN_POINT ( 'NONE',  ( 104.2130153241097901, -5.687305096039679597, 4.889329717555864541 ) ) ;
#18695 = ITEM_DEFINED_TRANSFORMATION ( 'NONE', 'NONE', #17809,  #28566 ) ;
#18696 = ORIENTED_EDGE ( 'NONE', *, *, #34790, .T. ) ;
#18697 = CARTESIAN_POINT ( 'NONE',  ( 0.000000000000000000, 0.000000000000000000, 5.429999999999999716 ) ) ;
#18698 = AXIS2_PLACEMENT_3D ( 'NONE', #8701, #30424, #3715 ) ;
#18700 = FACE_OUTER_BOUND ( 'NONE', #18955, .T. ) ;
#18699 = DIRECTION ( 'NONE',  ( -0.000000000000000000, 0.5288966977476834419, -0.8486862100397269959 ) ) ;
#18701 = AXIS2_PLACEMENT_3D ( 'NONE', #10769, #26424, #13090 ) ;
#18702 = ORIENTED_EDGE ( 'NONE', *, *, #24584, .T. ) ;
#18703 = ORIENTED_EDGE ( 'NONE', *, *, #18537, .T. ) ;
#18704 = CARTESIAN_POINT ( 'NONE',  ( 0.000000000000000000, 2.281310696040539424E-14, -36.68877005347592757 ) ) ;
#18705 = EDGE_LOOP ( 'NONE', ( #27855, #33726, #15520, #21444, #13279, #18095 ) ) ;
#18706 = CARTESIAN_POINT ( 'NONE',  ( -35.00000000000000000, 16.36947364650383818, 36.69637551990492597 ) ) ;
#18707 = EDGE_CURVE ( 'NONE', #31215, #2635, #25316, .T. ) ;
#18708 = DIRECTION ( 'NONE',  ( 1.000000000000000000, 0.000000000000000000, 1.300283923313630633E-47 ) ) ;
#18709 = VERTEX_POINT ( 'NONE', #8301 ) ;
#18710 = DIRECTION ( 'NONE',  ( 0.000000000000000000, 1.000000000000000000, 1.224646799147353207E-16 ) ) ;
#18711 = EDGE_CURVE ( 'NONE', #13597, #25101, #5417, .T. ) ;
#18712 = EDGE_CURVE ( 'NONE', #34350, #726, #10455, .T. ) ;
#18713 = PRODUCT_DEFINITION_SHAPE ( 'NONE', 'NONE',  #35240 ) ;
#18714 = DIRECTION ( 'NONE',  ( 0.000000000000000000, 0.000000000000000000, -1.000000000000000000 ) ) ;
#18715 = ORIENTED_EDGE ( 'NONE', *, *, #13540, .T. ) ;
#18716 = CARTESIAN_POINT ( 'NONE',  ( 10.00000000000000000, 7.794228634059932048, -13.49999999999999822 ) ) ;
#18717 = DIRECTION ( 'NONE',  ( -1.000000000000000000, -0.000000000000000000, -0.000000000000000000 ) ) ;
#18718 = CYLINDRICAL_SURFACE ( 'NONE', #31459, 16.19999999999999574 ) ;
#18719 = MECHANICAL_DESIGN_GEOMETRIC_PRESENTATION_REPRESENTATION (  '', ( #17028 ), #4449 ) ;
#18720 = CARTESIAN_POINT ( 'NONE',  ( -500.0000000000000000, -113.0000000000000000, 155.0000000000000000 ) ) ;
#18721 = DIRECTION ( 'NONE',  ( 0.000000000000000000, 0.000000000000000000, 1.000000000000000000 ) ) ;
#18722 = DIRECTION ( 'NONE',  ( 0.000000000000000000, 0.000000000000000000, 1.000000000000000000 ) ) ;
#18723 = DIRECTION ( 'NONE',  ( 0.000000000000000000, 0.000000000000000000, -1.000000000000000000 ) ) ;
#18724 = EDGE_CURVE ( 'NONE', #6040, #32630, #119, .T. ) ;
#18725 = VECTOR ( 'NONE', #12231, 1000.000000000000000 ) ;
#18726 = ORIENTED_EDGE ( 'NONE', *, *, #1413, .T. ) ;
#18727 = FACE_OUTER_BOUND ( 'NONE', #7209, .T. ) ;
#18728 = DIRECTION ( 'NONE',  ( 0.000000000000000000, 0.000000000000000000, 1.000000000000000000 ) ) ;
#18729 = EDGE_LOOP ( 'NONE', ( #34404, #959, #20958, #22170, #21249, #13096, #4678, #12692, #3954, #5635 ) ) ;
#18731 = ORIENTED_EDGE ( 'NONE', *, *, #27878, .F. ) ;
#18730 = EDGE_CURVE ( 'NONE', #23016, #16381, #2024, .T. ) ;
#18732 = EDGE_CURVE ( 'NONE', #8317, #1101, #30019, .T. ) ;
#18733 = VECTOR ( 'NONE', #23956, 1000.000000000000114 ) ;
#18734 = ADVANCED_FACE ( 'NONE', ( #7103 ), #5613, .T. ) ;
#18735 = CARTESIAN_POINT ( 'NONE',  ( 0.000000000000000000, 27.98916443103598439, 15.38717335695048227 ) ) ;
#18736 = DIRECTION ( 'NONE',  ( -1.006271992937135158E-15, 4.669231749280401423E-14, 0.9999999999999998890 ) ) ;
#18737 = VERTEX_POINT ( 'NONE', #16511 ) ;
#18738 = DIRECTION ( 'NONE',  ( -1.000000000000000000, -0.000000000000000000, -0.000000000000000000 ) ) ;
#18739 = B_SPLINE_CURVE_WITH_KNOTS ( 'NONE', 3,
 ( #21983, #13979, #8617, #8092, #19496, #19151 ),
 .UNSPECIFIED., .F., .F.,
 ( 4, 2, 4 ),
 ( 1.978909662040563688E-07, 0.001873396183027086154, 0.003746594475087968324 ),
 .UNSPECIFIED. ) ;
#18740 = PRESENTATION_STYLE_ASSIGNMENT (( #13562 ) ) ;
#18741 = EDGE_CURVE ( 'NONE', #19872, #26754, #12260, .T. ) ;
#18742 = AXIS2_PLACEMENT_3D ( 'NONE', #3797, #1145, #3098 ) ;
#18743 = DIRECTION ( 'NONE',  ( 1.000000000000000000, 0.000000000000000000, -0.000000000000000000 ) ) ;
#18744 = ORIENTED_EDGE ( 'NONE', *, *, #3073, .F. ) ;
#18745 = ORIENTED_EDGE ( 'NONE', *, *, #17660, .F. ) ;
#18746 = CARTESIAN_POINT ( 'NONE',  ( -1.030735741678193262, 1.713938105891546382, 4.679999999999999716 ) ) ;
#18747 = B_SPLINE_CURVE_WITH_KNOTS ( 'NONE', 3,
 ( #10918, #24594, #27277, #7887, #2886, #32612 ),
 .UNSPECIFIED., .F., .F.,
 ( 4, 2, 4 ),
 ( 2.040444213406099367E-07, 0.001873402343194270235, 0.003746600641967199555 ),
 .UNSPECIFIED. ) ;
#18748 = DIRECTION ( 'NONE',  ( 0.000000000000000000, 1.836970198721029441E-16, -1.000000000000000000 ) ) ;
#18749 = DIRECTION ( 'NONE',  ( 0.000000000000000000, 0.000000000000000000, 1.000000000000000000 ) ) ;
#18750 = CARTESIAN_POINT ( 'NONE',  ( -442.0000000000000000, 113.0000000000000000, -155.0000000000000000 ) ) ;
#18751 = DIRECTION ( 'NONE',  ( -1.000000000000000000, 0.000000000000000000, 0.000000000000000000 ) ) ;
#18752 = VERTEX_POINT ( 'NONE', #15814 ) ;
#18753 = CARTESIAN_POINT ( 'NONE',  ( -14.84098889165989377, 28.96462362251111244, 68.31122994652405112 ) ) ;
#18754 = CARTESIAN_POINT ( 'NONE',  ( 0.02407890056441847060, -0.3931553186915530129, 31.08824725498900321 ) ) ;
#18755 = FACE_OUTER_BOUND ( 'NONE', #30064, .T. ) ;
#18756 = VECTOR ( 'NONE', #22685, 1000.000000000000000 ) ;
#18757 = EDGE_CURVE ( 'NONE', #28398, #21809, #28826, .T. ) ;
#18758 = APPLICATION_CONTEXT ( 'automotive_design' ) ;
#18759 = SURFACE_STYLE_USAGE ( .BOTH. , #29804 ) ;
#18760 = CARTESIAN_POINT ( 'NONE',  ( 110.7380848894536598, 7.027127293105233764E-16, 60.00000000000000000 ) ) ;
#18762 = DIRECTION ( 'NONE',  ( 1.000000000000000000, 0.000000000000000000, 0.000000000000000000 ) ) ;
#18761 = DIRECTION ( 'NONE',  ( 0.000000000000000000, 0.000000000000000000, 1.000000000000000000 ) ) ;
#18763 = CARTESIAN_POINT ( 'NONE',  ( 0.006871052634921217921, 28.06661910905163992, 12.85272128629691579 ) ) ;
#18764 = EDGE_LOOP ( 'NONE', ( #21823, #13367, #20102, #29497 ) ) ;
#18765 = CARTESIAN_POINT ( 'NONE',  ( 0.02407890056655564992, -30.46391896562411716, 6.211548095912460710 ) ) ;
#18767 = FACE_BOUND ( 'NONE', #11145, .T. ) ;
#18766 = DIRECTION ( 'NONE',  ( -1.000000000000000000, 0.000000000000000000, -0.000000000000000000 ) ) ;
#18768 = ORIENTED_EDGE ( 'NONE', *, *, #6369, .T. ) ;
#18769 = DIRECTION ( 'NONE',  ( 1.000000000000000000, -0.000000000000000000, -0.000000000000000000 ) ) ;
#18770 = EDGE_LOOP ( 'NONE', ( #10115, #10926, #2394, #11156 ) ) ;
#18771 = ADVANCED_FACE ( 'NONE', ( #2427 ), #26646, .T. ) ;
#18772 = EDGE_CURVE ( 'NONE', #32250, #16547, #7947, .T. ) ;
#18773 = ORIENTED_EDGE ( 'NONE', *, *, #6509, .F. ) ;
#18774 = FACE_OUTER_BOUND ( 'NONE', #29548, .T. ) ;
#18775 = ORIENTED_EDGE ( 'NONE', *, *, #34127, .T. ) ;
#18776 = ORIENTED_EDGE ( 'NONE', *, *, #32605, .F. ) ;
#18777 = CARTESIAN_POINT ( 'NONE',  ( 11.99999999999999645, 134.9999999999999432, -186.9999999999999716 ) ) ;
#18778 = LINE ( 'NONE', #20907, #30483 ) ;
#18779 = DIRECTION ( 'NONE',  ( 1.300283923313630633E-47, 0.000000000000000000, 1.000000000000000000 ) ) ;
#18780 = ORIENTED_EDGE ( 'NONE', *, *, #34607, .F. ) ;
#18781 = ORIENTED_EDGE ( 'NONE', *, *, #18971, .T. ) ;
#18782 = DIRECTION ( 'NONE',  ( 0.000000000000000000, 0.000000000000000000, 1.000000000000000000 ) ) ;
#18783 = EDGE_CURVE ( 'NONE', #32668, #31670, #19091, .T. ) ;
#18784 = DIRECTION ( 'NONE',  ( -1.000000000000000000, 0.000000000000000000, -5.546364386991661285E-52 ) ) ;
#18785 = CARTESIAN_POINT ( 'NONE',  ( 105.0000000000000000, 0.000000000000000000, 60.00000000000000000 ) ) ;
#18786 = ORIENTED_EDGE ( 'NONE', *, *, #19452, .T. ) ;
#18787 = CIRCLE ( 'NONE', #24441, 2.525000000000001243 ) ;
#18788 = CARTESIAN_POINT ( 'NONE',  ( 99.26191511054632599, 0.000000000000000000, 60.00000000000000000 ) ) ;
#18789 = CARTESIAN_POINT ( 'NONE',  ( 5.021133111224679091, 24.02303923978504940, -67.50000000000000000 ) ) ;
#18790 = VERTEX_POINT ( 'NONE', #19002 ) ;
#18791 = DIRECTION ( 'NONE',  ( 0.000000000000000000, 0.000000000000000000, -1.000000000000000000 ) ) ;
#18792 = CARTESIAN_POINT ( 'NONE',  ( 1.749999999999999778, 31.89769921723006263, -12.91988538846924151 ) ) ;
#18793 = DIRECTION ( 'NONE',  ( 0.000000000000000000, 0.000000000000000000, 1.000000000000000000 ) ) ;
#18794 = VERTEX_POINT ( 'NONE', #23962 ) ;
#18795 = CARTESIAN_POINT ( 'NONE',  ( 11.99999999999999645, 144.9999999999999716, -190.9999999999999432 ) ) ;
#18796 = VERTEX_POINT ( 'NONE', #26999 ) ;
#18797 = DIRECTION ( 'NONE',  ( 0.000000000000000000, 1.131431318426415506E-52, 1.000000000000000000 ) ) ;
#18798 = ORIENTED_EDGE ( 'NONE', *, *, #20238, .T. ) ;
#18799 = EDGE_CURVE ( 'NONE', #19057, #4259, #34844, .T. ) ;
#18801 = CARTESIAN_POINT ( 'NONE',  ( 0.7564103417896115289, 22.02455111472467308, -25.79115045147355190 ) ) ;
#18800 = CARTESIAN_POINT ( 'NONE',  ( 0.000000000000000000, 25.67797970382135375, 16.40405592474768426 ) ) ;
#18802 =( NAMED_UNIT ( * ) SI_UNIT ( $, .STERADIAN. ) SOLID_ANGLE_UNIT ( ) );
#18803 = VERTEX_POINT ( 'NONE', #24476 ) ;
#18804 = PLANE ( 'NONE',  #84 ) ;
#18805 = AXIS2_PLACEMENT_3D ( 'NONE', #31803, #15288, #15985 ) ;
#18806 = EDGE_CURVE ( 'NONE', #9216, #2852, #29876, .T. ) ;
#18807 = ORIENTED_EDGE ( 'NONE', *, *, #35049, .F. ) ;
#18808 = AXIS2_PLACEMENT_3D ( 'NONE', #26286, #34839, #29321 ) ;
#18809 = EDGE_CURVE ( 'NONE', #22576, #4259, #28048, .T. ) ;
#18810 = EDGE_CURVE ( 'NONE', #24390, #4119, #14187, .T. ) ;
#18811 = CARTESIAN_POINT ( 'NONE',  ( 756.6996743545911386, 1339.756604052074181, 1753.598338701303419 ) ) ;
#18812 = VERTEX_POINT ( 'NONE', #14005 ) ;
#18813 = DIRECTION ( 'NONE',  ( 1.000000000000000000, -0.000000000000000000, -0.000000000000000000 ) ) ;
#18814 = CARTESIAN_POINT ( 'NONE',  ( -102.6978521731631702, 4.579603235088349322, 5.941779048586182554 ) ) ;
#18815 = ORIENTED_EDGE ( 'NONE', *, *, #11983, .T. ) ;
#18816 = FACE_OUTER_BOUND ( 'NONE', #2545, .T. ) ;
#18817 = CARTESIAN_POINT ( 'NONE',  ( 0.8377008405913533018, -8.431745484732017459, -12.39578842395470559 ) ) ;
#18818 = CARTESIAN_POINT ( 'NONE',  ( -105.1762619145411293, -5.114955647091113278, -5.485182652933522363 ) ) ;
#18819 = AXIS2_PLACEMENT_3D ( 'NONE', #3792, #15194, #26202 ) ;
#18820 = FACE_OUTER_BOUND ( 'NONE', #24536, .T. ) ;
#18821 = ORIENTED_EDGE ( 'NONE', *, *, #15306, .T. ) ;
#18822 = ORIENTED_EDGE ( 'NONE', *, *, #31224, .T. ) ;
#18823 = AXIS2_PLACEMENT_3D ( 'NONE', #14209, #30390, #669 ) ;
#18824 = EDGE_LOOP ( 'NONE', ( #13525, #12578, #22767, #34481 ) ) ;
#18825 = DIRECTION ( 'NONE',  ( -1.000000000000000000, 0.000000000000000000, 0.000000000000000000 ) ) ;
#18826 = AXIS2_PLACEMENT_3D ( 'NONE', #20588, #7039, #23604 ) ;
#18827 = DIRECTION ( 'NONE',  ( 1.000000000000000000, 0.000000000000000000, -1.232595164407831220E-32 ) ) ;
#18828 = DIRECTION ( 'NONE',  ( 0.000000000000000000, 0.000000000000000000, 1.000000000000000000 ) ) ;
#18829 = DIRECTION ( 'NONE',  ( -1.000000000000000000, -0.000000000000000000, -0.000000000000000000 ) ) ;
#18830 = CARTESIAN_POINT ( 'NONE',  ( 2.789999999999999147, -13.59935610937951900, -28.90010281771846223 ) ) ;
#18831 = DIRECTION ( 'NONE',  ( 0.000000000000000000, 0.000000000000000000, 1.000000000000000000 ) ) ;
#18832 = DIRECTION ( 'NONE',  ( 1.000000000000000000, 0.000000000000000000, 5.546364386991661285E-52 ) ) ;
#18833 = ORIENTED_EDGE ( 'NONE', *, *, #24407, .F. ) ;
#18834 = CARTESIAN_POINT ( 'NONE',  ( 0.1835380226106660129, 19.62374805819769819, -25.61906966869672075 ) ) ;
#18835 = CARTESIAN_POINT ( 'NONE',  ( 2.765921099433441999, 4.286445725888479608, -30.79383171238939809 ) ) ;
#18836 = AXIS2_PLACEMENT_3D ( 'NONE', #13432, #18953, #5566 ) ;
#18837 = CARTESIAN_POINT ( 'NONE',  ( 2.604019705859993206, 29.54981872718654046, -12.99685134853830348 ) ) ;
#18838 = VERTEX_POINT ( 'NONE', #3480 ) ;
#18839 = CARTESIAN_POINT ( 'NONE',  ( -418.0000000000000000, 124.9999999999999574, -194.9999999999999716 ) ) ;
#18840 = ORIENTED_EDGE ( 'NONE', *, *, #14123, .F. ) ;
#18841 = LINE ( 'NONE', #321, #13209 ) ;
#18842 = CYLINDRICAL_SURFACE ( 'NONE', #22978, 7.999999999999979572 ) ;
#18844 = ORIENTED_EDGE ( 'NONE', *, *, #11535, .T. ) ;
#18843 = VECTOR ( 'NONE', #9100, 1000.000000000000000 ) ;
#18845 = AXIS2_PLACEMENT_3D ( 'NONE', #10293, #28638, #31305 ) ;
#18846 = EDGE_CURVE ( 'NONE', #1722, #22371, #11875, .T. ) ;
#18847 = DIRECTION ( 'NONE',  ( 1.000000000000000000, 0.000000000000000000, 0.000000000000000000 ) ) ;
#18848 = AXIS2_PLACEMENT_3D ( 'NONE', #12544, #17904, #22878 ) ;
#18849 = DIRECTION ( 'NONE',  ( 0.000000000000000000, 0.000000000000000000, -1.000000000000000000 ) ) ;
#18850 = CARTESIAN_POINT ( 'NONE',  ( -500.0000000000000000, 144.9999999999999716, 155.0000000000000000 ) ) ;
#18851 = AXIS2_PLACEMENT_3D ( 'NONE', #13369, #8536, #10699 ) ;
#18852 = EDGE_CURVE ( 'NONE', #29579, #16627, #6501, .T. ) ;
#18853 = ORIENTED_EDGE ( 'NONE', *, *, #22212, .T. ) ;
#18855 = ORIENTED_EDGE ( 'NONE', *, *, #9731, .F. ) ;
#18854 = EDGE_CURVE ( 'NONE', #23681, #14870, #11697, .T. ) ;
#18856 = DIRECTION ( 'NONE',  ( 2.157368784019057470E-14, 2.238938693723582162E-14, 0.9999999999999998890 ) ) ;
#18857 = CARTESIAN_POINT ( 'NONE',  ( -9.978866888775733912, -15.68591377522703745, -67.50000000000000000 ) ) ;
#18858 = EDGE_CURVE ( 'NONE', #14308, #6643, #19703, .T. ) ;
#18859 = ORIENTED_EDGE ( 'NONE', *, *, #32190, .F. ) ;
#18860 = AXIS2_PLACEMENT_3D ( 'NONE', #16911, #30942, #14414 ) ;
#18861 = CARTESIAN_POINT ( 'NONE',  ( -8.000000000000000000, 0.000000000000000000, -14.77499999999999858 ) ) ;
#18862 = DIRECTION ( 'NONE',  ( -1.000000000000000000, 0.000000000000000000, -5.546364386991661285E-52 ) ) ;
#18863 = CARTESIAN_POINT ( 'NONE',  ( -107.5860917622571407, -4.424982940199791770, 6.059505149883825936 ) ) ;
#18864 = EDGE_LOOP ( 'NONE', ( #28738, #28192, #16826, #12706 ) ) ;
#18865 = DIRECTION ( 'NONE',  ( 0.000000000000000000, 2.309213040847544338E-50, 1.000000000000000000 ) ) ;
#18866 = ADVANCED_FACE ( 'NONE', ( #33559 ), #3310, .F. ) ;
#18867 = EDGE_CURVE ( 'NONE', #16, #14561, #13826, .T. ) ;
#18869 = CARTESIAN_POINT ( 'NONE',  ( 8.485274312747504766, 31.41981051364775013, 68.31122994652405112 ) ) ;
#18868 = CARTESIAN_POINT ( 'NONE',  ( -12.00000000000001066, -64.99999999999997158, -175.0000000000000000 ) ) ;
#18871 = ORIENTED_EDGE ( 'NONE', *, *, #28415, .T. ) ;
#18870 = AXIS2_PLACEMENT_3D ( 'NONE', #2832, #3716, #884 ) ;
#18872 = ORIENTED_EDGE ( 'NONE', *, *, #30371, .T. ) ;
#18873 = CARTESIAN_POINT ( 'NONE',  ( 2.789999999999999147, -9.994970281559119485, -28.75192165143428724 ) ) ;
#18874 = CIRCLE ( 'NONE', #9207, 44.99999999999997158 ) ;
#18875 = ORIENTED_EDGE ( 'NONE', *, *, #31323, .F. ) ;
#18876 = AXIS2_PLACEMENT_3D ( 'NONE', #20011, #14326, #27005 ) ;
#18877 = CARTESIAN_POINT ( 'NONE',  ( 0.000000000000000000, 3.524919873834583163E-15, 68.31122994652405112 ) ) ;
#18878 = CARTESIAN_POINT ( 'NONE',  ( 0.000000000000000000, 33.69708579775584667, -36.68877005347592757 ) ) ;
#18879 = VERTEX_POINT ( 'NONE', #17404 ) ;
#18880 = ORIENTED_EDGE ( 'NONE', *, *, #26385, .F. ) ;
#18881 = CARTESIAN_POINT ( 'NONE',  ( -5.344999999999999751, 1.414467053015192657E-16, 3.930000000000000160 ) ) ;
#18882 = CARTESIAN_POINT ( 'NONE',  ( 1.205771365940061957, -15.58845726811992449, 7.826847450972439323E-16 ) ) ;
#18883 = VERTEX_POINT ( 'NONE', #2952 ) ;
#18884 = DIRECTION ( 'NONE',  ( 1.000000000000000000, 0.000000000000000000, 0.000000000000000000 ) ) ;
#18885 = DIRECTION ( 'NONE',  ( 0.000000000000000000, 1.310824597558155437E-49, 1.000000000000000000 ) ) ;
#18886 = CIRCLE ( 'NONE', #22201, 1.999999999999999112 ) ;
#18887 = FACE_OUTER_BOUND ( 'NONE', #13574, .T. ) ;
#18888 = DIRECTION ( 'NONE',  ( 0.000000000000000000, 1.836970198721029441E-16, -1.000000000000000000 ) ) ;
#18889 = DIRECTION ( 'NONE',  ( -3.040835319149746090E-31, -1.000000000000000000, 0.000000000000000000 ) ) ;
#18890 = B_SPLINE_CURVE_WITH_KNOTS ( 'NONE', 3,
 ( #20654, #31499, #15681, #31837, #7452, #15324 ),
 .UNSPECIFIED., .F., .F.,
 ( 4, 2, 4 ),
 ( 2.011514595390488525E-07, 0.001873399447076933835, 0.003746597742694328728 ),
 .UNSPECIFIED. ) ;
#18891 = DIRECTION ( 'NONE',  ( -1.000000000000000000, 0.000000000000000000, -0.000000000000000000 ) ) ;
#18892 = DIRECTION ( 'NONE',  ( -1.000000000000000000, 0.000000000000000000, 0.000000000000000000 ) ) ;
#18893 = ORIENTED_EDGE ( 'NONE', *, *, #26666, .F. ) ;
#18894 = VECTOR ( 'NONE', #5754, 1000.000000000000000 ) ;
#18895 = CARTESIAN_POINT ( 'NONE',  ( 5.390701026406702567, -37.47456861236020131, 68.31122994652405112 ) ) ;
#18896 = DIRECTION ( 'NONE',  ( 1.000000000000000000, 0.000000000000000000, 0.000000000000000000 ) ) ;
#18897 = VECTOR ( 'NONE', #34860, 1000.000000000000000 ) ;
#18898 = EDGE_CURVE ( 'NONE', #1364, #26980, #31786, .T. ) ;
#18899 = ORIENTED_EDGE ( 'NONE', *, *, #5283, .T. ) ;
#18900 = ORIENTED_EDGE ( 'NONE', *, *, #27703, .F. ) ;
#18901 = EDGE_CURVE ( 'NONE', #1194, #18566, #14546, .T. ) ;
#18902 = EDGE_CURVE ( 'NONE', #16548, #7253, #26684, .T. ) ;
#18903 = CARTESIAN_POINT ( 'NONE',  ( 104.9997419262085430, 5.748131698890998287, 4.817519326574049465 ) ) ;
#18904 = EDGE_CURVE ( 'NONE', #26182, #27028, #22362, .T. ) ;
#18905 = DIRECTION ( 'NONE',  ( -2.241610805150630393E-14, 5.303032354855167898E-14, 1.000000000000000000 ) ) ;
#18906 = EDGE_LOOP ( 'NONE', ( #32679, #29743, #23671, #8750, #3578, #3326 ) ) ;
#18907 = DIRECTION ( 'NONE',  ( 0.9635499925192230197, -0.2675283385292204774, -0.000000000000000000 ) ) ;
#18908 = FILL_AREA_STYLE_COLOUR ( '', #31789 ) ;
#18909 = CARTESIAN_POINT ( 'NONE',  ( -442.0000000000000000, -105.0000000000000142, 107.9999999999999858 ) ) ;
#18910 = ORIENTED_EDGE ( 'NONE', *, *, #15161, .T. ) ;
#18911 = EDGE_LOOP ( 'NONE', ( #15948, #12005, #23518, #20064 ) ) ;
#18912 = DIRECTION ( 'NONE',  ( -1.000000000000000000, -3.040835319149746090E-31, -1.232595164407830946E-32 ) ) ;
#18913 = DIRECTION ( 'NONE',  ( -1.000000000000000000, 8.881784197001254296E-16, 0.000000000000000000 ) ) ;
#18914 = CARTESIAN_POINT ( 'NONE',  ( -12.00000000000003908, -134.9999999999999716, -162.9999999999999432 ) ) ;
#18916 = EDGE_CURVE ( 'NONE', #16525, #22746, #15691, .T. ) ;
#18915 = LINE ( 'NONE', #398, #34713 ) ;
#18917 = DIRECTION ( 'NONE',  ( -1.000000000000000000, -0.000000000000000000, -0.000000000000000000 ) ) ;
#18918 = ORIENTED_EDGE ( 'NONE', *, *, #28306, .T. ) ;
#18919 = CARTESIAN_POINT ( 'NONE',  ( 22.89764159710611224, 13.56412600238610544, -87.50000000000000000 ) ) ;
#18920 = CARTESIAN_POINT ( 'NONE',  ( 2.261199740790834412, -32.14027485980090404, 9.048862969375786491 ) ) ;
#18921 = CARTESIAN_POINT ( 'NONE',  ( -361.0000000000000000, 124.9999999999999432, 164.9999999999999716 ) ) ;
#18922 = VECTOR ( 'NONE', #28294, 1000.000000000000000 ) ;
#18923 = AXIS2_PLACEMENT_3D ( 'NONE', #25704, #31229, #20547 ) ;
#18924 = VECTOR ( 'NONE', #3840, 1000.000000000000000 ) ;
#18925 = FACE_OUTER_BOUND ( 'NONE', #32515, .T. ) ;
#18926 = LINE ( 'NONE', #21588, #6434 ) ;
#18927 = DIRECTION ( 'NONE',  ( -0.000000000000000000, 1.836970198721029934E-16, -1.000000000000000000 ) ) ;
#18929 = FACE_OUTER_BOUND ( 'NONE', #14909, .T. ) ;
#18928 = DIRECTION ( 'NONE',  ( 0.8568571761675894960, 0.5155538571770215128, -0.000000000000000000 ) ) ;
#18930 = EDGE_CURVE ( 'NONE', #28532, #29779, #22011, .T. ) ;
#18931 = ADVANCED_FACE ( 'NONE', ( #30188 ), #6144, .T. ) ;
#18932 = CARTESIAN_POINT ( 'NONE',  ( 2.789999999999999147, 30.93646776788807173, -7.943134866715984899 ) ) ;
#18933 = ORIENTED_EDGE ( 'NONE', *, *, #9826, .T. ) ;
#18934 = FACE_OUTER_BOUND ( 'NONE', #33428, .T. ) ;
#18936 = CARTESIAN_POINT ( 'NONE',  ( 110.4182009727613547, -1.926730348087509981, -7.257477599627513598 ) ) ;
#18935 = DIRECTION ( 'NONE',  ( 0.000000000000000000, 0.000000000000000000, -1.000000000000000000 ) ) ;
#18937 = VERTEX_POINT ( 'NONE', #3133 ) ;
#18938 = LINE ( 'NONE', #32093, #2964 ) ;
#18939 = ORIENTED_EDGE ( 'NONE', *, *, #30452, .F. ) ;
#18940 =( GEOMETRIC_REPRESENTATION_CONTEXT ( 3 ) GLOBAL_UNCERTAINTY_ASSIGNED_CONTEXT ( ( #1418 ) ) GLOBAL_UNIT_ASSIGNED_CONTEXT ( ( #3776, #9816, #9994 ) ) REPRESENTATION_CONTEXT ( 'NONE', 'WORKASPACE' ) );
#18941 = AXIS2_PLACEMENT_3D ( 'NONE', #19541, #495, #24860 ) ;
#18942 = AXIS2_PLACEMENT_3D ( 'NONE', #18199, #26175, #3937 ) ;
#18943 = ADVANCED_FACE ( 'NONE', ( #24843 ), #476, .T. ) ;
#18944 = EDGE_CURVE ( 'NONE', #28271, #31232, #6845, .T. ) ;
#18945 = CIRCLE ( 'NONE', #6981, 4.750000000000004441 ) ;
#18946 = ORIENTED_EDGE ( 'NONE', *, *, #3107, .T. ) ;
#18947 = DIRECTION ( 'NONE',  ( 0.000000000000000000, 1.000000000000000000, -5.053935297177146739E-49 ) ) ;
#18948 = ORIENTED_EDGE ( 'NONE', *, *, #33578, .T. ) ;
#18949 = ORIENTED_EDGE ( 'NONE', *, *, #22982, .T. ) ;
#18950 = DIRECTION ( 'NONE',  ( 1.000000000000000000, 0.000000000000000000, 0.000000000000000000 ) ) ;
#18951 = EDGE_CURVE ( 'NONE', #29194, #2425, #1528, .T. ) ;
#18952 = DIRECTION ( 'NONE',  ( 0.000000000000000000, 1.000000000000000000, -3.374343856708137958E-53 ) ) ;
#18953 = DIRECTION ( 'NONE',  ( -1.000000000000000000, 0.000000000000000000, 0.000000000000000000 ) ) ;
#18954 = EDGE_LOOP ( 'NONE', ( #27284, #14043, #34998, #8566 ) ) ;
#18955 = EDGE_LOOP ( 'NONE', ( #29836, #20785, #23954, #12504, #17248, #11468 ) ) ;
#18956 = CARTESIAN_POINT ( 'NONE',  ( -20.00000000000001776, -113.0000000000000000, 162.9999999999999716 ) ) ;
#18957 =( LENGTH_UNIT ( ) NAMED_UNIT ( * ) SI_UNIT ( .MILLI., .METRE. ) );
#18958 = CARTESIAN_POINT ( 'NONE',  ( 102.4443407045872902, -5.151199242560473124, -11.39037137834242586 ) ) ;
#18959 = CARTESIAN_POINT ( 'NONE',  ( -25.63124651156763889, 20.05601094782694105, 68.31122994652405112 ) ) ;
#18960 = ORIENTED_EDGE ( 'NONE', *, *, #2321, .T. ) ;
#18961 = CARTESIAN_POINT ( 'NONE',  ( -143.0000000000000568, -97.49999999999998579, 51.88904920397793319 ) ) ;
#18962 = FACE_OUTER_BOUND ( 'NONE', #11378, .T. ) ;
#18963 = EDGE_LOOP ( 'NONE', ( #11358, #31098, #1470, #5306 ) ) ;
#18964 = CARTESIAN_POINT ( 'NONE',  ( -35.00000000000000000, -46.95407462254104303, -36.69637551990492597 ) ) ;
#18965 = CARTESIAN_POINT ( 'NONE',  ( 10.17231796313411429, 17.63622956525712127, -77.50000000000000000 ) ) ;
#18966 = LINE ( 'NONE', #16840, #33713 ) ;
#18967 = EDGE_CURVE ( 'NONE', #15089, #3779, #34441, .T. ) ;
#18968 = AXIS2_PLACEMENT_3D ( 'NONE', #145, #3339, #17070 ) ;
#18969 = DIRECTION ( 'NONE',  ( 0.000000000000000000, 0.000000000000000000, -1.000000000000000000 ) ) ;
#18970 = EDGE_LOOP ( 'NONE', ( #17666, #585, #15557, #8488 ) ) ;
#18971 = EDGE_CURVE ( 'NONE', #6373, #23746, #34995, .T. ) ;
#18972 = AXIS2_PLACEMENT_3D ( 'NONE', #26791, #26093, #1711 ) ;
#18973 = VECTOR ( 'NONE', #30787, 1000.000000000000000 ) ;
#18974 = DIRECTION ( 'NONE',  ( -0.6051742151937647973, -0.7960930657056438653, 0.000000000000000000 ) ) ;
#18975 = EDGE_LOOP ( 'NONE', ( #19189, #8113, #5218, #26000 ) ) ;
#18977 = DIRECTION ( 'NONE',  ( 0.000000000000000000, 1.131431318426415506E-52, 1.000000000000000000 ) ) ;
#18976 = DIRECTION ( 'NONE',  ( 1.000000000000000000, 0.000000000000000000, 0.000000000000000000 ) ) ;
#18978 = CARTESIAN_POINT ( 'NONE',  ( -15.99999999999998579, 112.9999999999999574, 155.0000000000000000 ) ) ;
#18979 = ADVANCED_FACE ( 'NONE', ( #4177 ), #10057, .T. ) ;
#18980 = EDGE_CURVE ( 'NONE', #7133, #11066, #23406, .T. ) ;
#18981 = VERTEX_POINT ( 'NONE', #25907 ) ;
#18982 = CARTESIAN_POINT ( 'NONE',  ( 2.783128920429635667, -21.36428053051117715, 22.28216981039778233 ) ) ;
#18983 = EDGE_CURVE ( 'NONE', #33898, #11797, #7364, .T. ) ;
#18984 = DIRECTION ( 'NONE',  ( 0.000000000000000000, 1.000000000000000000, -6.123233995736766036E-17 ) ) ;
#18985 = VERTEX_POINT ( 'NONE', #3998 ) ;
#18986 = VECTOR ( 'NONE', #30753, 1000.000000000000000 ) ;
#18987 = ORIENTED_EDGE ( 'NONE', *, *, #32856, .F. ) ;
#18988 = DIRECTION ( 'NONE',  ( -0.000000000000000000, -1.000000000000000000, -0.000000000000000000 ) ) ;
#18989 = CARTESIAN_POINT ( 'NONE',  ( -108.3728249738879583, 3.859208454723701998, 6.436243333213716333 ) ) ;
#18990 = EDGE_LOOP ( 'NONE', ( #14186, #7912, #15931 ) ) ;
#18991 = ORIENTED_EDGE ( 'NONE', *, *, #12304, .T. ) ;
#18992 = DIRECTION ( 'NONE',  ( -0.000000000000000000, 1.000000000000000000, -0.000000000000000000 ) ) ;
#18993 = PRODUCT_DEFINITION_FORMATION_WITH_SPECIFIED_SOURCE ( 'ANY', '', #5768, .NOT_KNOWN. ) ;
#18994 = CARTESIAN_POINT ( 'NONE',  ( 3.754050022231059103E-15, -11.02739026146942969, -7.899999792244740249 ) ) ;
#18995 = AXIS2_PLACEMENT_3D ( 'NONE', #18590, #18408, #29429 ) ;
#18996 = CARTESIAN_POINT ( 'NONE',  ( 2.809983787309732928E-16, -17.84464379609624984, -24.93395722650028290 ) ) ;
#18997 = CARTESIAN_POINT ( 'NONE',  ( -355.0000000000000000, -119.0000000000000000, 113.9999999999999858 ) ) ;
#18998 = VERTEX_POINT ( 'NONE', #23584 ) ;
#18999 = VERTEX_POINT ( 'NONE', #20911 ) ;
#19000 = VECTOR ( 'NONE', #27018, 1000.000000000000000 ) ;
#19001 = PRODUCT_DEFINITION_SHAPE ( 'NONE', 'NONE',  #35202 ) ;
#19002 = CARTESIAN_POINT ( 'NONE',  ( 15.99999999999998579, 144.9999999999999716, -162.9999999999999432 ) ) ;
#19003 = DIRECTION ( 'NONE',  ( 0.3193015301359796165, -0.9476531711828025673, 0.000000000000000000 ) ) ;
#19004 = EDGE_CURVE ( 'NONE', #26512, #25584, #20231, .T. ) ;
#19005 = CARTESIAN_POINT ( 'NONE',  ( 15.99999999999998579, -115.0000000000000000, 155.0000000000000000 ) ) ;
#19006 = CARTESIAN_POINT ( 'NONE',  ( -3.250000000000000000, 5.404196845913421754, 5.429999999999999716 ) ) ;
#19007 = LINE ( 'NONE', #34849, #30413 ) ;
#19008 = CARTESIAN_POINT ( 'NONE',  ( -39.79673454871243621, -35.10674429148210862, 45.90417104242168733 ) ) ;
#19010 = LINE ( 'NONE', #17538, #14076 ) ;
#19009 =( REPRESENTATION_RELATIONSHIP ('NONE','NONE', #23037, #28231 ) REPRESENTATION_RELATIONSHIP_WITH_TRANSFORMATION ( #4469 )SHAPE_REPRESENTATION_RELATIONSHIP( ) );
#19011 = CARTESIAN_POINT ( 'NONE',  ( -25.63124651156763179, 20.05601094782693394, 68.31122994652405112 ) ) ;
#19012 = ORIENTED_EDGE ( 'NONE', *, *, #12983, .F. ) ;
#19013 = EDGE_CURVE ( 'NONE', #18879, #32399, #3828, .T. ) ;
#19014 = CARTESIAN_POINT ( 'NONE',  ( -12.00000000000001066, 144.9999999999999716, -154.9999999999999716 ) ) ;
#19015 = CARTESIAN_POINT ( 'NONE',  ( -12.00000000000001066, -28.99999999999999645, 154.9999999999999716 ) ) ;
#19016 = EDGE_CURVE ( 'NONE', #34043, #19094, #29649, .T. ) ;
#19017 = DIRECTION ( 'NONE',  ( -1.292961597001347186E-16, 0.000000000000000000, 1.000000000000000000 ) ) ;
#19018 = ORIENTED_EDGE ( 'NONE', *, *, #30814, .F. ) ;
#19019 = EDGE_CURVE ( 'NONE', #13074, #1683, #25548, .T. ) ;
#19020 = VECTOR ( 'NONE', #28956, 1000.000000000000000 ) ;
#19021 = CYLINDRICAL_SURFACE ( 'NONE', #21770, 7.999999999999979572 ) ;
#19022 = VERTEX_POINT ( 'NONE', #33739 ) ;
#19023 = CIRCLE ( 'NONE', #8761, 2.000000000000001776 ) ;
#19024 = CARTESIAN_POINT ( 'NONE',  ( -101.8755507196252950, 4.063381404898921190, -11.82275161328742641 ) ) ;
#19025 = DIRECTION ( 'NONE',  ( 0.000000000000000000, 1.000000000000000000, 1.836970198721029688E-16 ) ) ;
#19026 = EDGE_CURVE ( 'NONE', #27727, #28601, #2082, .T. ) ;
#19027 = VECTOR ( 'NONE', #3973, 1000.000000000000000 ) ;
#19028 = EDGE_LOOP ( 'NONE', ( #10583, #22101, #26838, #24604, #260, #216, #12546, #13554 ) ) ;
#19029 = VECTOR ( 'NONE', #34242, 1000.000000000000000 ) ;
#19030 = CARTESIAN_POINT ( 'NONE',  ( -418.0000000000000000, -105.0000000000000142, -77.99999999999997158 ) ) ;
#19031 = DIRECTION ( 'NONE',  ( -5.546364386991661285E-52, 0.000000000000000000, -1.000000000000000000 ) ) ;
#19032 = CARTESIAN_POINT ( 'NONE',  ( 2.765921099433442887, -26.45933846664205902, 16.32596387352436551 ) ) ;
#19033 = VECTOR ( 'NONE', #25274, 1000.000000000000000 ) ;
#19034 = VERTEX_POINT ( 'NONE', #31246 ) ;
#19035 = ORIENTED_EDGE ( 'NONE', *, *, #31496, .T. ) ;
#19036 = DIRECTION ( 'NONE',  ( -7.836557490484587452E-14, 8.342254427821387269E-15, 0.9999999999999998890 ) ) ;
#19037 = CARTESIAN_POINT ( 'NONE',  ( -347.0000000000000000, -125.0000000000000284, 181.0000000000000000 ) ) ;
#19038 = VERTEX_POINT ( 'NONE', #31589 ) ;
#19039 = CARTESIAN_POINT ( 'NONE',  ( 0.5248942303300246914, 26.54141775410178283, -20.24262527922973831 ) ) ;
#19040 = CARTESIAN_POINT ( 'NONE',  ( -15.99999999999998579, -137.0000000000000000, 174.9999999999999432 ) ) ;
#19041 = CIRCLE ( 'NONE', #16195, 34.41491905851385269 ) ;
#19042 = DIRECTION ( 'NONE',  ( 1.000000000000000000, 0.000000000000000000, 0.000000000000000000 ) ) ;
#19043 = CARTESIAN_POINT ( 'NONE',  ( -100.2299249775011418, -1.854090048725077100, 7.268955362025008249 ) ) ;
#19044 = ITEM_DEFINED_TRANSFORMATION ( 'NONE', 'NONE', #9825,  #28566 ) ;
#19045 = ORIENTED_EDGE ( 'NONE', *, *, #15735, .T. ) ;
#19046 = EDGE_LOOP ( 'NONE', ( #928, #15093, #15346, #19426, #20909, #10819, #31014, #27876 ) ) ;
#19047 = DIRECTION ( 'NONE',  ( 1.000000000000000000, 0.000000000000000000, 0.000000000000000000 ) ) ;
#19048 = VECTOR ( 'NONE', #15457, 1000.000000000000000 ) ;
#19049 = ORIENTED_EDGE ( 'NONE', *, *, #762, .T. ) ;
#19051 = CARTESIAN_POINT ( 'NONE',  ( -410.0000000000000568, -105.0000000000000142, -174.9999999999999716 ) ) ;
#19050 = DIRECTION ( 'NONE',  ( 0.000000000000000000, 0.4817536741017036106, 0.8763066800438700232 ) ) ;
#19052 = VECTOR ( 'NONE', #1968, 1000.000000000000000 ) ;
#19053 = ORIENTED_EDGE ( 'NONE', *, *, #16300, .T. ) ;
#19054 = EDGE_LOOP ( 'NONE', ( #24677, #19739, #6791, #4951, #9049 ) ) ;
#19055 = VECTOR ( 'NONE', #27365, 1000.000000000000000 ) ;
#19056 = DIRECTION ( 'NONE',  ( -1.000000000000000000, -0.000000000000000000, 0.000000000000000000 ) ) ;
#19057 = VERTEX_POINT ( 'NONE', #12394 ) ;
#19058 = ADVANCED_FACE ( 'NONE', ( #23246 ), #28581, .F. ) ;
#19059 = DIRECTION ( 'NONE',  ( 1.000000000000000000, 0.000000000000000000, 0.000000000000000000 ) ) ;
#19060 = DIRECTION ( 'NONE',  ( 0.000000000000000000, 5.145227585319922065E-49, 1.000000000000000000 ) ) ;
#19061 = ORIENTED_EDGE ( 'NONE', *, *, #24304, .F. ) ;
#19062 = ORIENTED_EDGE ( 'NONE', *, *, #28567, .F. ) ;
#19063 = DIRECTION ( 'NONE',  ( 0.000000000000000000, -1.000000000000000000, -5.053935297177146739E-49 ) ) ;
#19064 = EDGE_CURVE ( 'NONE', #25899, #1486, #31082, .T. ) ;
#19065 = CARTESIAN_POINT ( 'NONE',  ( -21.67835495107042476, 31.04982069277124879, -36.68877005347593467 ) ) ;
#19066 = VERTEX_POINT ( 'NONE', #4513 ) ;
#19067 = EDGE_CURVE ( 'NONE', #24998, #916, #33277, .T. ) ;
#19068 = LINE ( 'NONE', #16400, #25443 ) ;
#19069 = LINE ( 'NONE', #29559, #3598 ) ;
#19070 = DIRECTION ( 'NONE',  ( 0.000000000000000000, 0.1253332335643122519, -0.9921147013144767657 ) ) ;
#19071 = AXIS2_PLACEMENT_3D ( 'NONE', #17486, #33297, #30634 ) ;
#19072 = AXIS2_PLACEMENT_3D ( 'NONE', #22021, #8658, #19536 ) ;
#19073 = CARTESIAN_POINT ( 'NONE',  ( 0.000000000000000000, 49.99999999999999289, 0.000000000000000000 ) ) ;
#19074 = DIRECTION ( 'NONE',  ( 0.000000000000000000, 1.310824597558155437E-49, 1.000000000000000000 ) ) ;
#19075 = DIRECTION ( 'NONE',  ( 0.000000000000000000, 0.000000000000000000, 1.000000000000000000 ) ) ;
#19076 = CIRCLE ( 'NONE', #23606, 7.999999999999979572 ) ;
#19077 = EDGE_CURVE ( 'NONE', #32120, #33261, #28407, .T. ) ;
#19078 = CARTESIAN_POINT ( 'NONE',  ( -418.0000000000000000, 104.9999999999999858, -162.9999999999999716 ) ) ;
#19079 = VERTEX_POINT ( 'NONE', #12227 ) ;
#19081 = AXIS2_PLACEMENT_3D ( 'NONE', #28776, #4716, #26451 ) ;
#19080 = DIRECTION ( 'NONE',  ( -0.000000000000000000, 1.000000000000000000, -0.000000000000000000 ) ) ;
#19082 = CARTESIAN_POINT ( 'NONE',  ( 824.9889302421501043, 1274.265674307988093, 1753.598338701302964 ) ) ;
#19083 = AXIS2_PLACEMENT_3D ( 'NONE', #10046, #15937, #12729 ) ;
#19084 = VERTEX_POINT ( 'NONE', #29455 ) ;
#19085 = ORIENTED_EDGE ( 'NONE', *, *, #32094, .T. ) ;
#19086 = DIRECTION ( 'NONE',  ( 0.000000000000000000, -1.000000000000000000, -5.053935297177146739E-49 ) ) ;
#19087 = APPLICATION_PROTOCOL_DEFINITION ( 'draft international standard', 'automotive_design', 1998, #9642 ) ;
#19088 = VERTEX_POINT ( 'NONE', #7723 ) ;
#19089 = CARTESIAN_POINT ( 'NONE',  ( 2.765921099433442443, 20.99477179376858871, -22.93149026599722617 ) ) ;
#19090 = CONTEXT_DEPENDENT_SHAPE_REPRESENTATION ( #24425, #13310 ) ;
#19091 = CIRCLE ( 'NONE', #12839, 7.999999999999979572 ) ;
#19092 = DIRECTION ( 'NONE',  ( 1.000000000000000000, 0.000000000000000000, 0.000000000000000000 ) ) ;
#19093 = ORIENTED_EDGE ( 'NONE', *, *, #16852, .T. ) ;
#19094 = VERTEX_POINT ( 'NONE', #32111 ) ;
#19095 = DIRECTION ( 'NONE',  ( -1.000000000000000000, -0.000000000000000000, -0.000000000000000000 ) ) ;
#19096 = CYLINDRICAL_SURFACE ( 'NONE', #13549, 7.999999999999979572 ) ;
#19097 = AXIS2_PLACEMENT_3D ( 'NONE', #12359, #9668, #30859 ) ;
#19098 = EDGE_CURVE ( 'NONE', #2489, #6590, #26596, .T. ) ;
#19099 = DIRECTION ( 'NONE',  ( 0.000000000000000000, 0.000000000000000000, -1.000000000000000000 ) ) ;
#19100 = DIRECTION ( 'NONE',  ( 0.000000000000000000, 0.000000000000000000, 1.000000000000000000 ) ) ;
#19101 = CARTESIAN_POINT ( 'NONE',  ( 29.44023756548695658, 13.87360028845404614, 68.31122994652405112 ) ) ;
#19102 = ORIENTED_EDGE ( 'NONE', *, *, #25952, .F. ) ;
#19103 = CARTESIAN_POINT ( 'NONE',  ( -499.9999999999999432, -113.0000000000000000, -155.0000000000000000 ) ) ;
#19104 = FACE_OUTER_BOUND ( 'NONE', #15527, .T. ) ;
#19105 = CARTESIAN_POINT ( 'NONE',  ( -418.0000000000000000, -141.0000000000000000, -155.0000000000000000 ) ) ;
#19106 = EDGE_CURVE ( 'NONE', #14881, #12542, #25344, .T. ) ;
#19107 = VECTOR ( 'NONE', #1280, 1000.000000000000000 ) ;
#19108 = CARTESIAN_POINT ( 'NONE',  ( -418.0000000000000000, 105.0000000000000142, 190.9999999999999716 ) ) ;
#19109 = LINE ( 'NONE', #2877, #26331 ) ;
#19110 = EDGE_CURVE ( 'NONE', #32967, #1944, #18610, .T. ) ;
#19111 = DIRECTION ( 'NONE',  ( 0.000000000000000000, -1.000000000000000000, 0.000000000000000000 ) ) ;
#19113 = DIRECTION ( 'NONE',  ( 0.7621620551276367950, 0.6473862847818272481, -0.000000000000000000 ) ) ;
#19112 = FACE_OUTER_BOUND ( 'NONE', #6297, .T. ) ;
#19114 = EDGE_CURVE ( 'NONE', #13159, #12420, #23684, .T. ) ;
#19115 = EDGE_CURVE ( 'NONE', #16741, #5474, #15128, .T. ) ;
#19116 = CARTESIAN_POINT ( 'NONE',  ( -20.02113311122478123, 18.16264470403145381, -87.50000000000000000 ) ) ;
#19117 = ORIENTED_EDGE ( 'NONE', *, *, #9292, .F. ) ;
#19118 = CARTESIAN_POINT ( 'NONE',  ( -143.0000000000000568, 85.49999999999998579, 65.00000000000000000 ) ) ;
#19120 = CARTESIAN_POINT ( 'NONE',  ( -499.9999999999999432, 144.9999999999999716, -162.9999999999999716 ) ) ;
#19119 = CARTESIAN_POINT ( 'NONE',  ( -130.6469666100234406, 6.000000000000000000, -62.49999999999999289 ) ) ;
#19121 = EDGE_CURVE ( 'NONE', #28732, #34550, #12919, .T. ) ;
#19122 = AXIS2_PLACEMENT_3D ( 'NONE', #18956, #32631, #74 ) ;
#19123 = VERTEX_POINT ( 'NONE', #13264 ) ;
#19124 = VECTOR ( 'NONE', #27969, 1000.000000000000000 ) ;
#19125 = EDGE_LOOP ( 'NONE', ( #1852, #24705, #6627, #20518 ) ) ;
#19126 = EDGE_LOOP ( 'NONE', ( #33333, #3756, #16098, #14171 ) ) ;
#19127 = FACE_BOUND ( 'NONE', #27460, .T. ) ;
#19128 = ORIENTED_EDGE ( 'NONE', *, *, #10044, .F. ) ;
#19129 = ORIENTED_EDGE ( 'NONE', *, *, #9727, .T. ) ;
#19130 = DIRECTION ( 'NONE',  ( -0.7960930657056438653, 0.6051742151937650194, 1.111686998345334199E-16 ) ) ;
#19131 = VECTOR ( 'NONE', #13108, 1000.000000000000000 ) ;
#19132 = CONTEXT_DEPENDENT_SHAPE_REPRESENTATION ( #32599, #9478 ) ;
#19133 = DIRECTION ( 'NONE',  ( -3.040835319149746090E-31, -1.000000000000000000, 3.748118910144520367E-63 ) ) ;
#19134 = DIRECTION ( 'NONE',  ( -1.000000000000000000, 0.000000000000000000, 0.000000000000000000 ) ) ;
#19135 = AXIS2_PLACEMENT_3D ( 'NONE', #34437, #10398, #32106 ) ;
#19136 = EDGE_LOOP ( 'NONE', ( #20003, #6622, #9796, #30877 ) ) ;
#19137 = EDGE_LOOP ( 'NONE', ( #9567, #23031, #13634, #24613 ) ) ;
#19138 = DIRECTION ( 'NONE',  ( -1.000000000000000000, 0.000000000000000000, 0.000000000000000000 ) ) ;
#19139 = DIRECTION ( 'NONE',  ( -1.000000000000000000, -0.000000000000000000, 0.000000000000000000 ) ) ;
#19140 = CARTESIAN_POINT ( 'NONE',  ( 110.7380848894536598, -0.3789272201562005615, -12.50000000000000533 ) ) ;
#19141 = PLANE ( 'NONE',  #30167 ) ;
#19142 = VERTEX_POINT ( 'NONE', #27123 ) ;
#19143 = AXIS2_PLACEMENT_3D ( 'NONE', #30278, #738, #11074 ) ;
#19144 = CARTESIAN_POINT ( 'NONE',  ( -12.00000000000001066, -28.99999999999999645, -154.9999999999999716 ) ) ;
#19145 = DIRECTION ( 'NONE',  ( 1.000000000000000000, 0.000000000000000000, -0.000000000000000000 ) ) ;
#19146 = VERTEX_POINT ( 'NONE', #32453 ) ;
#19147 = AXIS2_PLACEMENT_3D ( 'NONE', #26607, #2226, #18791 ) ;
#19148 = FACE_OUTER_BOUND ( 'NONE', #2446, .T. ) ;
#19149 = DIRECTION ( 'NONE',  ( 0.000000000000000000, -0.5288966977476834419, -0.8486862100397269959 ) ) ;
#19150 = DIRECTION ( 'NONE',  ( 0.000000000000000000, 2.465190328815661892E-32, 1.000000000000000000 ) ) ;
#19151 = CARTESIAN_POINT ( 'NONE',  ( 1.749999999999999778, 6.714005886385429278, -33.75364837705166110 ) ) ;
#19152 = EDGE_LOOP ( 'NONE', ( #24770, #31285, #31135, #4765 ) ) ;
#19153 = EDGE_CURVE ( 'NONE', #16922, #13770, #35015, .T. ) ;
#19154 = EDGE_CURVE ( 'NONE', #32312, #9482, #359, .T. ) ;
#19155 = FACE_OUTER_BOUND ( 'NONE', #4650, .T. ) ;
#19156 = ORIENTED_EDGE ( 'NONE', *, *, #21975, .F. ) ;
#19158 = SURFACE_STYLE_USAGE ( .BOTH. , #32653 ) ;
#19157 = CARTESIAN_POINT ( 'NONE',  ( 0.02407890056655738464, 26.03801215795517621, 16.98986790278620873 ) ) ;
#19159 = AXIS2_PLACEMENT_3D ( 'NONE', #17199, #17026, #8989 ) ;
#19160 = ORIENTED_EDGE ( 'NONE', *, *, #16292, .T. ) ;
#19161 = CARTESIAN_POINT ( 'NONE',  ( -5.021133111224679091, 26.05646109878476224, -67.50000000000000000 ) ) ;
#19162 = CARTESIAN_POINT ( 'NONE',  ( 2.765921099433443331, 26.03801215795517621, 16.98986790278620873 ) ) ;
#19163 = CIRCLE ( 'NONE', #35064, 3.999999999999976019 ) ;
#19164 = ORIENTED_EDGE ( 'NONE', *, *, #19823, .F. ) ;
#19165 = EDGE_CURVE ( 'NONE', #693, #23520, #24435, .T. ) ;
#19166 = AXIS2_PLACEMENT_3D ( 'NONE', #22411, #13877, #30421 ) ;
#19167 = ORIENTED_EDGE ( 'NONE', *, *, #28406, .T. ) ;
#19168 = CARTESIAN_POINT ( 'NONE',  ( -5.021133111225092982, -15.68591377522703745, -67.50000000000000000 ) ) ;
#19169 = CARTESIAN_POINT ( 'NONE',  ( -104.3031396033928218, 5.070301591678567199, 5.526538532257565528 ) ) ;
#19170 = ORIENTED_EDGE ( 'NONE', *, *, #17357, .F. ) ;
#19171 = VERTEX_POINT ( 'NONE', #13436 ) ;
#19172 = LINE ( 'NONE', #25364, #18429 ) ;
#19173 = ADVANCED_FACE ( 'NONE', ( #29797 ), #29277, .T. ) ;
#19174 = EDGE_CURVE ( 'NONE', #15297, #1165, #24269, .T. ) ;
#19175 = CARTESIAN_POINT ( 'NONE',  ( -449.9999999999999432, 105.0000000000000142, 187.0000000000000000 ) ) ;
#19176 = ADVANCED_FACE ( 'NONE', ( #21083 ), #4688, .F. ) ;
#19177 = LINE ( 'NONE', #5607, #11817 ) ;
#19178 = CARTESIAN_POINT ( 'NONE',  ( -499.9999999999999432, 136.9999999999999432, -162.9999999999999716 ) ) ;
#19179 = VERTEX_POINT ( 'NONE', #21263 ) ;
#19180 = ORIENTED_EDGE ( 'NONE', *, *, #20522, .T. ) ;
#19181 = DIRECTION ( 'NONE',  ( 0.000000000000000000, 0.000000000000000000, -1.000000000000000000 ) ) ;
#19182 = DIRECTION ( 'NONE',  ( 0.000000000000000000, 1.310824597558155437E-49, 1.000000000000000000 ) ) ;
#19183 = CARTESIAN_POINT ( 'NONE',  ( 0.000000000000000000, 2.281310696040539424E-14, -36.68877005347594178 ) ) ;
#19184 = EDGE_CURVE ( 'NONE', #15995, #17865, #10593, .T. ) ;
#19185 = CARTESIAN_POINT ( 'NONE',  ( 1.040000000000000924, 0.000000000000000000, 0.000000000000000000 ) ) ;
#19186 = CARTESIAN_POINT ( 'NONE',  ( -14.84098889165989377, 28.96462362251111244, 68.31122994652405112 ) ) ;
#19187 = CARTESIAN_POINT ( 'NONE',  ( 11.99999999999999645, 124.9999999999999716, 155.0000000000000000 ) ) ;
#19188 = DIRECTION ( 'NONE',  ( 1.000000000000000000, 0.000000000000000000, 0.000000000000000000 ) ) ;
#19189 = ORIENTED_EDGE ( 'NONE', *, *, #8629, .F. ) ;
#19190 = CARTESIAN_POINT ( 'NONE',  ( 0.000000000000000000, 3.524919873834583163E-15, 68.31122994652405112 ) ) ;
#19191 = CARTESIAN_POINT ( 'NONE',  ( 2.789999999999999147, -21.75986515490491868, 21.28569233123086946 ) ) ;
#19192 = DIRECTION ( 'NONE',  ( -0.000000000000000000, -0.000000000000000000, -1.000000000000000000 ) ) ;
#19193 = ORIENTED_EDGE ( 'NONE', *, *, #1926, .T. ) ;
#19194 = AXIS2_PLACEMENT_3D ( 'NONE', #25511, #12356, #34405 ) ;
#19195 = VECTOR ( 'NONE', #12490, 1000.000000000000000 ) ;
#19196 = ADVANCED_FACE ( 'NONE', ( #24090 ), #7542, .F. ) ;
#19197 = FACE_OUTER_BOUND ( 'NONE', #15912, .T. ) ;
#19198 = VERTEX_POINT ( 'NONE', #32283 ) ;
#19199 = CARTESIAN_POINT ( 'NONE',  ( -109.0611100676622272, 3.127595108844668736, -12.10573782681415267 ) ) ;
#19200 = CARTESIAN_POINT ( 'NONE',  ( -20.00000000000004619, -134.9999999999999716, -162.9999999999999432 ) ) ;
#19201 = VECTOR ( 'NONE', #18827, 1000.000000000000000 ) ;
#19202 = ORIENTED_EDGE ( 'NONE', *, *, #10808, .T. ) ;
#19203 = PLANE ( 'NONE',  #34201 ) ;
#19204 = CARTESIAN_POINT ( 'NONE',  ( 11.99999999999999645, -145.0000000000000000, 174.9999999999999432 ) ) ;
#19205 = DIRECTION ( 'NONE',  ( -1.000000000000000000, 0.000000000000000000, -5.546364386991661285E-52 ) ) ;
#19206 = ORIENTED_EDGE ( 'NONE', *, *, #31412, .T. ) ;
#19207 = VERTEX_POINT ( 'NONE', #13087 ) ;
#19208 = VECTOR ( 'NONE', #31420, 1000.000000000000000 ) ;
#19209 = DIRECTION ( 'NONE',  ( 2.631201909438060585E-14, -5.396010391056496978E-16, 1.000000000000000000 ) ) ;
#19210 = DIRECTION ( 'NONE',  ( 1.000000000000000000, 0.000000000000000000, -1.232595164407831220E-32 ) ) ;
#19211 = EDGE_LOOP ( 'NONE', ( #26270, #13605, #17663, #26337 ) ) ;
#19212 = CARTESIAN_POINT ( 'NONE',  ( 24.11848021413632992, 29.19488569250028220, 68.31122994652405112 ) ) ;
#19213 = EDGE_CURVE ( 'NONE', #18737, #3997, #2216, .T. ) ;
#19214 = CARTESIAN_POINT ( 'NONE',  ( -361.0000000000000000, -125.0000000000000284, 126.0000000000000000 ) ) ;
#19215 = VECTOR ( 'NONE', #27442, 1000.000000000000000 ) ;
#19216 = EDGE_CURVE ( 'NONE', #5102, #12124, #433, .T. ) ;
#19217 = CARTESIAN_POINT ( 'NONE',  ( 2.265105736152236204, 14.91070698422201346, -29.86438609618728890 ) ) ;
#19218 = CARTESIAN_POINT ( 'NONE',  ( 15.99999999999998579, -145.0000000000000000, -186.9999999999999716 ) ) ;
#19219 = ORIENTED_EDGE ( 'NONE', *, *, #25395, .F. ) ;
#19221 = VERTEX_POINT ( 'NONE', #6271 ) ;
#19220 =( REPRESENTATION_RELATIONSHIP ('NONE','NONE', #23037, #15767 ) REPRESENTATION_RELATIONSHIP_WITH_TRANSFORMATION ( #8342 )SHAPE_REPRESENTATION_RELATIONSHIP( ) );
#19222 = ORIENTED_EDGE ( 'NONE', *, *, #26086, .F. ) ;
#19223 = LINE ( 'NONE', #11020, #32302 ) ;
#19224 = FACE_OUTER_BOUND ( 'NONE', #23062, .T. ) ;
#19225 = VECTOR ( 'NONE', #12229, 1000.000000000000000 ) ;
#19226 = CARTESIAN_POINT ( 'NONE',  ( -355.0000000000000000, 118.9999999999999716, 113.9999999999999858 ) ) ;
#19227 = ORIENTED_EDGE ( 'NONE', *, *, #6958, .F. ) ;
#19228 = ORIENTED_EDGE ( 'NONE', *, *, #23910, .T. ) ;
#19229 = CARTESIAN_POINT ( 'NONE',  ( 1.749999999999999778, 34.17636915695680244, -4.045051921974834208 ) ) ;
#19230 = EDGE_LOOP ( 'NONE', ( #31587, #31860, #33636, #7587, #27660, #28816 ) ) ;
#19231 = DIRECTION ( 'NONE',  ( -0.000000000000000000, -0.000000000000000000, 1.000000000000000000 ) ) ;
#19232 = CARTESIAN_POINT ( 'NONE',  ( 42.44043929807611448, -17.65143121711728469, 20.00000000000000000 ) ) ;
#19233 = ORIENTED_EDGE ( 'NONE', *, *, #15929, .F. ) ;
#19234 = VERTEX_POINT ( 'NONE', #8967 ) ;
#19235 = DIRECTION ( 'NONE',  ( -1.000000000000000000, 0.000000000000000000, -0.000000000000000000 ) ) ;
#19236 = CIRCLE ( 'NONE', #21480, 34.41491905851385269 ) ;
#19237 = CARTESIAN_POINT ( 'NONE',  ( 2.790000000000000036, 29.09243261715505469, -9.683176917503056202 ) ) ;
#19238 = VERTEX_POINT ( 'NONE', #13967 ) ;
#19239 = DIRECTION ( 'NONE',  ( -0.000000000000000000, -1.836970198721029688E-16, 1.000000000000000000 ) ) ;
#19240 = LINE ( 'NONE', #15877, #16033 ) ;
#19241 = PLANE ( 'NONE',  #4160 ) ;
#19242 = CARTESIAN_POINT ( 'NONE',  ( -1.625000000000000000, -1.866624223957557671, 4.679999999999999716 ) ) ;
#19243 = PRESENTATION_LAYER_ASSIGNMENT (  '', '', ( #31172 ) ) ;
#19244 = PRESENTATION_LAYER_ASSIGNMENT (  '', '', ( #18605 ) ) ;
#19245 = LINE ( 'NONE', #19415, #28492 ) ;
#19246 = DIRECTION ( 'NONE',  ( 1.000000000000000000, 0.000000000000000000, 0.000000000000000000 ) ) ;
#19247 = DIRECTION ( 'NONE',  ( 1.848892746611746419E-32, 6.842277657836020854E-49, -1.000000000000000000 ) ) ;
#19248 = AXIS2_PLACEMENT_3D ( 'NONE', #18394, #26380, #5178 ) ;
#19249 = ORIENTED_EDGE ( 'NONE', *, *, #24948, .T. ) ;
#19250 = DIRECTION ( 'NONE',  ( -1.000000000000000000, -0.000000000000000000, -0.000000000000000000 ) ) ;
#19251 = CARTESIAN_POINT ( 'NONE',  ( 844.3520950806066594, 1093.298738741797706, 1753.598338701303646 ) ) ;
#19252 = ORIENTED_EDGE ( 'NONE', *, *, #12304, .F. ) ;
#19253 = ORIENTED_EDGE ( 'NONE', *, *, #30385, .F. ) ;
#19254 = ADVANCED_FACE ( 'NONE', ( #8255 ), #30507, .F. ) ;
#19255 = VECTOR ( 'NONE', #9461, 1000.000000000000000 ) ;
#19256 = EDGE_CURVE ( 'NONE', #30159, #32496, #33164, .T. ) ;
#19257 = EDGE_CURVE ( 'NONE', #29040, #19647, #3087, .T. ) ;
#19258 = VECTOR ( 'NONE', #28872, 1000.000000000000000 ) ;
#19259 = LINE ( 'NONE', #30454, #9116 ) ;
#19260 = ORIENTED_EDGE ( 'NONE', *, *, #33789, .T. ) ;
#19261 = EDGE_CURVE ( 'NONE', #26118, #27945, #22319, .T. ) ;
#19262 = CARTESIAN_POINT ( 'NONE',  ( -347.0000000000000000, -125.0000000000000284, 181.0000000000000000 ) ) ;
#19263 = CARTESIAN_POINT ( 'NONE',  ( -449.9999999999999432, 137.0000000000000000, 154.9999999999999716 ) ) ;
#19264 = ITEM_DEFINED_TRANSFORMATION ( 'NONE', 'NONE', #12747,  #28566 ) ;
#19265 = VECTOR ( 'NONE', #10446, 1000.000000000000000 ) ;
#19267 = DIRECTION ( 'NONE',  ( 0.000000000000000000, 0.000000000000000000, 1.000000000000000000 ) ) ;
#19266 = DIRECTION ( 'NONE',  ( 0.000000000000000000, 0.000000000000000000, 1.000000000000000000 ) ) ;
#19268 = ORIENTED_EDGE ( 'NONE', *, *, #24823, .F. ) ;
#19269 = ORIENTED_EDGE ( 'NONE', *, *, #16373, .F. ) ;
#19270 = FACE_OUTER_BOUND ( 'NONE', #24434, .T. ) ;
#19271 = DIRECTION ( 'NONE',  ( -1.000000000000000000, 0.000000000000000000, 0.000000000000000000 ) ) ;
#19272 = CARTESIAN_POINT ( 'NONE',  ( 0.1859802604725803721, 12.64393372169665675, 29.70253967906869974 ) ) ;
#19273 = CYLINDRICAL_SURFACE ( 'NONE', #2303, 2.033421858999711951 ) ;
#19274 = DIRECTION ( 'NONE',  ( 0.000000000000000000, 1.836970198721029441E-16, -1.000000000000000000 ) ) ;
#19275 = EDGE_LOOP ( 'NONE', ( #1446, #21063, #1964, #34424 ) ) ;
#19276 = VECTOR ( 'NONE', #5101, 1000.000000000000000 ) ;
#19277 = LINE ( 'NONE', #8745, #10102 ) ;
#19278 = PLANE ( 'NONE',  #31059 ) ;
#19279 = DIRECTION ( 'NONE',  ( -1.000000000000000000, 0.000000000000000000, -0.000000000000000000 ) ) ;
#19280 = DIRECTION ( 'NONE',  ( -0.9941379571543593752, 0.1081190184239433083, 0.000000000000000000 ) ) ;
#19281 = DIRECTION ( 'NONE',  ( 0.000000000000000000, 0.000000000000000000, 1.000000000000000000 ) ) ;
#19283 = DIRECTION ( 'NONE',  ( 0.000000000000000000, 0.000000000000000000, 1.000000000000000000 ) ) ;
#19282 = PLANE ( 'NONE',  #5347 ) ;
#19284 = VECTOR ( 'NONE', #7988, 1000.000000000000000 ) ;
#19285 = CARTESIAN_POINT ( 'NONE',  ( 2.789999999999999147, 25.67797970382158113, -16.40405592474728635 ) ) ;
#19286 = ORIENTED_EDGE ( 'NONE', *, *, #25749, .T. ) ;
#19287 = CARTESIAN_POINT ( 'NONE',  ( 11.99999999999999645, 108.9999999999999858, -175.0000000000000284 ) ) ;
#19289 = CARTESIAN_POINT ( 'NONE',  ( 109.9362594651775140, -2.948796715283049874, -6.904248079351286371 ) ) ;
#19288 = CARTESIAN_POINT ( 'NONE',  ( -355.0000000000000000, -135.0000000000000000, 109.9999999999999858 ) ) ;
#19290 = ORIENTED_EDGE ( 'NONE', *, *, #10876, .F. ) ;
#19291 = EDGE_CURVE ( 'NONE', #30767, #14102, #11833, .T. ) ;
#19292 = EDGE_LOOP ( 'NONE', ( #1412, #1540, #4303, #30971, #28542, #22154 ) ) ;
#19293 = EDGE_CURVE ( 'NONE', #23708, #34034, #27291, .T. ) ;
#19294 = AXIS2_PLACEMENT_3D ( 'NONE', #8087, #21976, #29463 ) ;
#19295 = EDGE_LOOP ( 'NONE', ( #19501, #1392 ) ) ;
#19296 = DIRECTION ( 'NONE',  ( 0.000000000000000000, 0.000000000000000000, 1.000000000000000000 ) ) ;
#19297 = VERTEX_POINT ( 'NONE', #21967 ) ;
#19298 = ORIENTED_EDGE ( 'NONE', *, *, #18219, .T. ) ;
#19299 = EDGE_CURVE ( 'NONE', #7013, #18126, #8603, .T. ) ;
#19300 = DIRECTION ( 'NONE',  ( 0.000000000000000000, 1.224646799147353207E-16, -1.000000000000000000 ) ) ;
#19301 = CIRCLE ( 'NONE', #20446, 7.999999999999979572 ) ;
#19302 = LINE ( 'NONE', #2733, #16957 ) ;
#19303 = CARTESIAN_POINT ( 'NONE',  ( -361.0000000000000000, 134.9999999999999716, 126.0000000000000000 ) ) ;
#19304 = ORIENTED_EDGE ( 'NONE', *, *, #30830, .T. ) ;
#19305 = EDGE_CURVE ( 'NONE', #2690, #22142, #22498, .T. ) ;
#19306 = ORIENTED_EDGE ( 'NONE', *, *, #31267, .T. ) ;
#19307 = DIRECTION ( 'NONE',  ( 0.000000000000000000, -3.374343856708137958E-53, 1.000000000000000000 ) ) ;
#19308 = DIRECTION ( 'NONE',  ( 0.000000000000000000, 1.310824597558155437E-49, 1.000000000000000000 ) ) ;
#19309 = ADVANCED_FACE ( 'NONE', ( #16828 ), #19839, .F. ) ;
#19310 = CARTESIAN_POINT ( 'NONE',  ( 104.0571527818341906, -5.663308120860368611, -11.14355020191728762 ) ) ;
#19311 = CYLINDRICAL_SURFACE ( 'NONE', #8571, 7.999999999999979572 ) ;
#19312 = EDGE_LOOP ( 'NONE', ( #28501, #19907, #15237, #33976 ) ) ;
#19313 = EDGE_CURVE ( 'NONE', #26108, #10330, #14321, .T. ) ;
#19314 = LINE ( 'NONE', #3095, #20786 ) ;
#19315 = DIRECTION ( 'NONE',  ( -1.000000000000000000, 6.792721752314501023E-48, -3.697785493223492838E-32 ) ) ;
#19316 = ORIENTED_EDGE ( 'NONE', *, *, #26675, .F. ) ;
#19317 = CARTESIAN_POINT ( 'NONE',  ( -5.038454199367317088, -32.15304576796697233, 68.31122994652405112 ) ) ;
#19318 = DIRECTION ( 'NONE',  ( 0.000000000000000000, 0.000000000000000000, -1.000000000000000000 ) ) ;
#19319 = FACE_OUTER_BOUND ( 'NONE', #22885, .T. ) ;
#19320 = CIRCLE ( 'NONE', #558, 4.750000000000004441 ) ;
#19321 = DIRECTION ( 'NONE',  ( 0.000000000000000000, 2.309213040847544338E-50, 1.000000000000000000 ) ) ;
#19322 = ORIENTED_EDGE ( 'NONE', *, *, #17590, .T. ) ;
#19323 = DIRECTION ( 'NONE',  ( 0.000000000000000000, 2.309213040847544338E-50, 1.000000000000000000 ) ) ;
#19324 = ORIENTED_EDGE ( 'NONE', *, *, #15719, .T. ) ;
#19326 = CARTESIAN_POINT ( 'NONE',  ( 0.07094833404649768249, 21.26181984063927999, -23.50417665061993944 ) ) ;
#19325 = SURFACE_STYLE_USAGE ( .BOTH. , #34999 ) ;
#19327 = FACE_OUTER_BOUND ( 'NONE', #19916, .T. ) ;
#19328 = AXIS2_PLACEMENT_3D ( 'NONE', #9099, #30643, #33310 ) ;
#19329 = EDGE_LOOP ( 'NONE', ( #11894, #6270, #33336, #13956, #30846, #13843 ) ) ;
#19330 = DIRECTION ( 'NONE',  ( -0.2675283385292216987, 0.9635499925192227977, 0.000000000000000000 ) ) ;
#19331 = CYLINDRICAL_SURFACE ( 'NONE', #16032, 3.999999999999982681 ) ;
#19332 = ORIENTED_EDGE ( 'NONE', *, *, #19121, .F. ) ;
#19333 = ORIENTED_EDGE ( 'NONE', *, *, #33292, .F. ) ;
#19334 = ORIENTED_EDGE ( 'NONE', *, *, #13033, .T. ) ;
#19335 = CARTESIAN_POINT ( 'NONE',  ( -20.00000000000007461, 136.9999999999999432, -159.0000000000000000 ) ) ;
#19336 = CARTESIAN_POINT ( 'NONE',  ( -20.00000000000007461, 104.9999999999999858, -187.0000000000000000 ) ) ;
#19337 = ORIENTED_EDGE ( 'NONE', *, *, #480, .T. ) ;
#19338 = VERTEX_POINT ( 'NONE', #6103 ) ;
#19339 = FACE_OUTER_BOUND ( 'NONE', #32665, .T. ) ;
#19340 = EDGE_CURVE ( 'NONE', #17151, #5081, #31596, .T. ) ;
#19341 = VECTOR ( 'NONE', #27597, 1000.000000000000000 ) ;
#19342 = CYLINDRICAL_SURFACE ( 'NONE', #24954, 16.19999999999999574 ) ;
#19343 = CARTESIAN_POINT ( 'NONE',  ( 129.3530333899765594, 6.000000000000000000, -57.49999999999999289 ) ) ;
#19344 = CARTESIAN_POINT ( 'NONE',  ( -442.0000000000000000, 105.0000000000000000, 132.0000000000000000 ) ) ;
#19345 = EDGE_CURVE ( 'NONE', #319, #11101, #11159, .T. ) ;
#19346 = VERTEX_POINT ( 'NONE', #25328 ) ;
#19347 = ADVANCED_FACE ( 'NONE', ( #17002, #779 ), #11648, .T. ) ;
#19348 = ORIENTED_EDGE ( 'NONE', *, *, #16488, .T. ) ;
#19349 = CARTESIAN_POINT ( 'NONE',  ( -5.021133111224782120, 16.12922284503174097, -87.50000000000000000 ) ) ;
#19350 = DIRECTION ( 'NONE',  ( -0.000000000000000000, -0.000000000000000000, -1.000000000000000000 ) ) ;
#19351 = CARTESIAN_POINT ( 'NONE',  ( 0.000000000000000000, 3.524919873834583163E-15, 68.31122994652405112 ) ) ;
#19352 = CARTESIAN_POINT ( 'NONE',  ( -349.0000000000000000, -135.0000000000000000, 126.0000000000000000 ) ) ;
#19353 = LINE ( 'NONE', #3316, #25894 ) ;
#19354 = FACE_OUTER_BOUND ( 'NONE', #14178, .T. ) ;
#19355 = CARTESIAN_POINT ( 'NONE',  ( 9.199999999999999289, -11.69134295108990962, 6.750000000000026645 ) ) ;
#19356 = VERTEX_POINT ( 'NONE', #24971 ) ;
#19357 = DIRECTION ( 'NONE',  ( -1.000000000000000000, 0.000000000000000000, -0.000000000000000000 ) ) ;
#19358 = DIRECTION ( 'NONE',  ( -1.000000000000000000, 0.000000000000000000, -0.000000000000000000 ) ) ;
#19359 = ADVANCED_FACE ( 'NONE', ( #599 ), #16467, .F. ) ;
#19360 = DIRECTION ( 'NONE',  ( 0.000000000000000000, 0.000000000000000000, 1.000000000000000000 ) ) ;
#19361 = ORIENTED_EDGE ( 'NONE', *, *, #11093, .T. ) ;
#19362 = DIRECTION ( 'NONE',  ( -1.000000000000000000, -0.000000000000000000, -0.000000000000000000 ) ) ;
#19363 = ORIENTED_EDGE ( 'NONE', *, *, #26354, .F. ) ;
#19364 = CARTESIAN_POINT ( 'NONE',  ( -5.038454199367317088, -32.15304576796695102, -36.68877005347593467 ) ) ;
#19365 = CARTESIAN_POINT ( 'NONE',  ( -105.3347027237455080, 5.115232524641490919, 11.40545467192879947 ) ) ;
#19366 = EDGE_CURVE ( 'NONE', #14308, #9458, #24614, .T. ) ;
#19367 = VECTOR ( 'NONE', #31971, 1000.000000000000000 ) ;
#19368 = EDGE_CURVE ( 'NONE', #24651, #6040, #20520, .T. ) ;
#19369 = EDGE_CURVE ( 'NONE', #15358, #17291, #31546, .T. ) ;
#19370 = ORIENTED_EDGE ( 'NONE', *, *, #22980, .F. ) ;
#19371 = DIRECTION ( 'NONE',  ( 1.848892746611746419E-32, 6.842277657836020854E-49, -1.000000000000000000 ) ) ;
#19372 = CARTESIAN_POINT ( 'NONE',  ( -418.0000000000000000, -105.0000000000000142, -105.9999999999999574 ) ) ;
#19373 = CARTESIAN_POINT ( 'NONE',  ( -12.00000000000001066, -109.0000000000000142, -155.0000000000000284 ) ) ;
#19374 = EDGE_CURVE ( 'NONE', #10833, #23287, #12518, .T. ) ;
#19375 = EDGE_LOOP ( 'NONE', ( #7479, #28932, #5943, #9785 ) ) ;
#19376 = AXIS2_PLACEMENT_3D ( 'NONE', #18830, #965, #11652 ) ;
#19377 = CARTESIAN_POINT ( 'NONE',  ( 832.5958878573111406, 1203.171521049847570, 1753.598338701303192 ) ) ;
#19378 = TOROIDAL_SURFACE ( 'NONE', #17684, 30.47050528711512030, 8.000000000000000000 ) ;
#19379 = DIRECTION ( 'NONE',  ( -1.000000000000000000, -0.000000000000000000, -0.000000000000000000 ) ) ;
#19380 = ORIENTED_EDGE ( 'NONE', *, *, #23923, .T. ) ;
#19381 = DIRECTION ( 'NONE',  ( 0.000000000000000000, -0.000000000000000000, 1.000000000000000000 ) ) ;
#19382 = CARTESIAN_POINT ( 'NONE',  ( -35.71762877834949990, -12.58147180936567011, 68.31122994652405112 ) ) ;
#19383 = DIRECTION ( 'NONE',  ( -3.040835319149746090E-31, -1.000000000000000000, 0.000000000000000000 ) ) ;
#19384 = CARTESIAN_POINT ( 'NONE',  ( -101.6215955338914370, -3.854070255762961139, 6.439229133474693612 ) ) ;
#19385 = ITEM_DEFINED_TRANSFORMATION ( 'NONE', 'NONE', #30904,  #28566 ) ;
#19386 = EDGE_CURVE ( 'NONE', #20322, #27420, #27050, .T. ) ;
#19387 = ORIENTED_EDGE ( 'NONE', *, *, #26521, .F. ) ;
#19388 = EDGE_CURVE ( 'NONE', #9166, #18057, #4877, .T. ) ;
#19389 = ORIENTED_EDGE ( 'NONE', *, *, #5835, .F. ) ;
#19390 = VERTEX_POINT ( 'NONE', #1480 ) ;
#19391 = CIRCLE ( 'NONE', #1743, 3.999999999999976019 ) ;
#19392 = DIRECTION ( 'NONE',  ( -0.8568571761675904952, 0.5155538571770196254, 0.000000000000000000 ) ) ;
#19394 = AXIS2_PLACEMENT_3D ( 'NONE', #17919, #4346, #15403 ) ;
#19393 = DIRECTION ( 'NONE',  ( 0.000000000000000000, 0.000000000000000000, -1.000000000000000000 ) ) ;
#19395 = CARTESIAN_POINT ( 'NONE',  ( -15.99999999999998579, 4.559999999999908127, 172.9900000000000091 ) ) ;
#19396 = ORIENTED_EDGE ( 'NONE', *, *, #30229, .T. ) ;
#19397 = ORIENTED_EDGE ( 'NONE', *, *, #30216, .F. ) ;
#19398 = DIRECTION ( 'NONE',  ( 0.000000000000000000, 0.000000000000000000, 1.000000000000000000 ) ) ;
#19399 = ORIENTED_EDGE ( 'NONE', *, *, #10175, .F. ) ;
#19400 = CARTESIAN_POINT ( 'NONE',  ( -3.250000000000000000, -5.838643359331793015, 3.930000000000000160 ) ) ;
#19401 = DIRECTION ( 'NONE',  ( -0.000000000000000000, 1.000000000000000000, -0.000000000000000000 ) ) ;
#19402 = ORIENTED_EDGE ( 'NONE', *, *, #858, .F. ) ;
#19403 = ORIENTED_EDGE ( 'NONE', *, *, #28692, .F. ) ;
#19404 = CARTESIAN_POINT ( 'NONE',  ( -35.00000000000000000, 3.353962854566122864, -15.81122994652406355 ) ) ;
#19405 = AXIS2_PLACEMENT_3D ( 'NONE', #818, #8528, #16738 ) ;
#19406 = AXIS2_PLACEMENT_3D ( 'NONE', #15169, #1974, #32040 ) ;
#19407 = CARTESIAN_POINT ( 'NONE',  ( -7.700000000000000178, 0.000000000000000000, 0.000000000000000000 ) ) ;
#19408 = ORIENTED_EDGE ( 'NONE', *, *, #18772, .F. ) ;
#19409 = DIRECTION ( 'NONE',  ( -1.000000000000000000, -0.000000000000000000, -0.000000000000000000 ) ) ;
#19410 = CARTESIAN_POINT ( 'NONE',  ( -9.144464960067640646, -31.23432620483745836, 68.31122994652405112 ) ) ;
#19411 = LINE ( 'NONE', #3544, #15565 ) ;
#19412 = EDGE_CURVE ( 'NONE', #30341, #3104, #32153, .T. ) ;
#19413 = DIRECTION ( 'NONE',  ( 0.000000000000000000, 0.000000000000000000, -1.000000000000000000 ) ) ;
#19414 = EDGE_CURVE ( 'NONE', #19338, #29324, #12305, .T. ) ;
#19415 = CARTESIAN_POINT ( 'NONE',  ( -12.00000000000001066, -124.9999999999999432, -154.9999999999999716 ) ) ;
#19416 = CYLINDRICAL_SURFACE ( 'NONE', #24716, 16.19999999999999574 ) ;
#19417 = VECTOR ( 'NONE', #6810, 1000.000000000000000 ) ;
#19418 = CARTESIAN_POINT ( 'NONE',  ( -144.4704739938196099, -45.49999999999999289, 63.00000000000000000 ) ) ;
#19419 = EDGE_CURVE ( 'NONE', #9979, #10097, #33302, .T. ) ;
#19420 = VECTOR ( 'NONE', #16999, 1000.000000000000000 ) ;
#19421 = VERTEX_POINT ( 'NONE', #31373 ) ;
#19422 = CARTESIAN_POINT ( 'NONE',  ( 0.000000000000000000, -33.69708579775585378, -36.68877005347594178 ) ) ;
#19423 = DIRECTION ( 'NONE',  ( 0.1063910735368947813, -0.9943243633099144718, -3.335902418024520312E-15 ) ) ;
#19424 = EDGE_CURVE ( 'NONE', #9180, #12202, #6453, .T. ) ;
#19425 = ORIENTED_EDGE ( 'NONE', *, *, #4788, .T. ) ;
#19426 = ORIENTED_EDGE ( 'NONE', *, *, #14879, .F. ) ;
#19427 = DIRECTION ( 'NONE',  ( 0.000000000000000000, 0.000000000000000000, -1.000000000000000000 ) ) ;
#19428 = CIRCLE ( 'NONE', #2914, 1.649999999999999467 ) ;
#19429 = CARTESIAN_POINT ( 'NONE',  ( 103.4583262007279245, 5.530333585247596773, 5.066783516361279993 ) ) ;
#19430 = APPLICATION_PROTOCOL_DEFINITION ( 'draft international standard', 'automotive_design', 1998, #1679 ) ;
#19431 = ORIENTED_EDGE ( 'NONE', *, *, #27319, .T. ) ;
#19432 = VECTOR ( 'NONE', #15222, 1000.000000000000000 ) ;
#19433 = AXIS2_PLACEMENT_3D ( 'NONE', #931, #11801, #33662 ) ;
#19434 = DIRECTION ( 'NONE',  ( 0.000000000000000000, -1.000000000000000000, 2.225651257388386197E-16 ) ) ;
#19435 = DIRECTION ( 'NONE',  ( -0.05413890858541786644, 0.9985334138511238189, 0.000000000000000000 ) ) ;
#19437 = CARTESIAN_POINT ( 'NONE',  ( 2.789999999999999147, -8.813854705727671046, 29.13568936554939981 ) ) ;
#19436 = CARTESIAN_POINT ( 'NONE',  ( 2.033800776873903704, -18.61835568386960915, 28.34776818504836626 ) ) ;
#19438 = EDGE_LOOP ( 'NONE', ( #14847, #13465, #26234, #13774 ) ) ;
#19439 = VERTEX_POINT ( 'NONE', #15018 ) ;
#19440 = CARTESIAN_POINT ( 'NONE',  ( 12.00000000000003908, -115.0000000000000000, -158.9999999999999716 ) ) ;
#19441 = ADVANCED_FACE ( 'NONE', ( #17873 ), #26197, .T. ) ;
#19442 = CARTESIAN_POINT ( 'NONE',  ( 1.749999999999999778, 0.000000000000000000, 0.000000000000000000 ) ) ;
#19443 = CARTESIAN_POINT ( 'NONE',  ( 15.99999999999997868, -137.0000000000000000, 155.0000000000000000 ) ) ;
#19444 = PLANE ( 'NONE',  #29185 ) ;
#19445 = ORIENTED_EDGE ( 'NONE', *, *, #8629, .T. ) ;
#19446 = VECTOR ( 'NONE', #26293, 1000.000000000000000 ) ;
#19447 = CARTESIAN_POINT ( 'NONE',  ( 5.021133111224369117, -3.725253662474303784, -67.50000000000000000 ) ) ;
#19448 = CARTESIAN_POINT ( 'NONE',  ( 105.0000000000000000, 0.000000000000000000, 60.00000000000000000 ) ) ;
#19449 = DIRECTION ( 'NONE',  ( 1.000000000000000000, 0.000000000000000000, 0.000000000000000000 ) ) ;
#19450 = EDGE_LOOP ( 'NONE', ( #31579, #31869, #11450, #29078, #33870, #16432 ) ) ;
#19451 = PLANE ( 'NONE',  #32254 ) ;
#19452 = EDGE_CURVE ( 'NONE', #13509, #32964, #7128, .T. ) ;
#19453 = CARTESIAN_POINT ( 'NONE',  ( -449.9999999999999432, 113.0000000000000000, -175.0000000000000000 ) ) ;
#19454 = LINE ( 'NONE', #16616, #11555 ) ;
#19455 = EDGE_CURVE ( 'NONE', #26862, #11246, #1819, .T. ) ;
#19458 = DIRECTION ( 'NONE',  ( 0.000000000000000000, 0.000000000000000000, 1.000000000000000000 ) ) ;
#19457 = DIRECTION ( 'NONE',  ( 0.000000000000000000, 0.000000000000000000, 1.000000000000000000 ) ) ;
#19456 = CIRCLE ( 'NONE', #20014, 7.999999999999979572 ) ;
#19459 = ADVANCED_FACE ( 'NONE', ( #26032 ), #9661, .T. ) ;
#19460 = VECTOR ( 'NONE', #5623, 1000.000000000000114 ) ;
#19461 = LINE ( 'NONE', #14115, #26931 ) ;
#19462 = ORIENTED_EDGE ( 'NONE', *, *, #30508, .F. ) ;
#19464 = CIRCLE ( 'NONE', #8641, 3.999999999999976019 ) ;
#19463 = CYLINDRICAL_SURFACE ( 'NONE', #20168, 7.999999999999979572 ) ;
#19465 = ORIENTED_EDGE ( 'NONE', *, *, #31516, .F. ) ;
#19466 = EDGE_LOOP ( 'NONE', ( #21362, #25971 ) ) ;
#19467 =( REPRESENTATION_RELATIONSHIP ('NONE','NONE', #23037, #28231 ) REPRESENTATION_RELATIONSHIP_WITH_TRANSFORMATION ( #8914 )SHAPE_REPRESENTATION_RELATIONSHIP( ) );
#19468 = ORIENTED_EDGE ( 'NONE', *, *, #30577, .T. ) ;
#19469 = CARTESIAN_POINT ( 'NONE',  ( 11.99999999999999645, -145.0000000000000000, -194.9999999999999432 ) ) ;
#19470 = EDGE_LOOP ( 'NONE', ( #252, #23422, #21515, #16894 ) ) ;
#19471 = ORIENTED_EDGE ( 'NONE', *, *, #4540, .F. ) ;
#19472 = CARTESIAN_POINT ( 'NONE',  ( 1.394999999999999574, 21.72796464722046039, -26.68861566460872936 ) ) ;
#19474 = VECTOR ( 'NONE', #27280, 1000.000000000000114 ) ;
#19473 = ITEM_DEFINED_TRANSFORMATION ( 'NONE', 'NONE', #15529,  #28566 ) ;
#19475 = ORIENTED_EDGE ( 'NONE', *, *, #18020, .T. ) ;
#19476 = CARTESIAN_POINT ( 'NONE',  ( 11.99999999999999645, 136.9999999999999716, -155.0000000000000000 ) ) ;
#19477 = VECTOR ( 'NONE', #10778, 1000.000000000000000 ) ;
#19478 = CARTESIAN_POINT ( 'NONE',  ( -499.9999999999999432, -105.0000000000000142, -187.0000000000000000 ) ) ;
#19479 = ORIENTED_EDGE ( 'NONE', *, *, #25230, .T. ) ;
#19480 = CIRCLE ( 'NONE', #1282, 8.000000000000000000 ) ;
#19481 = ORIENTED_EDGE ( 'NONE', *, *, #11621, .T. ) ;
#19482 = AXIS2_PLACEMENT_3D ( 'NONE', #5584, #449, #8272 ) ;
#19483 = CARTESIAN_POINT ( 'NONE',  ( -144.4704739938196099, -85.49999999999998579, 63.00000000000000000 ) ) ;
#19484 = CARTESIAN_POINT ( 'NONE',  ( 17.27856612038524631, 33.69708579775584667, 68.31122994652405112 ) ) ;
#19485 = CARTESIAN_POINT ( 'NONE',  ( -37.12776225901827587, -7.411627343331159246, 68.31122994652405112 ) ) ;
#19486 = DIRECTION ( 'NONE',  ( -1.000000000000000000, 0.000000000000000000, 0.000000000000000000 ) ) ;
#19487 = ORIENTED_EDGE ( 'NONE', *, *, #19388, .F. ) ;
#19488 = DIRECTION ( 'NONE',  ( -1.000000000000000000, 0.000000000000000000, 0.000000000000000000 ) ) ;
#19489 = DIRECTION ( 'NONE',  ( 1.000000000000000000, -0.000000000000000000, -0.000000000000000000 ) ) ;
#19490 = ORIENTED_EDGE ( 'NONE', *, *, #13663, .T. ) ;
#19491 = ADVANCED_FACE ( 'NONE', ( #1649 ), #25861, .T. ) ;
#19492 = DIRECTION ( 'NONE',  ( -0.000000000000000000, -0.000000000000000000, -1.000000000000000000 ) ) ;
#19493 = CARTESIAN_POINT ( 'NONE',  ( -5.021133111225196011, -25.61315202898006049, -67.50000000000000000 ) ) ;
#19494 = EDGE_CURVE ( 'NONE', #34043, #32609, #1466, .T. ) ;
#19495 = PLANE ( 'NONE',  #4696 ) ;
#19496 = CARTESIAN_POINT ( 'NONE',  ( 2.033800773692430397, 6.875399836226916861, -33.21096214980137518 ) ) ;
#19497 = ORIENTED_EDGE ( 'NONE', *, *, #29083, .T. ) ;
#19498 = ADVANCED_BREP_SHAPE_REPRESENTATION ( '', ( #10060, #28566 ), #30284 ) ;
#19499 = EDGE_CURVE ( 'NONE', #9157, #28176, #10573, .T. ) ;
#19500 = CARTESIAN_POINT ( 'NONE',  ( -499.9999999999999432, 136.9999999999999432, -194.9999999999999716 ) ) ;
#19501 = ORIENTED_EDGE ( 'NONE', *, *, #18287, .F. ) ;
#19502 = EDGE_CURVE ( 'NONE', #10848, #4890, #6632, .T. ) ;
#19504 = CARTESIAN_POINT ( 'NONE',  ( -442.0000000000000000, 137.0000000000000000, -175.0000000000000000 ) ) ;
#19503 = PLANE ( 'NONE',  #33024 ) ;
#19505 = AXIS2_PLACEMENT_3D ( 'NONE', #16058, #31861, #16234 ) ;
#19507 = ORIENTED_EDGE ( 'NONE', *, *, #9275, .F. ) ;
#19506 = VECTOR ( 'NONE', #9600, 1000.000000000000000 ) ;
#19508 = VECTOR ( 'NONE', #13199, 1000.000000000000000 ) ;
#19509 = VECTOR ( 'NONE', #29767, 1000.000000000000000 ) ;
#19510 = DIRECTION ( 'NONE',  ( -1.000000000000000000, 0.000000000000000000, 0.000000000000000000 ) ) ;
#19511 = EDGE_CURVE ( 'NONE', #12135, #3029, #14848, .T. ) ;
#19512 = ORIENTED_EDGE ( 'NONE', *, *, #14966, .T. ) ;
#19513 = ORIENTED_EDGE ( 'NONE', *, *, #34641, .F. ) ;
#19514 = EDGE_LOOP ( 'NONE', ( #15177, #32486, #11883, #24128 ) ) ;
#19515 = DIRECTION ( 'NONE',  ( 0.000000000000000000, 1.000000000000000000, 0.000000000000000000 ) ) ;
#19516 = DIRECTION ( 'NONE',  ( -0.9985334138511239299, 0.05413890858541753337, 0.000000000000000000 ) ) ;
#19517 = ORIENTED_EDGE ( 'NONE', *, *, #25004, .T. ) ;
#19518 = ORIENTED_EDGE ( 'NONE', *, *, #34922, .F. ) ;
#19519 = DIRECTION ( 'NONE',  ( 0.000000000000000000, 0.000000000000000000, 1.000000000000000000 ) ) ;
#19520 = DIRECTION ( 'NONE',  ( 2.891205793294675368E-16, 7.888609052210118054E-31, 1.000000000000000000 ) ) ;
#19521 = VECTOR ( 'NONE', #22514, 1000.000000000000114 ) ;
#19522 = DIRECTION ( 'NONE',  ( 0.000000000000000000, -0.000000000000000000, 1.000000000000000000 ) ) ;
#19523 = LINE ( 'NONE', #20052, #25055 ) ;
#19524 = VERTEX_POINT ( 'NONE', #31880 ) ;
#19525 = VERTEX_POINT ( 'NONE', #18575 ) ;
#19526 = DIRECTION ( 'NONE',  ( -1.000000000000000000, -0.000000000000000000, -0.000000000000000000 ) ) ;
#19527 = LINE ( 'NONE', #8650, #31687 ) ;
#19528 = LINE ( 'NONE', #3135, #10655 ) ;
#19529 = DIRECTION ( 'NONE',  ( 0.000000000000000000, -1.000000000000000000, 6.123233995736766036E-17 ) ) ;
#19530 = AXIS2_PLACEMENT_3D ( 'NONE', #7052, #31109, #26107 ) ;
#19531 = CARTESIAN_POINT ( 'NONE',  ( -8.267476927982267298, 31.47782073335735831, 68.31122994652405112 ) ) ;
#19532 = VECTOR ( 'NONE', #24676, 1000.000000000000000 ) ;
#19533 = DIRECTION ( 'NONE',  ( -0.2149704402110243495, -0.9766205557100865464, 0.000000000000000000 ) ) ;
#19534 = DIRECTION ( 'NONE',  ( 0.000000000000000000, 0.000000000000000000, 1.000000000000000000 ) ) ;
#19535 = EDGE_LOOP ( 'NONE', ( #1735, #17641, #13435, #22692 ) ) ;
#19536 = DIRECTION ( 'NONE',  ( 1.000000000000000000, 0.000000000000000000, 0.000000000000000000 ) ) ;
#19537 = CYLINDRICAL_SURFACE ( 'NONE', #2357, 2.033421858999711951 ) ;
#19538 = EDGE_CURVE ( 'NONE', #3093, #16221, #2629, .T. ) ;
#19539 = CARTESIAN_POINT ( 'NONE',  ( -500.0000000000000000, -113.0000000000000000, 194.9999999999999716 ) ) ;
#19540 = ORIENTED_EDGE ( 'NONE', *, *, #16552, .F. ) ;
#19541 = CARTESIAN_POINT ( 'NONE',  ( -418.0000000000000000, -112.9999999999999858, -174.9999999999999716 ) ) ;
#19542 = VERTEX_POINT ( 'NONE', #21399 ) ;
#19543 = EDGE_CURVE ( 'NONE', #28747, #32609, #25799, .T. ) ;
#19544 = LINE ( 'NONE', #11531, #29271 ) ;
#19545 = DIRECTION ( 'NONE',  ( 1.000000000000000000, 3.040835319149746528E-31, 1.232595164407830946E-32 ) ) ;
#19546 = EDGE_CURVE ( 'NONE', #24034, #2524, #4828, .T. ) ;
#19547 = ORIENTED_EDGE ( 'NONE', *, *, #31018, .T. ) ;
#19548 = EDGE_CURVE ( 'NONE', #22594, #33860, #8035, .T. ) ;
#19549 = EDGE_CURVE ( 'NONE', #8592, #32250, #7679, .T. ) ;
#19550 = LINE ( 'NONE', #5992, #18323 ) ;
#19551 = FACE_OUTER_BOUND ( 'NONE', #20315, .T. ) ;
#19552 = PLANE ( 'NONE',  #11494 ) ;
#19553 = ORIENTED_EDGE ( 'NONE', *, *, #8934, .F. ) ;
#19554 = PRODUCT_DEFINITION_FORMATION_WITH_SPECIFIED_SOURCE ( 'ANY', '', #11202, .NOT_KNOWN. ) ;
#19555 = AXIS2_PLACEMENT_3D ( 'NONE', #19855, #30870, #6476 ) ;
#19556 = DIRECTION ( 'NONE',  ( 2.631201909438060585E-14, -5.396010391056496978E-16, 1.000000000000000000 ) ) ;
#19557 = DIRECTION ( 'NONE',  ( 0.000000000000000000, -0.000000000000000000, 1.000000000000000000 ) ) ;
#19558 = ORIENTED_EDGE ( 'NONE', *, *, #1873, .T. ) ;
#19559 = CARTESIAN_POINT ( 'NONE',  ( -145.0000000000000568, -189.5512933739568666, -180.0000000000000284 ) ) ;
#19560 = EDGE_CURVE ( 'NONE', #15708, #21709, #7168, .T. ) ;
#19561 = DIRECTION ( 'NONE',  ( 0.000000000000000000, 2.312964634635740689E-15, -1.000000000000000000 ) ) ;
#19562 = DIRECTION ( 'NONE',  ( 0.000000000000000000, 1.836970198721029441E-16, -1.000000000000000000 ) ) ;
#19563 = DIRECTION ( 'NONE',  ( 0.000000000000000000, -1.224646799147353207E-16, 1.000000000000000000 ) ) ;
#19564 = ORIENTED_EDGE ( 'NONE', *, *, #5181, .F. ) ;
#19565 = VERTEX_POINT ( 'NONE', #15538 ) ;
#19566 = VERTEX_POINT ( 'NONE', #21575 ) ;
#19567 = CARTESIAN_POINT ( 'NONE',  ( -345.0000000000000000, -135.0000000000000000, 126.0000000000000000 ) ) ;
#19568 = CARTESIAN_POINT ( 'NONE',  ( -430.0000000000000000, -114.9999999999999858, 126.0000000000000000 ) ) ;
#19569 = EDGE_CURVE ( 'NONE', #7759, #23936, #3774, .T. ) ;
#19570 = CIRCLE ( 'NONE', #30350, 7.999999999999979572 ) ;
#19571 = FACE_OUTER_BOUND ( 'NONE', #18970, .T. ) ;
#19572 = EDGE_CURVE ( 'NONE', #28310, #21537, #27082, .T. ) ;
#19573 = ORIENTED_EDGE ( 'NONE', *, *, #25091, .T. ) ;
#19574 = ORIENTED_EDGE ( 'NONE', *, *, #26275, .T. ) ;
#19575 = LINE ( 'NONE', #6019, #16322 ) ;
#19576 = ORIENTED_EDGE ( 'NONE', *, *, #31183, .F. ) ;
#19577 = VECTOR ( 'NONE', #18348, 1000.000000000000000 ) ;
#19578 = FACE_OUTER_BOUND ( 'NONE', #11659, .T. ) ;
#19579 = FACE_OUTER_BOUND ( 'NONE', #14175, .T. ) ;
#19580 = ORIENTED_EDGE ( 'NONE', *, *, #14028, .T. ) ;
#19581 = ADVANCED_FACE ( 'NONE', ( #29783 ), #32437, .F. ) ;
#19582 = VERTEX_POINT ( 'NONE', #23536 ) ;
#19583 = DIRECTION ( 'NONE',  ( 1.000000000000000000, 0.000000000000000000, -0.000000000000000000 ) ) ;
#19584 = AXIS2_PLACEMENT_3D ( 'NONE', #21021, #20842, #17845 ) ;
#19585 = VECTOR ( 'NONE', #12023, 1000.000000000000000 ) ;
#19586 = CARTESIAN_POINT ( 'NONE',  ( -12.00000000000001066, -32.99999999999997158, -175.0000000000000000 ) ) ;
#19587 = ORIENTED_EDGE ( 'NONE', *, *, #16683, .T. ) ;
#19588 = DIRECTION ( 'NONE',  ( 0.000000000000000000, -1.000000000000000000, -2.132064625830773463E-16 ) ) ;
#19590 = AXIS2_PLACEMENT_3D ( 'NONE', #28823, #25492, #11989 ) ;
#19589 = CARTESIAN_POINT ( 'NONE',  ( -20.02113311122509032, -11.61907005722761532, -67.50000000000000000 ) ) ;
#19591 = CARTESIAN_POINT ( 'NONE',  ( 11.99999999999999645, -115.0000000000000000, 162.9999999999999716 ) ) ;
#19592 = DIRECTION ( 'NONE',  ( -1.000000000000000000, -3.469446951953834515E-18, 0.000000000000000000 ) ) ;
#19593 = ADVANCED_FACE ( 'NONE', ( #29756 ), #34397, .F. ) ;
#19594 = EDGE_CURVE ( 'NONE', #20222, #15134, #32169, .T. ) ;
#19595 = DIRECTION ( 'NONE',  ( -0.000000000000000000, -0.000000000000000000, -1.000000000000000000 ) ) ;
#19596 = DIRECTION ( 'NONE',  ( 0.000000000000000000, 0.000000000000000000, 1.000000000000000000 ) ) ;
#19597 = DIRECTION ( 'NONE',  ( -1.000000000000000000, 0.000000000000000000, -0.000000000000000000 ) ) ;
#19598 = AXIS2_PLACEMENT_3D ( 'NONE', #27286, #27643, #3258 ) ;
#19599 = ORIENTED_EDGE ( 'NONE', *, *, #11078, .F. ) ;
#19600 = CARTESIAN_POINT ( 'NONE',  ( 841.5859286751250465, 1119.151158108397567, 1753.598338701303419 ) ) ;
#19601 = ORIENTED_EDGE ( 'NONE', *, *, #13623, .F. ) ;
#19602 = AXIS2_PLACEMENT_3D ( 'NONE', #16206, #24006, #21175 ) ;
#19603 = ORIENTED_EDGE ( 'NONE', *, *, #22151, .F. ) ;
#19604 = EDGE_CURVE ( 'NONE', #30730, #1893, #10549, .T. ) ;
#19605 = VECTOR ( 'NONE', #22624, 1000.000000000000000 ) ;
#19606 = DIRECTION ( 'NONE',  ( 0.000000000000000000, 0.000000000000000000, 1.000000000000000000 ) ) ;
#19607 = CIRCLE ( 'NONE', #33234, 34.41491905851385269 ) ;
#19608 = DIRECTION ( 'NONE',  ( 0.000000000000000000, 0.000000000000000000, 1.000000000000000000 ) ) ;
#19609 = APPLICATION_PROTOCOL_DEFINITION ( 'draft international standard', 'automotive_design', 1998, #12152 ) ;
#19610 = VERTEX_POINT ( 'NONE', #18746 ) ;
#19611 = DIRECTION ( 'NONE',  ( 0.000000000000000000, 1.224646799147346305E-16, 1.000000000000000000 ) ) ;
#19612 = CARTESIAN_POINT ( 'NONE',  ( -99.95223371984603489, -0.8438318447813536460, -12.47259309357265522 ) ) ;
#19613 = CIRCLE ( 'NONE', #24132, 5.738084889453667792 ) ;
#19614 = EDGE_CURVE ( 'NONE', #29028, #15121, #18217, .T. ) ;
#19615 = EDGE_CURVE ( 'NONE', #19094, #29748, #32600, .T. ) ;
#19616 = ADVANCED_FACE ( 'NONE', ( #10726 ), #18393, .T. ) ;
#19618 = DIRECTION ( 'NONE',  ( -1.000000000000000000, 0.000000000000000000, 0.000000000000000000 ) ) ;
#19617 = LINE ( 'NONE', #30461, #256 ) ;
#19619 = ORIENTED_EDGE ( 'NONE', *, *, #31471, .F. ) ;
#19620 = VERTEX_POINT ( 'NONE', #2697 ) ;
#19621 = PLANE ( 'NONE',  #23667 ) ;
#19622 = EDGE_CURVE ( 'NONE', #29522, #1801, #25367, .T. ) ;
#19623 = CARTESIAN_POINT ( 'NONE',  ( 10.00000000000000000, 2.296212748401288367E-15, 47.49999999999999289 ) ) ;
#19624 = FACE_OUTER_BOUND ( 'NONE', #15392, .T. ) ;
#19625 = FACE_OUTER_BOUND ( 'NONE', #16391, .T. ) ;
#19626 = VERTEX_POINT ( 'NONE', #394 ) ;
#19627 = DIRECTION ( 'NONE',  ( -1.000000000000000000, 0.000000000000000000, 1.848892746611746966E-32 ) ) ;
#19628 = DIRECTION ( 'NONE',  ( 0.000000000000000000, 1.000000000000000000, -0.000000000000000000 ) ) ;
#19629 = LINE ( 'NONE', #11968, #12914 ) ;
#19630 = VERTEX_POINT ( 'NONE', #22277 ) ;
#19631 = AXIS2_PLACEMENT_3D ( 'NONE', #32118, #31767, #8086 ) ;
#19632 = DIRECTION ( 'NONE',  ( 0.000000000000000000, 0.000000000000000000, 1.000000000000000000 ) ) ;
#19633 = CARTESIAN_POINT ( 'NONE',  ( 12.00000000000001066, -109.0000000000000142, 155.0000000000000000 ) ) ;
#19634 = DIRECTION ( 'NONE',  ( -1.000000000000000000, -0.000000000000000000, -0.000000000000000000 ) ) ;
#19635 = CARTESIAN_POINT ( 'NONE',  ( 5.021133111224265200, -11.61907005722761532, -67.50000000000000000 ) ) ;
#19637 = DIRECTION ( 'NONE',  ( 1.000000000000000000, 0.000000000000000000, 0.000000000000000000 ) ) ;
#19636 = DIRECTION ( 'NONE',  ( -1.000000000000000000, 0.000000000000000000, -0.000000000000000000 ) ) ;
#19638 = CIRCLE ( 'NONE', #288, 32.54542015209057126 ) ;
#19639 = UNCERTAINTY_MEASURE_WITH_UNIT (LENGTH_MEASURE( 1.000000000000000082E-05 ), #32474, 'distance_accuracy_value', 'NONE');
#19640 = CARTESIAN_POINT ( 'NONE',  ( -3.660469135640938497E-16, -11.08319859408599228, -28.58839307351527381 ) ) ;
#19641 = VERTEX_POINT ( 'NONE', #6230 ) ;
#19642 = CARTESIAN_POINT ( 'NONE',  ( -35.00000000000000000, 11.30824010203864916, 28.57494248152496397 ) ) ;
#19643 = DIRECTION ( 'NONE',  ( 1.000000000000000000, 0.000000000000000000, 0.000000000000000000 ) ) ;
#19644 = ORIENTED_EDGE ( 'NONE', *, *, #15233, .T. ) ;
#19645 = B_SPLINE_CURVE_WITH_KNOTS ( 'NONE', 3,
 ( #4268, #31843, #9974, #31509 ),
 .UNSPECIFIED., .F., .F.,
 ( 4, 4 ),
 ( 0.005298361175080963312, 0.005985229640890900142 ),
 .UNSPECIFIED. ) ;
#19646 = B_SPLINE_CURVE_WITH_KNOTS ( 'NONE', 3,
 ( #27083, #29234, #2001, #16072 ),
 .UNSPECIFIED., .F., .F.,
 ( 4, 4 ),
 ( 0.0003071994222346450588, 0.0006879348191048121524 ),
 .UNSPECIFIED. ) ;
#19647 = VERTEX_POINT ( 'NONE', #11418 ) ;
#19648 = AXIS2_PLACEMENT_3D ( 'NONE', #20403, #9368, #1693 ) ;
#19649 = VECTOR ( 'NONE', #3276, 1000.000000000000227 ) ;
#19650 = EDGE_LOOP ( 'NONE', ( #24571, #30132 ) ) ;
#19651 = DIRECTION ( 'NONE',  ( 0.000000000000000000, 8.881784197001252323E-16, 1.000000000000000000 ) ) ;
#19652 = ORIENTED_EDGE ( 'NONE', *, *, #4662, .F. ) ;
#19653 = ORIENTED_EDGE ( 'NONE', *, *, #3556, .T. ) ;
#19654 = LINE ( 'NONE', #19472, #15635 ) ;
#19655 = VECTOR ( 'NONE', #4184, 1000.000000000000000 ) ;
#19656 = EDGE_CURVE ( 'NONE', #33286, #24787, #24401, .T. ) ;
#19657 = ADVANCED_FACE ( 'NONE', ( #19270 ), #8561, .F. ) ;
#19658 = ORIENTED_EDGE ( 'NONE', *, *, #7303, .T. ) ;
#19659 = CARTESIAN_POINT ( 'NONE',  ( -418.0000000000000000, 105.0000000000000142, 162.9999999999999716 ) ) ;
#19660 = CARTESIAN_POINT ( 'NONE',  ( 0.000000000000000000, 3.909681563761695067, 30.21863799912385673 ) ) ;
#19661 = ORIENTED_EDGE ( 'NONE', *, *, #1413, .F. ) ;
#19662 = ORIENTED_EDGE ( 'NONE', *, *, #34113, .F. ) ;
#19663 = DIRECTION ( 'NONE',  ( 0.000000000000000000, 1.000000000000000000, 0.000000000000000000 ) ) ;
#19664 = FACE_OUTER_BOUND ( 'NONE', #29630, .T. ) ;
#19665 = VECTOR ( 'NONE', #18762, 1000.000000000000000 ) ;
#19666 = CARTESIAN_POINT ( 'NONE',  ( 102.1109711573756016, -4.971563738489883200, -11.47098163371368251 ) ) ;
#19667 = FACE_OUTER_BOUND ( 'NONE', #13364, .T. ) ;
#19668 = DIRECTION ( 'NONE',  ( 0.000000000000000000, 1.000000000000000000, 0.000000000000000000 ) ) ;
#19669 = ORIENTED_EDGE ( 'NONE', *, *, #7009, .T. ) ;
#19670 = CARTESIAN_POINT ( 'NONE',  ( -35.00000000000000000, 3.353962854566122864, 15.81122994652406355 ) ) ;
#19671 = CARTESIAN_POINT ( 'NONE',  ( 6.857172176539690689, 37.23415287044795718, -36.68877005347593467 ) ) ;
#19672 = ORIENTED_EDGE ( 'NONE', *, *, #23283, .T. ) ;
#19673 = DIRECTION ( 'NONE',  ( 0.6051742151937650194, -0.7960930657056438653, 0.000000000000000000 ) ) ;
#19674 = CARTESIAN_POINT ( 'NONE',  ( -18.38714294329533416, -33.09555747561019245, -36.68877005347593467 ) ) ;
#19675 = CARTESIAN_POINT ( 'NONE',  ( -499.9999999999999432, 140.9999999999999716, 187.0000000000000000 ) ) ;
#19676 = DIRECTION ( 'NONE',  ( 0.000000000000000000, 1.000000000000000000, 5.053935297177146739E-49 ) ) ;
#19677 = SURFACE_STYLE_FILL_AREA ( #14866 ) ;
#19678 = AXIS2_PLACEMENT_3D ( 'NONE', #23761, #18254, #18782 ) ;
#19679 = ORIENTED_EDGE ( 'NONE', *, *, #3853, .T. ) ;
#19681 = CARTESIAN_POINT ( 'NONE',  ( 0.02407890056655651728, -3.506335382740735529, 30.89238256715863784 ) ) ;
#19680 = DIRECTION ( 'NONE',  ( -0.000000000000000000, -0.000000000000000000, 1.000000000000000000 ) ) ;
#19682 = VECTOR ( 'NONE', #27297, 1000.000000000000000 ) ;
#19683 = ORIENTED_EDGE ( 'NONE', *, *, #34646, .F. ) ;
#19684 =( REPRESENTATION_RELATIONSHIP ('NONE','NONE', #23037, #15767 ) REPRESENTATION_RELATIONSHIP_WITH_TRANSFORMATION ( #515 )SHAPE_REPRESENTATION_RELATIONSHIP( ) );
#19685 =( NAMED_UNIT ( * ) SI_UNIT ( $, .STERADIAN. ) SOLID_ANGLE_UNIT ( ) );
#19686 = CARTESIAN_POINT ( 'NONE',  ( 1.532562817202168137, 33.69708579775584667, -36.68877005347592757 ) ) ;
#19687 = CIRCLE ( 'NONE', #13430, 3.999999999999976019 ) ;
#19688 = ORIENTED_EDGE ( 'NONE', *, *, #12944, .T. ) ;
#19689 = AXIS2_PLACEMENT_3D ( 'NONE', #28044, #28402, #9538 ) ;
#19690 = ORIENTED_EDGE ( 'NONE', *, *, #14842, .T. ) ;
#19691 = CARTESIAN_POINT ( 'NONE',  ( 99.26191511054632599, -4.118294838564020743E-16, -7.500000000000000000 ) ) ;
#19692 = ORIENTED_EDGE ( 'NONE', *, *, #22059, .F. ) ;
#19693 = VERTEX_POINT ( 'NONE', #8919 ) ;
#19694 = DIRECTION ( 'NONE',  ( 0.000000000000000000, 0.000000000000000000, -1.000000000000000000 ) ) ;
#19695 = EDGE_CURVE ( 'NONE', #2295, #28456, #19795, .T. ) ;
#19696 = CARTESIAN_POINT ( 'NONE',  ( 2.789999999999999147, -17.84464379609659446, 24.93395722650000934 ) ) ;
#19697 = VECTOR ( 'NONE', #13397, 1000.000000000000000 ) ;
#19698 = EDGE_CURVE ( 'NONE', #18691, #32277, #16600, .T. ) ;
#19699 = CARTESIAN_POINT ( 'NONE',  ( 2.789999999999999147, 24.20451283648857554, -19.51346322004903300 ) ) ;
#19700 = LINE ( 'NONE', #8646, #6868 ) ;
#19701 = ORIENTED_EDGE ( 'NONE', *, *, #17131, .T. ) ;
#19702 = ORIENTED_EDGE ( 'NONE', *, *, #28761, .T. ) ;
#19703 = LINE ( 'NONE', #648, #9977 ) ;
#19704 = LINE ( 'NONE', #3311, #3315 ) ;
#19705 = PRODUCT_RELATED_PRODUCT_CATEGORY ( 'part', '', ( #22286 ) ) ;
#19706 = LINE ( 'NONE', #17406, #23731 ) ;
#19707 = VECTOR ( 'NONE', #6155, 1000.000000000000000 ) ;
#19708 = DIRECTION ( 'NONE',  ( -0.000000000000000000, -0.000000000000000000, 1.000000000000000000 ) ) ;
#19709 = FACE_OUTER_BOUND ( 'NONE', #23094, .T. ) ;
#19710 = CARTESIAN_POINT ( 'NONE',  ( -418.0000000000000000, -105.0000000000000142, 132.0000000000000000 ) ) ;
#19711 = DIRECTION ( 'NONE',  ( 0.000000000000000000, -3.374343856708137958E-53, 1.000000000000000000 ) ) ;
#19712 = ORIENTED_EDGE ( 'NONE', *, *, #27631, .T. ) ;
#19713 = CIRCLE ( 'NONE', #33338, 7.999999999999979572 ) ;
#19714 = FACE_OUTER_BOUND ( 'NONE', #9117, .T. ) ;
#19715 = CARTESIAN_POINT ( 'NONE',  ( -500.0000000000000000, -141.0000000000000000, 162.9999999999999716 ) ) ;
#19716 = CARTESIAN_POINT ( 'NONE',  ( 2.783128938119423079, -0.3206953221638416673, 30.86785892350564708 ) ) ;
#19717 = ORIENTED_EDGE ( 'NONE', *, *, #20295, .T. ) ;
#19718 = LINE ( 'NONE', #318, #33720 ) ;
#19719 = ORIENTED_EDGE ( 'NONE', *, *, #33499, .F. ) ;
#19720 = DIRECTION ( 'NONE',  ( -0.000000000000000000, 1.000000000000000000, -0.000000000000000000 ) ) ;
#19721 = DIRECTION ( 'NONE',  ( 1.000000000000000000, 0.000000000000000000, 0.000000000000000000 ) ) ;
#19722 = VECTOR ( 'NONE', #23166, 1000.000000000000000 ) ;
#19723 = CIRCLE ( 'NONE', #6045, 1.155000000000000027 ) ;
#19724 = ORIENTED_EDGE ( 'NONE', *, *, #8588, .F. ) ;
#19725 = CARTESIAN_POINT ( 'NONE',  ( 2.033589655920501116, 14.91861104533755267, 30.45815716957509167 ) ) ;
#19726 = CARTESIAN_POINT ( 'NONE',  ( -500.0000000000000000, -137.0000000000000000, 155.0000000000000000 ) ) ;
#19727 = DIRECTION ( 'NONE',  ( -0.9766205557100871015, -0.2149704402110223789, -0.000000000000000000 ) ) ;
#19728 = ORIENTED_EDGE ( 'NONE', *, *, #32844, .T. ) ;
#19729 = DIRECTION ( 'NONE',  ( 0.1063910735368947813, -0.9943243633099144718, -3.335902418024520312E-15 ) ) ;
#19730 = CARTESIAN_POINT ( 'NONE',  ( 2.765921099433441999, -29.68817180695669578, -9.232883799364548949 ) ) ;
#19731 = VERTEX_POINT ( 'NONE', #8739 ) ;
#19732 = FACE_OUTER_BOUND ( 'NONE', #13721, .T. ) ;
#19733 = ADVANCED_FACE ( 'NONE', ( #24572 ), #24928, .F. ) ;
#19734 = DIRECTION ( 'NONE',  ( -1.000000000000000000, 0.000000000000000000, 0.000000000000000000 ) ) ;
#19735 = CARTESIAN_POINT ( 'NONE',  ( 0.000000000000000000, -29.69698570178010755, -11.75786841620047163 ) ) ;
#19736 = CARTESIAN_POINT ( 'NONE',  ( -347.0000000000000000, -125.0000000000000284, 126.0000000000000000 ) ) ;
#19737 = ITEM_DEFINED_TRANSFORMATION ( 'NONE', 'NONE', #21795,  #28566 ) ;
#19738 = ORIENTED_EDGE ( 'NONE', *, *, #22711, .T. ) ;
#19739 = ORIENTED_EDGE ( 'NONE', *, *, #26484, .F. ) ;
#19740 = ORIENTED_EDGE ( 'NONE', *, *, #19184, .T. ) ;
#19741 = PRODUCT_DEFINITION_SHAPE ( 'NONE', 'NONE',  #35100 ) ;
#19742 = EDGE_CURVE ( 'NONE', #11336, #22309, #17128, .T. ) ;
#19743 = LINE ( 'NONE', #9226, #3319 ) ;
#19744 = VECTOR ( 'NONE', #20925, 1000.000000000000000 ) ;
#19745 = EDGE_CURVE ( 'NONE', #29922, #1812, #29, .T. ) ;
#19746 = CARTESIAN_POINT ( 'NONE',  ( -499.9999999999999432, -105.0000000000000142, -162.9999999999999716 ) ) ;
#19747 = AXIS2_PLACEMENT_3D ( 'NONE', #4837, #21047, #5364 ) ;
#19748 = AXIS2_PLACEMENT_3D ( 'NONE', #4094, #6601, #19973 ) ;
#19749 = LINE ( 'NONE', #3180, #24120 ) ;
#19750 = DIRECTION ( 'NONE',  ( 1.000000000000000000, 0.000000000000000000, 0.000000000000000000 ) ) ;
#19751 = ORIENTED_EDGE ( 'NONE', *, *, #33928, .T. ) ;
#19752 = EDGE_LOOP ( 'NONE', ( #2075, #9709, #28593, #4176 ) ) ;
#19753 = ADVANCED_FACE ( 'NONE', ( #13918 ), #19621, .F. ) ;
#19754 = CARTESIAN_POINT ( 'NONE',  ( 1.749999999999999778, -33.39989884085096605, 8.296590337300138174 ) ) ;
#19755 = ORIENTED_EDGE ( 'NONE', *, *, #28258, .T. ) ;
#19756 = LINE ( 'NONE', #25245, #5021 ) ;
#19757 = ADVANCED_FACE ( 'NONE', ( #13738 ), #10893, .T. ) ;
#19758 = CARTESIAN_POINT ( 'NONE',  ( -9.978866888775426602, 14.09580098603202636, -87.50000000000000000 ) ) ;
#19759 = ORIENTED_EDGE ( 'NONE', *, *, #11403, .T. ) ;
#19760 = CIRCLE ( 'NONE', #4378, 4.000000000000003553 ) ;
#19761 = ORIENTED_EDGE ( 'NONE', *, *, #28995, .T. ) ;
#19762 = PLANE ( 'NONE',  #11526 ) ;
#19763 = VERTEX_POINT ( 'NONE', #32589 ) ;
#19764 = DIRECTION ( 'NONE',  ( 0.000000000000000000, -1.000000000000000000, 0.000000000000000000 ) ) ;
#19765 = FILL_AREA_STYLE_COLOUR ( '', #23981 ) ;
#19766 = DIRECTION ( 'NONE',  ( 0.000000000000000000, 0.000000000000000000, 1.000000000000000000 ) ) ;
#19767 = CARTESIAN_POINT ( 'NONE',  ( 12.73347502555019162, -33.69708579775584667, 68.31122994652405112 ) ) ;
#19768 = CIRCLE ( 'NONE', #33203, 4.000000000000003553 ) ;
#19769 = CARTESIAN_POINT ( 'NONE',  ( -100.1500607241188021, -1.660053020383221778, 12.39330379916376224 ) ) ;
#19770 = CARTESIAN_POINT ( 'NONE',  ( 2.265105867312950938, 31.31301644755038538, -11.56311898902712976 ) ) ;
#19771 = CARTESIAN_POINT ( 'NONE',  ( -410.0000000000000568, 113.0000000000000000, -175.0000000000000000 ) ) ;
#19772 = EDGE_LOOP ( 'NONE', ( #18768, #20918, #32881, #21060 ) ) ;
#19773 = VECTOR ( 'NONE', #15915, 1000.000000000000000 ) ;
#19774 = AXIS2_PLACEMENT_3D ( 'NONE', #6031, #10864, #22248 ) ;
#19775 = VERTEX_POINT ( 'NONE', #8210 ) ;
#19776 = CARTESIAN_POINT ( 'NONE',  ( 851.2675110943097252, 1028.667690325297599, 1753.598338701303419 ) ) ;
#19777 = ORIENTED_EDGE ( 'NONE', *, *, #32189, .T. ) ;
#19778 = ORIENTED_EDGE ( 'NONE', *, *, #222, .T. ) ;
#19779 = AXIS2_PLACEMENT_3D ( 'NONE', #6847, #23248, #9703 ) ;
#19780 = CARTESIAN_POINT ( 'NONE',  ( 2.265105904191462738, 13.50646231473634451, 30.52517305359789646 ) ) ;
#19781 = CARTESIAN_POINT ( 'NONE',  ( -442.0000000000000000, 104.9999999999999858, -155.0000000000000000 ) ) ;
#19782 = APPLICATION_PROTOCOL_DEFINITION ( 'draft international standard', 'automotive_design', 1998, #27146 ) ;
#19783 = ORIENTED_EDGE ( 'NONE', *, *, #16755, .F. ) ;
#19784 = CARTESIAN_POINT ( 'NONE',  ( -9.978866888775527855, 4.168562732279007754, -87.50000000000000000 ) ) ;
#19785 = CARTESIAN_POINT ( 'NONE',  ( -99.92679314812558289, -0.6743631657302385785, -12.48293875069316528 ) ) ;
#19786 = EDGE_CURVE ( 'NONE', #17680, #12453, #16960, .T. ) ;
#19787 = CONTEXT_DEPENDENT_SHAPE_REPRESENTATION ( #10359, #15871 ) ;
#19789 = CARTESIAN_POINT ( 'NONE',  ( -418.0000000000000000, 141.0000000000000000, -175.0000000000000000 ) ) ;
#19788 = CARTESIAN_POINT ( 'NONE',  ( -12.00000000000001066, -28.99999999999999645, -154.9999999999999716 ) ) ;
#19790 = AXIS2_PLACEMENT_3D ( 'NONE', #18387, #26028, #12872 ) ;
#19791 = ORIENTED_EDGE ( 'NONE', *, *, #29582, .F. ) ;
#19792 = EDGE_LOOP ( 'NONE', ( #5748, #13660, #25867, #31435, #8631, #29217 ) ) ;
#19793 = ADVANCED_FACE ( 'NONE', ( #27784 ), #5529, .F. ) ;
#19794 = EDGE_CURVE ( 'NONE', #18985, #27567, #14277, .T. ) ;
#19795 = LINE ( 'NONE', #29936, #29366 ) ;
#19796 = FACE_OUTER_BOUND ( 'NONE', #2136, .T. ) ;
#19797 = CARTESIAN_POINT ( 'NONE',  ( -414.0000000000000568, 105.0000000000000142, 162.9999999999999716 ) ) ;
#19798 = FACE_OUTER_BOUND ( 'NONE', #3378, .T. ) ;
#19799 = EDGE_LOOP ( 'NONE', ( #3817, #1044, #12392, #5575 ) ) ;
#19801 = LINE ( 'NONE', #30649, #21490 ) ;
#19800 = AXIS2_PLACEMENT_3D ( 'NONE', #30820, #3575, #11795 ) ;
#19803 = DIRECTION ( 'NONE',  ( 0.000000000000000000, 0.000000000000000000, -1.000000000000000000 ) ) ;
#19802 = AXIS2_PLACEMENT_3D ( 'NONE', #23150, #20816, #15314 ) ;
#19804 = DIRECTION ( 'NONE',  ( -1.000000000000000000, -0.000000000000000000, -0.000000000000000000 ) ) ;
#19805 = ORIENTED_EDGE ( 'NONE', *, *, #31144, .T. ) ;
#19806 = DIRECTION ( 'NONE',  ( 1.000000000000000000, 0.000000000000000000, 1.300283923313630633E-47 ) ) ;
#19807 = PLANE ( 'NONE',  #26781 ) ;
#19808 = EDGE_CURVE ( 'NONE', #34124, #32414, #21923, .T. ) ;
#19809 = CARTESIAN_POINT ( 'NONE',  ( 2.790000000000000924, 12.80000000000000071, 3.000000000000000000 ) ) ;
#19810 = AXIS2_PLACEMENT_3D ( 'NONE', #17271, #25424, #11921 ) ;
#19812 = DIRECTION ( 'NONE',  ( 0.000000000000000000, -0.8486862100397269959, 0.5288966977476833309 ) ) ;
#19811 = DIRECTION ( 'NONE',  ( 0.000000000000000000, -1.000000000000000000, -0.000000000000000000 ) ) ;
#19813 = DIRECTION ( 'NONE',  ( 0.000000000000000000, 1.310824597558155437E-49, 1.000000000000000000 ) ) ;
#19814 = ORIENTED_EDGE ( 'NONE', *, *, #6539, .F. ) ;
#19815 = DIRECTION ( 'NONE',  ( -1.000000000000000000, 0.000000000000000000, 0.000000000000000000 ) ) ;
#19816 = CARTESIAN_POINT ( 'NONE',  ( -4.875000000000000000, -1.866624223957557671, 0.000000000000000000 ) ) ;
#19817 = EDGE_CURVE ( 'NONE', #22594, #9350, #15145, .T. ) ;
#19818 = EDGE_CURVE ( 'NONE', #30600, #24075, #23132, .T. ) ;
#19819 = AXIS2_PLACEMENT_3D ( 'NONE', #10316, #21176, #12831 ) ;
#19820 = VERTEX_POINT ( 'NONE', #16781 ) ;
#19821 = SHAPE_REPRESENTATION ( 'angular contact ball bearing_68_iso_ISO 15 ABB - 5820 - Full,SI,NC,Full_68', ( #28566 ), #17234 ) ;
#19822 =( LENGTH_UNIT ( ) NAMED_UNIT ( * ) SI_UNIT ( .MILLI., .METRE. ) );
#19823 = EDGE_CURVE ( 'NONE', #16210, #26021, #23162, .T. ) ;
#19824 = ORIENTED_EDGE ( 'NONE', *, *, #18665, .F. ) ;
#19825 = AXIS2_PLACEMENT_3D ( 'NONE', #34119, #31625, #1210 ) ;
#19826 = ORIENTED_EDGE ( 'NONE', *, *, #9797, .T. ) ;
#19827 = CARTESIAN_POINT ( 'NONE',  ( 2.789999999999999147, -3.728217946243117087, 30.24156218513554606 ) ) ;
#19828 = EDGE_LOOP ( 'NONE', ( #14804, #15997, #23011, #6183 ) ) ;
#19829 = ORIENTED_EDGE ( 'NONE', *, *, #5193, .T. ) ;
#19830 = DIRECTION ( 'NONE',  ( -1.000000000000000000, 0.000000000000000000, 0.000000000000000000 ) ) ;
#19831 = AXIS2_PLACEMENT_3D ( 'NONE', #14013, #22553, #17411 ) ;
#19832 = CONTEXT_DEPENDENT_SHAPE_REPRESENTATION ( #23116, #1227 ) ;
#19833 = ORIENTED_EDGE ( 'NONE', *, *, #28653, .F. ) ;
#19834 = CARTESIAN_POINT ( 'NONE',  ( -15.99999999999998579, 75.55999999999990280, 172.9900000000000091 ) ) ;
#19835 = CARTESIAN_POINT ( 'NONE',  ( -445.9999999999999432, 137.0000000000000000, -155.0000000000000000 ) ) ;
#19836 = EDGE_LOOP ( 'NONE', ( #31991, #23867, #2060, #13526 ) ) ;
#19837 = ORIENTED_EDGE ( 'NONE', *, *, #4722, .T. ) ;
#19838 = EDGE_CURVE ( 'NONE', #20533, #10877, #6592, .T. ) ;
#19839 = PLANE ( 'NONE',  #6587 ) ;
#19840 = PLANE ( 'NONE',  #14112 ) ;
#19841 = PLANE ( 'NONE',  #28946 ) ;
#19842 = CARTESIAN_POINT ( 'NONE',  ( 28.23027531293552528, -10.15143121711728469, 0.000000000000000000 ) ) ;
#19843 = DIRECTION ( 'NONE',  ( 0.000000000000000000, 1.000000000000000000, 1.310824597558155437E-49 ) ) ;
#19844 = ORIENTED_EDGE ( 'NONE', *, *, #31402, .F. ) ;
#19845 = CARTESIAN_POINT ( 'NONE',  ( 21.24400529595486020, -24.65555945140047811, 68.31122994652405112 ) ) ;
#19846 = AXIS2_PLACEMENT_3D ( 'NONE', #9016, #30556, #27696 ) ;
#19847 = CARTESIAN_POINT ( 'NONE',  ( 0.02407890056655608360, -27.96208973699893008, -13.59246946040217630 ) ) ;
#19848 = EDGE_LOOP ( 'NONE', ( #23503, #19692, #4365, #2742, #3271, #11436, #11400, #9739 ) ) ;
#19849 = DIRECTION ( 'NONE',  ( 0.9635499925192231307, 0.2675283385292199223, -0.000000000000000000 ) ) ;
#19850 = DIRECTION ( 'NONE',  ( -1.000000000000000000, 0.000000000000000000, 0.000000000000000000 ) ) ;
#19851 = CARTESIAN_POINT ( 'NONE',  ( 3.235562306570555532E-30, -11.61907005722761532, -67.50000000000000000 ) ) ;
#19852 = CARTESIAN_POINT ( 'NONE',  ( 99.26191511054634020, 0.3991779689724688773, -7.500000000000000000 ) ) ;
#19853 = CYLINDRICAL_SURFACE ( 'NONE', #7105, 34.41491905851385269 ) ;
#19854 = CONICAL_SURFACE ( 'NONE', #9018, 2.499999999999825473, 0.7853981633974538301 ) ;
#19855 = CARTESIAN_POINT ( 'NONE',  ( -35.55956070192387841, -32.65143121711728469, 10.00000000000000000 ) ) ;
#19856 = EDGE_LOOP ( 'NONE', ( #17277, #22400 ) ) ;
#19857 = DIRECTION ( 'NONE',  ( 1.000000000000000000, 0.000000000000000000, 0.000000000000000000 ) ) ;
#19859 = CARTESIAN_POINT ( 'NONE',  ( -361.0000000000000000, -125.0000000000000284, 130.0000000000000000 ) ) ;
#19858 = CARTESIAN_POINT ( 'NONE',  ( -445.9999999999999432, -125.0000000000000000, -101.9999999999999858 ) ) ;
#19860 = VECTOR ( 'NONE', #16836, 1000.000000000000000 ) ;
#19861 = EDGE_CURVE ( 'NONE', #11184, #6968, #1610, .T. ) ;
#19862 = EDGE_CURVE ( 'NONE', #32966, #4316, #31330, .T. ) ;
#19863 = ORIENTED_EDGE ( 'NONE', *, *, #415, .T. ) ;
#19864 = FACE_OUTER_BOUND ( 'NONE', #25467, .T. ) ;
#19865 = DIRECTION ( 'NONE',  ( -0.000000000000000000, -0.000000000000000000, 1.000000000000000000 ) ) ;
#19866 = ORIENTED_EDGE ( 'NONE', *, *, #9937, .T. ) ;
#19867 = ORIENTED_EDGE ( 'NONE', *, *, #28085, .T. ) ;
#19868 = VECTOR ( 'NONE', #34046, 1000.000000000000000 ) ;
#19869 = EDGE_CURVE ( 'NONE', #21129, #20981, #28491, .T. ) ;
#19870 = ORIENTED_EDGE ( 'NONE', *, *, #13051, .T. ) ;
#19871 = CARTESIAN_POINT ( 'NONE',  ( 109.2847039433696779, -3.833500081834649187, -6.453260708061876905 ) ) ;
#19872 = VERTEX_POINT ( 'NONE', #9273 ) ;
#19873 = ORIENTED_EDGE ( 'NONE', *, *, #3932, .T. ) ;
#19874 = CARTESIAN_POINT ( 'NONE',  ( 0.000000000000000000, -11.69134295108990607, 6.750000000000024869 ) ) ;
#19875 = DIRECTION ( 'NONE',  ( -1.000000000000000000, 6.792721752314501023E-48, -3.697785493223492838E-32 ) ) ;
#19876 = AXIS2_PLACEMENT_3D ( 'NONE', #34742, #26549, #20225 ) ;
#19877 = LINE ( 'NONE', #7017, #2623 ) ;
#19878 = DIRECTION ( 'NONE',  ( 0.000000000000000000, 0.000000000000000000, 1.000000000000000000 ) ) ;
#19879 = EDGE_LOOP ( 'NONE', ( #7852, #10615, #20314, #6544 ) ) ;
#19880 = ORIENTED_EDGE ( 'NONE', *, *, #3696, .F. ) ;
#19881 = CARTESIAN_POINT ( 'NONE',  ( 0.000000000000000000, 28.95078156989558948, 9.502838467758177643 ) ) ;
#19882 = CARTESIAN_POINT ( 'NONE',  ( 3.235562306570555532E-30, 1.325223266901699007E-14, -67.50000000000000000 ) ) ;
#19883 = CARTESIAN_POINT ( 'NONE',  ( -349.0000000000000000, 124.9999999999999432, 185.0000000000000000 ) ) ;
#19884 = CARTESIAN_POINT ( 'NONE',  ( -12.00000000000001066, -137.0000000000000000, 155.0000000000000000 ) ) ;
#19885 = CARTESIAN_POINT ( 'NONE',  ( -418.0000000000000000, 124.9999999999999574, -187.0000000000000000 ) ) ;
#19886 = DIRECTION ( 'NONE',  ( 0.000000000000000000, 0.000000000000000000, -1.000000000000000000 ) ) ;
#19887 = DIRECTION ( 'NONE',  ( 0.000000000000000000, 1.000000000000000000, 1.224646799147353207E-16 ) ) ;
#19888 = EDGE_LOOP ( 'NONE', ( #16484, #24112, #4817, #4463 ) ) ;
#19889 = EDGE_CURVE ( 'NONE', #29292, #31361, #10029, .T. ) ;
#19890 = DIRECTION ( 'NONE',  ( 1.000000000000000000, 3.040835319149746090E-31, 1.232595164407830946E-32 ) ) ;
#19891 = CARTESIAN_POINT ( 'NONE',  ( 0.1835381996566693985, 29.53850320881163682, -12.99634918694980357 ) ) ;
#19892 = CARTESIAN_POINT ( 'NONE',  ( -2.216215597024039141, -32.46987467335852529, 68.31122994652405112 ) ) ;
#19893 = VERTEX_POINT ( 'NONE', #28323 ) ;
#19894 =( REPRESENTATION_RELATIONSHIP ('NONE','NONE', #23037, #15767 ) REPRESENTATION_RELATIONSHIP_WITH_TRANSFORMATION ( #30802 )SHAPE_REPRESENTATION_RELATIONSHIP( ) );
#19895 = CYLINDRICAL_SURFACE ( 'NONE', #25171, 7.999999999999979572 ) ;
#19896 = ORIENTED_EDGE ( 'NONE', *, *, #19502, .F. ) ;
#19897 = DIRECTION ( 'NONE',  ( 0.000000000000000000, -1.000000000000000000, 6.123233995736766036E-17 ) ) ;
#19898 = CARTESIAN_POINT ( 'NONE',  ( -36.04853892210773836, 11.59936550071286376, 68.31122994652405112 ) ) ;
#19899 = EDGE_CURVE ( 'NONE', #5382, #9264, #14027, .T. ) ;
#19900 = EDGE_CURVE ( 'NONE', #13768, #21081, #29924, .T. ) ;
#19901 = EDGE_CURVE ( 'NONE', #24976, #6398, #4087, .T. ) ;
#19902 = ORIENTED_EDGE ( 'NONE', *, *, #7865, .F. ) ;
#19903 = DIRECTION ( 'NONE',  ( 5.546364386991661285E-52, 0.000000000000000000, 1.000000000000000000 ) ) ;
#19904 = FACE_OUTER_BOUND ( 'NONE', #10267, .T. ) ;
#19905 = LINE ( 'NONE', #26405, #5798 ) ;
#19906 = PRODUCT_DEFINITION_SHAPE ( 'NONE', 'NONE',  #35245 ) ;
#19907 = ORIENTED_EDGE ( 'NONE', *, *, #10276, .F. ) ;
#19908 = CARTESIAN_POINT ( 'NONE',  ( 828.4466382490892329, 1241.950150099747361, 1753.598338701303419 ) ) ;
#19909 = FACE_OUTER_BOUND ( 'NONE', #22573, .T. ) ;
#19910 = ORIENTED_EDGE ( 'NONE', *, *, #6533, .F. ) ;
#19911 = CARTESIAN_POINT ( 'NONE',  ( 19.99999999999996092, -134.9999999999999716, 162.9999999999999716 ) ) ;
#19912 = CARTESIAN_POINT ( 'NONE',  ( -361.0000000000000000, -125.0000000000000284, 164.9999999999999716 ) ) ;
#19913 = DIRECTION ( 'NONE',  ( -0.000000000000000000, 1.000000000000000000, -0.000000000000000000 ) ) ;
#19914 = CARTESIAN_POINT ( 'NONE',  ( 2.789999999999999591, 27.83606077057228489, 12.85640846290669970 ) ) ;
#19915 = EDGE_LOOP ( 'NONE', ( #15873, #29340, #28858 ) ) ;
#19916 = EDGE_LOOP ( 'NONE', ( #21028, #4791, #9242, #3862, #5612, #29543, #6914, #32696 ) ) ;
#19917 = ORIENTED_EDGE ( 'NONE', *, *, #31452, .F. ) ;
#19918 = CARTESIAN_POINT ( 'NONE',  ( -449.9999999999999432, -125.0000000000000000, 107.9999999999999858 ) ) ;
#19919 = CARTESIAN_POINT ( 'NONE',  ( 2.790000000000080860, -23.48523522029045196, -19.71414358107291420 ) ) ;
#19920 = CARTESIAN_POINT ( 'NONE',  ( -37.12776225901827587, -7.411627343331159246, 68.31122994652405112 ) ) ;
#19921 = ORIENTED_EDGE ( 'NONE', *, *, #6250, .F. ) ;
#19922 = ORIENTED_EDGE ( 'NONE', *, *, #22, .T. ) ;
#19923 = DIRECTION ( 'NONE',  ( 1.000000000000000000, 0.000000000000000000, 0.000000000000000000 ) ) ;
#19924 = DIRECTION ( 'NONE',  ( -0.4684084406997904848, 0.8835120444460226041, 0.000000000000000000 ) ) ;
#19925 = VERTEX_POINT ( 'NONE', #30990 ) ;
#19926 = PLANE ( 'NONE',  #18698 ) ;
#19927 = CARTESIAN_POINT ( 'NONE',  ( 0.02407890056655608360, 29.44518845714779332, -9.980709654879110104 ) ) ;
#19928 = ORIENTED_EDGE ( 'NONE', *, *, #10572, .F. ) ;
#19929 = VECTOR ( 'NONE', #27072, 1000.000000000000227 ) ;
#19930 = ORIENTED_EDGE ( 'NONE', *, *, #25463, .T. ) ;
#19931 =( NAMED_UNIT ( * ) SI_UNIT ( $, .STERADIAN. ) SOLID_ANGLE_UNIT ( ) );
#19932 = EDGE_CURVE ( 'NONE', #11236, #31513, #8885, .T. ) ;
#19933 = CARTESIAN_POINT ( 'NONE',  ( -20.00000000000007461, 144.9999999999999716, -162.9999999999999716 ) ) ;
#19934 = EDGE_LOOP ( 'NONE', ( #453, #10855, #12990, #28598, #31017, #33445 ) ) ;
#19935 = DIRECTION ( 'NONE',  ( 0.9635499925192227977, -0.2675283385292215321, -4.914415851915309929E-17 ) ) ;
#19936 = EDGE_CURVE ( 'NONE', #904, #27132, #12311, .T. ) ;
#19937 = CARTESIAN_POINT ( 'NONE',  ( 32.05156013847309993, -20.15193397489277771, 68.31122994652405112 ) ) ;
#19938 = EDGE_CURVE ( 'NONE', #8857, #15892, #30813, .T. ) ;
#19939 = AXIS2_PLACEMENT_3D ( 'NONE', #19920, #28095, #6893 ) ;
#19940 = CARTESIAN_POINT ( 'NONE',  ( -100.0520116554321390, -1.339152422118498498, 12.43243648734289408 ) ) ;
#19941 = CARTESIAN_POINT ( 'NONE',  ( -12.00000000000003908, -134.9999999999999716, -186.9999999999999716 ) ) ;
#19943 = ADVANCED_FACE ( 'NONE', ( #6767 ), #6937, .F. ) ;
#19942 = CARTESIAN_POINT ( 'NONE',  ( -442.0000000000000000, 105.0000000000000142, 187.0000000000000000 ) ) ;
#19944 = VERTEX_POINT ( 'NONE', #23326 ) ;
#19945 = ORIENTED_EDGE ( 'NONE', *, *, #16119, .F. ) ;
#19946 = CARTESIAN_POINT ( 'NONE',  ( 827.7550966477188013, 1248.413254941397554, 1753.598338701303419 ) ) ;
#19947 = CIRCLE ( 'NONE', #29616, 22.50000000000000355 ) ;
#19948 = ORIENTED_EDGE ( 'NONE', *, *, #18471, .T. ) ;
#19949 = ORIENTED_EDGE ( 'NONE', *, *, #4086, .F. ) ;
#19950 = ADVANCED_FACE ( 'NONE', ( #34173 ), #25286, .T. ) ;
#19951 = TOROIDAL_SURFACE ( 'NONE', #10845, 30.47050528711511674, 8.000000000000000000 ) ;
#19952 = DIRECTION ( 'NONE',  ( 0.000000000000000000, 0.000000000000000000, -1.000000000000000000 ) ) ;
#19953 = DIRECTION ( 'NONE',  ( 0.000000000000000000, 0.000000000000000000, 1.000000000000000000 ) ) ;
#19954 = ORIENTED_EDGE ( 'NONE', *, *, #325, .F. ) ;
#19955 = DIRECTION ( 'NONE',  ( 0.6876994588534230957, 0.7259954919231310644, 0.000000000000000000 ) ) ;
#19956 = CARTESIAN_POINT ( 'NONE',  ( -105.6714549178013840, -5.082150419746904291, -11.42046709103397895 ) ) ;
#19958 = DIRECTION ( 'NONE',  ( 1.000000000000000000, 3.040835319149746090E-31, 1.232595164407830946E-32 ) ) ;
#19957 = LINE ( 'NONE', #22099, #10499 ) ;
#19960 = ORIENTED_EDGE ( 'NONE', *, *, #24314, .F. ) ;
#19959 = AXIS2_PLACEMENT_3D ( 'NONE', #10730, #10554, #24234 ) ;
#19961 = VERTEX_POINT ( 'NONE', #1091 ) ;
#19962 = CARTESIAN_POINT ( 'NONE',  ( -12.00000000000001066, -124.9999999999999432, -190.9999999999999432 ) ) ;
#19963 = AXIS2_PLACEMENT_3D ( 'NONE', #27314, #14657, #1457 ) ;
#19964 = VECTOR ( 'NONE', #31948, 1000.000000000000000 ) ;
#19965 = PLANE ( 'NONE',  #19328 ) ;
#19966 = CARTESIAN_POINT ( 'NONE',  ( 5.510910596163087978E-15, 45.00000000000000711, -36.68877005347593467 ) ) ;
#19967 = CARTESIAN_POINT ( 'NONE',  ( 5.021133111224162171, -25.61315202898006049, -67.50000000000000000 ) ) ;
#19968 = VERTEX_POINT ( 'NONE', #33653 ) ;
#19969 = FACE_OUTER_BOUND ( 'NONE', #22772, .T. ) ;
#19970 = CARTESIAN_POINT ( 'NONE',  ( 0.5344654698445916452, 9.073918974790291969, 11.28351131189991108 ) ) ;
#19971 = ORIENTED_EDGE ( 'NONE', *, *, #8826, .F. ) ;
#19972 = AXIS2_PLACEMENT_3D ( 'NONE', #8214, #29942, #13922 ) ;
#19973 = DIRECTION ( 'NONE',  ( 0.000000000000000000, 0.000000000000000000, -1.000000000000000000 ) ) ;
#19974 = CARTESIAN_POINT ( 'NONE',  ( 19.99999999999998224, 134.9999999999999432, -186.9999999999999716 ) ) ;
#19975 = AXIS2_PLACEMENT_3D ( 'NONE', #27648, #5921, #11995 ) ;
#19976 = DIRECTION ( 'NONE',  ( 0.3701381553399144542, 0.9289767198167914186, 1.706502549609061988E-16 ) ) ;
#19978 = CARTESIAN_POINT ( 'NONE',  ( -35.00000000000000000, -4.831299144296466785, 15.81122994652406355 ) ) ;
#19977 = CARTESIAN_POINT ( 'NONE',  ( 2.765921099433442443, 30.61125888652961891, 5.439165181699118889 ) ) ;
#19979 = FACE_OUTER_BOUND ( 'NONE', #12179, .T. ) ;
#19980 = FACE_OUTER_BOUND ( 'NONE', #4248, .T. ) ;
#19981 = VERTEX_POINT ( 'NONE', #18010 ) ;
#19982 = DIRECTION ( 'NONE',  ( 0.000000000000000000, 0.000000000000000000, -1.000000000000000000 ) ) ;
#19984 = EDGE_CURVE ( 'NONE', #8292, #18383, #3569, .T. ) ;
#19983 = CARTESIAN_POINT ( 'NONE',  ( -8.373597507930047958E-14, 11.49192876466713287, 28.42779197342015607 ) ) ;
#19985 = PRODUCT_DEFINITION_SHAPE ( 'NONE', 'NONE',  #35181 ) ;
#19986 = EDGE_CURVE ( 'NONE', #2032, #30341, #22636, .T. ) ;
#19987 = VERTEX_POINT ( 'NONE', #17313 ) ;
#19988 = VECTOR ( 'NONE', #28670, 1000.000000000000114 ) ;
#19989 = EDGE_CURVE ( 'NONE', #17757, #20342, #28142, .T. ) ;
#19990 = EDGE_CURVE ( 'NONE', #21780, #17552, #22804, .T. ) ;
#19991 = VECTOR ( 'NONE', #10868, 1000.000000000000000 ) ;
#19992 = VECTOR ( 'NONE', #14526, 1000.000000000000000 ) ;
#19993 = AXIS2_PLACEMENT_3D ( 'NONE', #26349, #12665, #17840 ) ;
#19994 = ORIENTED_EDGE ( 'NONE', *, *, #3557, .T. ) ;
#19995 = ORIENTED_EDGE ( 'NONE', *, *, #4582, .T. ) ;
#19996 = DIRECTION ( 'NONE',  ( 0.000000000000000000, 1.000000000000000000, 0.000000000000000000 ) ) ;
#19997 = ORIENTED_EDGE ( 'NONE', *, *, #3857, .T. ) ;
#19998 = VERTEX_POINT ( 'NONE', #4786 ) ;
#19999 = PLANE ( 'NONE',  #30995 ) ;
#20000 = EDGE_CURVE ( 'NONE', #14902, #13361, #34704, .T. ) ;
#20001 = CIRCLE ( 'NONE', #1219, 2.525000000000001243 ) ;
#20002 = CONTEXT_DEPENDENT_SHAPE_REPRESENTATION ( #17419, #12040 ) ;
#20003 = ORIENTED_EDGE ( 'NONE', *, *, #21135, .T. ) ;
#20004 = CARTESIAN_POINT ( 'NONE',  ( -363.0000000000000000, -125.0000000000000284, 114.0000000000000000 ) ) ;
#20005 = CARTESIAN_POINT ( 'NONE',  ( 0.02407890056655608360, 29.44518845714779332, -9.980709654879110104 ) ) ;
#20006 = VERTEX_POINT ( 'NONE', #28833 ) ;
#20007 = ORIENTED_EDGE ( 'NONE', *, *, #7358, .F. ) ;
#20008 = CARTESIAN_POINT ( 'NONE',  ( -12.00000000000001066, 144.9999999999999716, -186.9999999999999716 ) ) ;
#20009 = CARTESIAN_POINT ( 'NONE',  ( 35.63428259149704758, -12.79065496477508823, 68.31122994652405112 ) ) ;
#20010 = DIRECTION ( 'NONE',  ( -0.000000000000000000, 1.131431318426415506E-52, 1.000000000000000000 ) ) ;
#20011 = CARTESIAN_POINT ( 'NONE',  ( 2.790000000000000924, 0.000000000000000000, 0.000000000000000000 ) ) ;
#20012 = FACE_BOUND ( 'NONE', #1557, .T. ) ;
#20013 = ORIENTED_EDGE ( 'NONE', *, *, #30645, .T. ) ;
#20014 = AXIS2_PLACEMENT_3D ( 'NONE', #23142, #25970, #30968 ) ;
#20015 = EDGE_CURVE ( 'NONE', #21709, #15708, #14050, .T. ) ;
#20016 = DIRECTION ( 'NONE',  ( -0.000000000000000000, 1.000000000000000000, -0.000000000000000000 ) ) ;
#20017 = EDGE_CURVE ( 'NONE', #10008, #9180, #11775, .T. ) ;
#20018 = LINE ( 'NONE', #22153, #33483 ) ;
#20019 = ORIENTED_EDGE ( 'NONE', *, *, #1990, .T. ) ;
#20020 = VECTOR ( 'NONE', #7791, 1000.000000000000000 ) ;
#20021 = TOROIDAL_SURFACE ( 'NONE', #24530, 15.69999999999999929, 0.3000000000000007661 ) ;
#20022 = VECTOR ( 'NONE', #7428, 1000.000000000000000 ) ;
#20023 = LINE ( 'NONE', #1147, #2578 ) ;
#20024 = DIRECTION ( 'NONE',  ( 0.000000000000000000, 0.000000000000000000, 1.000000000000000000 ) ) ;
#20025 = DIRECTION ( 'NONE',  ( 0.000000000000000000, 0.000000000000000000, 1.000000000000000000 ) ) ;
#20026 = DIRECTION ( 'NONE',  ( 0.000000000000000000, 1.000000000000000000, 2.465190328815662439E-32 ) ) ;
#20027 = FACE_OUTER_BOUND ( 'NONE', #3966, .T. ) ;
#20028 = CARTESIAN_POINT ( 'NONE',  ( -445.9999999999999432, -105.0000000000000142, 187.0000000000000000 ) ) ;
#20029 = ORIENTED_EDGE ( 'NONE', *, *, #16765, .F. ) ;
#20030 = DIRECTION ( 'NONE',  ( -1.000000000000000000, 0.000000000000000000, -0.000000000000000000 ) ) ;
#20032 = CARTESIAN_POINT ( 'NONE',  ( 19.99999999999998934, -137.0000000000000000, 155.0000000000000000 ) ) ;
#20031 = DIRECTION ( 'NONE',  ( 0.000000000000000000, 0.000000000000000000, 1.000000000000000000 ) ) ;
#20033 = ORIENTED_EDGE ( 'NONE', *, *, #10117, .T. ) ;
#20034 = EDGE_CURVE ( 'NONE', #1172, #4776, #24191, .T. ) ;
#20035 = EDGE_CURVE ( 'NONE', #13424, #33264, #18535, .T. ) ;
#20036 = PRODUCT_DEFINITION_SHAPE ( 'NONE', 'NONE',  #35104 ) ;
#20037 = CLOSED_SHELL ( 'NONE', ( #9084, #22386, #23184, #6852, #14439, #7391, #27632, #7837, #25016, #1499, #22603, #17239, #7683, #21123, #7694, #14789, #19347, #7957 ) ) ;
#20038 = PLANE ( 'NONE',  #8025 ) ;
#20039 = EDGE_LOOP ( 'NONE', ( #25202, #32841, #7612, #34086 ) ) ;
#20040 = EDGE_CURVE ( 'NONE', #802, #5820, #31671, .T. ) ;
#20041 = ORIENTED_EDGE ( 'NONE', *, *, #7540, .F. ) ;
#20042 = AXIS2_PLACEMENT_3D ( 'NONE', #13420, #5725, #27105 ) ;
#20043 = AXIS2_PLACEMENT_3D ( 'NONE', #10069, #31772, #7378 ) ;
#20044 = AXIS2_PLACEMENT_3D ( 'NONE', #2760, #10959, #34826 ) ;
#20045 = ORIENTED_EDGE ( 'NONE', *, *, #7152, .F. ) ;
#20046 = CARTESIAN_POINT ( 'NONE',  ( 37.55078559520313775, -4.831299144296470338, 68.31122994652405112 ) ) ;
#20047 = EDGE_LOOP ( 'NONE', ( #31460, #13673, #28363, #31371 ) ) ;
#20048 = VERTEX_POINT ( 'NONE', #2478 ) ;
#20049 = CARTESIAN_POINT ( 'NONE',  ( -5.210000000000000853, 0.000000000000000000, 0.000000000000000000 ) ) ;
#20050 = DIRECTION ( 'NONE',  ( -0.000000000000000000, 1.000000000000000000, -0.000000000000000000 ) ) ;
#20051 = CARTESIAN_POINT ( 'NONE',  ( -361.0000000000000000, -125.0000000000000284, 183.0000000000000000 ) ) ;
#20052 = CARTESIAN_POINT ( 'NONE',  ( 3.235562306570555532E-30, -11.61907005722761532, -67.50000000000000000 ) ) ;
#20053 = ORIENTED_EDGE ( 'NONE', *, *, #5554, .F. ) ;
#20054 = ORIENTED_EDGE ( 'NONE', *, *, #9535, .T. ) ;
#20055 = CARTESIAN_POINT ( 'NONE',  ( -449.9999999999999432, -125.0000000000000000, -101.9999999999999858 ) ) ;
#20056 = DIRECTION ( 'NONE',  ( 0.2675283385292205884, -0.9635499925192231307, -1.770012621235684308E-16 ) ) ;
#20057 = LINE ( 'NONE', #11694, #34374 ) ;
#20058 = LINE ( 'NONE', #25911, #34027 ) ;
#20059 = CARTESIAN_POINT ( 'NONE',  ( -445.9999999999999432, -112.9999999999999858, -155.0000000000000000 ) ) ;
#20060 = EDGE_CURVE ( 'NONE', #29345, #1567, #34498, .T. ) ;
#20061 = EDGE_CURVE ( 'NONE', #22784, #28687, #31102, .T. ) ;
#20062 = FACE_OUTER_BOUND ( 'NONE', #27944, .T. ) ;
#20063 = PLANE ( 'NONE',  #20962 ) ;
#20064 = ORIENTED_EDGE ( 'NONE', *, *, #30636, .F. ) ;
#20065 = CARTESIAN_POINT ( 'NONE',  ( -500.0000000000000000, -137.0000000000000000, 187.0000000000000000 ) ) ;
#20066 = EDGE_CURVE ( 'NONE', #7395, #20222, #21067, .T. ) ;
#20067 = DIRECTION ( 'NONE',  ( 1.000000000000000000, -0.000000000000000000, -0.000000000000000000 ) ) ;
#20068 = AXIS2_PLACEMENT_3D ( 'NONE', #11397, #33287, #32753 ) ;
#20069 = LINE ( 'NONE', #6335, #21195 ) ;
#20070 = ORIENTED_EDGE ( 'NONE', *, *, #20136, .T. ) ;
#20071 = EDGE_CURVE ( 'NONE', #23024, #27819, #13360, .T. ) ;
#20072 = AXIS2_PLACEMENT_3D ( 'NONE', #3886, #15996, #31815 ) ;
#20073 = AXIS2_PLACEMENT_3D ( 'NONE', #29990, #32821, #16480 ) ;
#20074 = EDGE_CURVE ( 'NONE', #8590, #9716, #10507, .T. ) ;
#20075 = LINE ( 'NONE', #9560, #2435 ) ;
#20076 = VERTEX_POINT ( 'NONE', #21001 ) ;
#20077 = CARTESIAN_POINT ( 'NONE',  ( 32.54460952423470133, 0.2297037030477266373, 68.31122994652405112 ) ) ;
#20078 = EDGE_LOOP ( 'NONE', ( #2281, #31328, #18859, #34738 ) ) ;
#20079 = CARTESIAN_POINT ( 'NONE',  ( 0.000000000000000000, 0.000000000000000000, 0.000000000000000000 ) ) ;
#20080 = CARTESIAN_POINT ( 'NONE',  ( 15.00000000000000000, 1.836970198721029589E-15, 20.00000000000000000 ) ) ;
#20081 = CARTESIAN_POINT ( 'NONE',  ( 7.700000000000001954, 0.000000000000000000, 0.000000000000000000 ) ) ;
#20082 = ORIENTED_EDGE ( 'NONE', *, *, #29812, .F. ) ;
#20083 = VECTOR ( 'NONE', #1494, 1000.000000000000000 ) ;
#20084 = DIRECTION ( 'NONE',  ( -0.9739980594652760670, 0.2265563509546286713, -3.242191041697942855E-14 ) ) ;
#20085 = DIRECTION ( 'NONE',  ( 0.000000000000000000, 0.000000000000000000, 1.000000000000000000 ) ) ;
#20086 = ORIENTED_EDGE ( 'NONE', *, *, #27915, .F. ) ;
#20087 = CARTESIAN_POINT ( 'NONE',  ( 1.039999999999999591, -25.27164158951584483, 23.36088151536909052 ) ) ;
#20088 = AXIS2_PLACEMENT_3D ( 'NONE', #25573, #22749, #22920 ) ;
#20089 = VECTOR ( 'NONE', #11707, 1000.000000000000000 ) ;
#20090 = CARTESIAN_POINT ( 'NONE',  ( 11.99999999999999645, -145.0000000000000000, -162.9999999999999432 ) ) ;
#20091 = LINE ( 'NONE', #19736, #24463 ) ;
#20092 = AXIS2_PLACEMENT_3D ( 'NONE', #2675, #26359, #1976 ) ;
#20093 = ORIENTED_EDGE ( 'NONE', *, *, #6737, .F. ) ;
#20094 = VERTEX_POINT ( 'NONE', #18352 ) ;
#20095 = AXIS2_PLACEMENT_3D ( 'NONE', #4320, #15206, #1664 ) ;
#20096 = ORIENTED_EDGE ( 'NONE', *, *, #26747, .F. ) ;
#20097 = LINE ( 'NONE', #1571, #8596 ) ;
#20098 = EDGE_CURVE ( 'NONE', #3490, #16456, #21538, .T. ) ;
#20099 = EDGE_CURVE ( 'NONE', #15441, #26021, #1778, .T. ) ;
#20100 = CARTESIAN_POINT ( 'NONE',  ( 1.749999999999999778, 34.17636915695680244, 4.045051921974837761 ) ) ;
#20101 = DIRECTION ( 'NONE',  ( -1.000000000000000000, 6.792721752314501023E-48, -3.697785493223492838E-32 ) ) ;
#20102 = ORIENTED_EDGE ( 'NONE', *, *, #2444, .F. ) ;
#20103 = LINE ( 'NONE', #33794, #6640 ) ;
#20104 = DIRECTION ( 'NONE',  ( 0.7960930657056439763, 0.6051742151937649083, 1.111686998345333706E-16 ) ) ;
#20105 = ORIENTED_EDGE ( 'NONE', *, *, #4935, .F. ) ;
#20106 = CARTESIAN_POINT ( 'NONE',  ( -5.021133111225092982, -13.65249191622732816, -67.50000000000000000 ) ) ;
#20107 = DIRECTION ( 'NONE',  ( 0.7259954919231307313, 0.6876994588534234287, -0.000000000000000000 ) ) ;
#20108 = EDGE_LOOP ( 'NONE', ( #5047, #13080, #32842, #9648, #27128, #23177 ) ) ;
#20109 = DIRECTION ( 'NONE',  ( -0.000000000000000000, 1.000000000000000000, -0.000000000000000000 ) ) ;
#20110 = VECTOR ( 'NONE', #29058, 1000.000000000000000 ) ;
#20111 = CARTESIAN_POINT ( 'NONE',  ( -12.00000000000001066, 112.9999999999999574, -155.0000000000000000 ) ) ;
#20112 = ORIENTED_EDGE ( 'NONE', *, *, #901, .T. ) ;
#20113 = CYLINDRICAL_SURFACE ( 'NONE', #6125, 3.999999999999976019 ) ;
#20114 = DIRECTION ( 'NONE',  ( 0.000000000000000000, -1.000000000000000000, -1.224646799147353207E-16 ) ) ;
#20115 = CARTESIAN_POINT ( 'NONE',  ( 15.99999999999998579, 4.559999999999908127, -177.7400000000000091 ) ) ;
#20116 = AXIS2_PLACEMENT_3D ( 'NONE', #25401, #33589, #4379 ) ;
#20117 = CIRCLE ( 'NONE', #33749, 7.999999999999979572 ) ;
#20118 = VECTOR ( 'NONE', #34905, 1000.000000000000000 ) ;
#20119 = CARTESIAN_POINT ( 'NONE',  ( -103.3398512556068738, -4.849606089681288701, 11.52174238786261107 ) ) ;
#20120 = CARTESIAN_POINT ( 'NONE',  ( -19.99999999999998934, -124.9999999999999432, -186.9999999999999716 ) ) ;
#20121 = LINE ( 'NONE', #6748, #16617 ) ;
#20122 = ORIENTED_EDGE ( 'NONE', *, *, #33928, .F. ) ;
#20123 = VERTEX_POINT ( 'NONE', #21364 ) ;
#20124 = DIRECTION ( 'NONE',  ( -0.1063910735369017202, 0.9943243633099136947, -1.000770725407181676E-14 ) ) ;
#20125 = ORIENTED_EDGE ( 'NONE', *, *, #10468, .F. ) ;
#20126 = DIRECTION ( 'NONE',  ( 1.000000000000000000, 3.469446951953834515E-18, 0.000000000000000000 ) ) ;
#20127 = AXIS2_PLACEMENT_3D ( 'NONE', #11422, #27787, #3755 ) ;
#20128 = CARTESIAN_POINT ( 'NONE',  ( -12.00000000000001066, -105.0000000000000142, -154.9999999999999716 ) ) ;
#20129 = CONTEXT_DEPENDENT_SHAPE_REPRESENTATION ( #26008, #9523 ) ;
#20130 = VERTEX_POINT ( 'NONE', #32373 ) ;
#20131 = CARTESIAN_POINT ( 'NONE',  ( -442.0000000000000000, 105.0000000000000142, 159.0000000000000000 ) ) ;
#20132 = CARTESIAN_POINT ( 'NONE',  ( -100.6619007216472994, -2.715097909449887048, -12.20238416997437447 ) ) ;
#20133 = EDGE_CURVE ( 'NONE', #27831, #24340, #9972, .T. ) ;
#20135 = AXIS2_PLACEMENT_3D ( 'NONE', #9214, #1032, #11900 ) ;
#20134 = CONTEXT_DEPENDENT_SHAPE_REPRESENTATION ( #21283, #15284 ) ;
#20136 = EDGE_CURVE ( 'NONE', #8625, #3609, #19723, .T. ) ;
#20138 = DIRECTION ( 'NONE',  ( -1.000000000000000000, -0.000000000000000000, -0.000000000000000000 ) ) ;
#20137 = CARTESIAN_POINT ( 'NONE',  ( -23.93921925319781963, 29.33115633223345142, 68.31122994652405112 ) ) ;
#20139 = VECTOR ( 'NONE', #11272, 1000.000000000000000 ) ;
#20140 = ORIENTED_EDGE ( 'NONE', *, *, #6124, .F. ) ;
#20141 = ORIENTED_EDGE ( 'NONE', *, *, #25707, .T. ) ;
#20142 = CIRCLE ( 'NONE', #4760, 10.87635688602997597 ) ;
#20143 = DIRECTION ( 'NONE',  ( 0.000000000000000000, 1.000000000000000000, 1.224646799147353207E-16 ) ) ;
#20144 = EDGE_CURVE ( 'NONE', #16565, #23973, #32528, .T. ) ;
#20145 = CIRCLE ( 'NONE', #28114, 3.999999999999976019 ) ;
#20146 = LINE ( 'NONE', #30991, #19255 ) ;
#20147 = CARTESIAN_POINT ( 'NONE',  ( 2.604019705961582165, 31.85364232850774258, -5.239790278972735749 ) ) ;
#20148 = EDGE_LOOP ( 'NONE', ( #2549, #29580, #28694, #29788 ) ) ;
#20149 = DIRECTION ( 'NONE',  ( 0.000000000000000000, 0.000000000000000000, 1.000000000000000000 ) ) ;
#20150 = CARTESIAN_POINT ( 'NONE',  ( 22.10765473302597073, -14.55883922869198344, -77.50000000000000000 ) ) ;
#20151 =( REPRESENTATION_RELATIONSHIP ('NONE','NONE', #23037, #28231 ) REPRESENTATION_RELATIONSHIP_WITH_TRANSFORMATION ( #31707 )SHAPE_REPRESENTATION_RELATIONSHIP( ) );
#20152 = EDGE_LOOP ( 'NONE', ( #23819, #24217, #2416, #8190 ) ) ;
#20153 = DIRECTION ( 'NONE',  ( 1.000000000000000000, 0.000000000000000000, -1.848892746611746966E-32 ) ) ;
#20154 = DIRECTION ( 'NONE',  ( 0.000000000000000000, 1.836970198721029441E-16, -1.000000000000000000 ) ) ;
#20155 = DIRECTION ( 'NONE',  ( -1.000000000000000000, -0.000000000000000000, -0.000000000000000000 ) ) ;
#20157 = DIRECTION ( 'NONE',  ( 0.000000000000000000, 1.000000000000000000, -0.000000000000000000 ) ) ;
#20156 = DIRECTION ( 'NONE',  ( -1.000000000000000000, 0.000000000000000000, 0.000000000000000000 ) ) ;
#20158 = VECTOR ( 'NONE', #7058, 1000.000000000000000 ) ;
#20159 = CARTESIAN_POINT ( 'NONE',  ( 0.1835379687083470712, 12.63602821951847233, -29.69442701139029950 ) ) ;
#20160 = CARTESIAN_POINT ( 'NONE',  ( 2.765921099435497243, 28.29688452313399338, 12.88099432405614309 ) ) ;
#20161 = ORIENTED_EDGE ( 'NONE', *, *, #4967, .T. ) ;
#20162 = DIRECTION ( 'NONE',  ( 0.000000000000000000, -1.000000000000000000, 6.123233995736766036E-17 ) ) ;
#20163 = DIRECTION ( 'NONE',  ( -0.000000000000000000, 0.000000000000000000, 1.000000000000000000 ) ) ;
#20164 = VECTOR ( 'NONE', #12132, 1000.000000000000000 ) ;
#20165 = CARTESIAN_POINT ( 'NONE',  ( 0.5288002592091670673, -32.14027485980077614, -9.048862969376250120 ) ) ;
#20167 = ORIENTED_EDGE ( 'NONE', *, *, #9962, .T. ) ;
#20166 = AXIS2_PLACEMENT_3D ( 'NONE', #14992, #28506, #26169 ) ;
#20168 = AXIS2_PLACEMENT_3D ( 'NONE', #27101, #582, #14117 ) ;
#20169 = AXIS2_PLACEMENT_3D ( 'NONE', #11370, #5826, #6180 ) ;
#20170 = EDGE_LOOP ( 'NONE', ( #34216, #20658, #23894, #16451 ) ) ;
#20171 = LINE ( 'NONE', #22352, #5641 ) ;
#20172 = ORIENTED_EDGE ( 'NONE', *, *, #8968, .F. ) ;
#20173 = VERTEX_POINT ( 'NONE', #32023 ) ;
#20174 = ORIENTED_EDGE ( 'NONE', *, *, #902, .T. ) ;
#20175 = CYLINDRICAL_SURFACE ( 'NONE', #28122, 10.00000000000000000 ) ;
#20176 = EDGE_CURVE ( 'NONE', #15056, #20282, #528, .T. ) ;
#20177 = VECTOR ( 'NONE', #7717, 1000.000000000000000 ) ;
#20178 = VERTEX_POINT ( 'NONE', #3184 ) ;
#20179 = DIRECTION ( 'NONE',  ( 0.000000000000000000, 0.000000000000000000, -1.000000000000000000 ) ) ;
#20180 = CARTESIAN_POINT ( 'NONE',  ( -35.55956070192387841, -17.65143121711728469, 10.00000000000000000 ) ) ;
#20181 = ORIENTED_EDGE ( 'NONE', *, *, #28499, .T. ) ;
#20182 = EDGE_LOOP ( 'NONE', ( #15017, #19425, #7677, #32188 ) ) ;
#20183 = DIRECTION ( 'NONE',  ( 1.000000000000000000, 0.000000000000000000, -1.232595164407831220E-32 ) ) ;
#20184 = CARTESIAN_POINT ( 'NONE',  ( 0.1859802519188287762, -28.85000931094353049, 14.48402167767607729 ) ) ;
#20185 = ADVANCED_FACE ( 'NONE', ( #10850 ), #22235, .T. ) ;
#20186 = AXIS2_PLACEMENT_3D ( 'NONE', #9590, #20445, #20788 ) ;
#20187 = EDGE_CURVE ( 'NONE', #17291, #33296, #10621, .T. ) ;
#20188 = DIRECTION ( 'NONE',  ( 0.000000000000000000, -1.000000000000000000, -1.836970198721029934E-16 ) ) ;
#20189 = CARTESIAN_POINT ( 'NONE',  ( 1.749999999999999778, -1.891117961020238436, 34.36292081097831641 ) ) ;
#20190 = CARTESIAN_POINT ( 'NONE',  ( -15.99999999999998579, 112.9999999999999574, -155.0000000000000000 ) ) ;
#20191 = VERTEX_POINT ( 'NONE', #24717 ) ;
#20192 = CARTESIAN_POINT ( 'NONE',  ( -500.0000000000000000, -137.0000000000000000, 162.9999999999999716 ) ) ;
#20193 = DIRECTION ( 'NONE',  ( 0.000000000000000000, 0.000000000000000000, -1.000000000000000000 ) ) ;
#20194 = LINE ( 'NONE', #6641, #26466 ) ;
#20195 = VECTOR ( 'NONE', #5988, 1000.000000000000000 ) ;
#20196 = ADVANCED_FACE ( 'NONE', ( #5315 ), #21878, .F. ) ;
#20197 = EDGE_CURVE ( 'NONE', #18398, #21299, #25736, .T. ) ;
#20198 = CYLINDRICAL_SURFACE ( 'NONE', #1096, 4.682234377621698584 ) ;
#20199 = ORIENTED_EDGE ( 'NONE', *, *, #12489, .T. ) ;
#20200 = CLOSED_SHELL ( 'NONE', ( #10820, #17983, #12351, #32607, #29074, #26488, #22015, #29358, #28356, #34976 ) ) ;
#20201 = CARTESIAN_POINT ( 'NONE',  ( 0.1835382055501959819, -30.93445778156035786, 9.191712967690730096 ) ) ;
#20202 = CARTESIAN_POINT ( 'NONE',  ( 0.02407890056655738464, 24.20451283648857554, -19.51346322004903300 ) ) ;
#20203 = CARTESIAN_POINT ( 'NONE',  ( -30.76765767668601725, -10.60922306139171667, 68.31122994652405112 ) ) ;
#20204 = EDGE_CURVE ( 'NONE', #1801, #4360, #3000, .T. ) ;
#20205 = LINE ( 'NONE', #33360, #20643 ) ;
#20206 = CARTESIAN_POINT ( 'NONE',  ( 0.000000000000000000, 0.000000000000000000, 0.000000000000000000 ) ) ;
#20207 = CARTESIAN_POINT ( 'NONE',  ( 2.261199744265443901, -1.325911039507465583, 33.36347027112249464 ) ) ;
#20208 = ORIENTED_EDGE ( 'NONE', *, *, #32655, .T. ) ;
#20209 = FACE_OUTER_BOUND ( 'NONE', #22239, .T. ) ;
#20210 = DIRECTION ( 'NONE',  ( -1.000000000000000000, 0.000000000000000000, 0.000000000000000000 ) ) ;
#20211 = VECTOR ( 'NONE', #18907, 1000.000000000000227 ) ;
#20212 = EDGE_LOOP ( 'NONE', ( #29124, #30010, #28111, #29795 ) ) ;
#20213 = VECTOR ( 'NONE', #10603, 1000.000000000000000 ) ;
#20214 = CARTESIAN_POINT ( 'NONE',  ( 2.790000000000082636, 30.58763704338517542, 2.144802104989564473 ) ) ;
#20215 = VECTOR ( 'NONE', #30024, 1000.000000000000000 ) ;
#20216 = ORIENTED_EDGE ( 'NONE', *, *, #31503, .F. ) ;
#20217 = AXIS2_PLACEMENT_3D ( 'NONE', #26843, #29692, #16184 ) ;
#20218 = VECTOR ( 'NONE', #9002, 1000.000000000000000 ) ;
#20219 = ORIENTED_EDGE ( 'NONE', *, *, #30535, .T. ) ;
#20220 = DIRECTION ( 'NONE',  ( 0.000000000000000000, 1.000000000000000000, 5.053935297177146739E-49 ) ) ;
#20221 = ORIENTED_EDGE ( 'NONE', *, *, #32146, .F. ) ;
#20222 = VERTEX_POINT ( 'NONE', #8356 ) ;
#20223 = CARTESIAN_POINT ( 'NONE',  ( 5.021133111224576062, 14.09580098603202458, -67.50000000000000000 ) ) ;
#20224 = AXIS2_PLACEMENT_3D ( 'NONE', #32262, #18589, #2356 ) ;
#20225 = DIRECTION ( 'NONE',  ( 1.000000000000000000, 0.000000000000000000, 0.000000000000000000 ) ) ;
#20226 = AXIS2_PLACEMENT_3D ( 'NONE', #1687, #12915, #34614 ) ;
#20227 = CARTESIAN_POINT ( 'NONE',  ( -414.0000000000000568, -105.0000000000000142, 162.9999999999999716 ) ) ;
#20228 = CARTESIAN_POINT ( 'NONE',  ( 0.000000000000000000, 3.524919873834583163E-15, 68.31122994652405112 ) ) ;
#20229 = ORIENTED_EDGE ( 'NONE', *, *, #28908, .F. ) ;
#20230 = VERTEX_POINT ( 'NONE', #19229 ) ;
#20231 = LINE ( 'NONE', #34262, #20236 ) ;
#20232 = CARTESIAN_POINT ( 'NONE',  ( -500.0000000000000000, -141.0000000000000000, 162.9999999999999716 ) ) ;
#20233 = CARTESIAN_POINT ( 'NONE',  ( -37.85301660235036536, 0.7430237821112573027, 68.31122994652405112 ) ) ;
#20234 = CARTESIAN_POINT ( 'NONE',  ( -410.0000000000000568, 105.0000000000000142, 187.0000000000000000 ) ) ;
#20235 = CARTESIAN_POINT ( 'NONE',  ( -20.02113311122509032, -15.68591377522703745, -67.50000000000000000 ) ) ;
#20236 = VECTOR ( 'NONE', #28232, 1000.000000000000000 ) ;
#20237 = DIRECTION ( 'NONE',  ( 1.848892746611746966E-32, -6.842277657836020854E-49, 1.000000000000000000 ) ) ;
#20238 = EDGE_CURVE ( 'NONE', #14266, #9246, #29392, .T. ) ;
#20239 = ADVANCED_FACE ( 'NONE', ( #33263 ), #30072, .T. ) ;
#20240 = CARTESIAN_POINT ( 'NONE',  ( 0.000000000000000000, 0.000000000000000000, 0.000000000000000000 ) ) ;
#20241 = ORIENTED_EDGE ( 'NONE', *, *, #18585, .F. ) ;
#20242 = AXIS2_PLACEMENT_3D ( 'NONE', #2912, #6110, #11126 ) ;
#20243 = CYLINDRICAL_SURFACE ( 'NONE', #9412, 7.999999999999979572 ) ;
#20244 = DIRECTION ( 'NONE',  ( 0.000000000000000000, -0.5000000000000018874, -0.8660254037844374864 ) ) ;
#20245 = LINE ( 'NONE', #6158, #30852 ) ;
#20246 = ORIENTED_EDGE ( 'NONE', *, *, #29687, .F. ) ;
#20247 = DIRECTION ( 'NONE',  ( 0.000000000000000000, 1.000000000000000000, 5.145227585319922065E-49 ) ) ;
#20248 = ORIENTED_EDGE ( 'NONE', *, *, #2762, .F. ) ;
#20249 = DIRECTION ( 'NONE',  ( 0.000000000000000000, 1.000000000000000000, 0.000000000000000000 ) ) ;
#20250 = CARTESIAN_POINT ( 'NONE',  ( 1.395000000000002238, 28.00026196654299682, -20.00929742917093179 ) ) ;
#20251 = EDGE_CURVE ( 'NONE', #6306, #4415, #24454, .T. ) ;
#20252 = ORIENTED_EDGE ( 'NONE', *, *, #27849, .F. ) ;
#20253 = DIRECTION ( 'NONE',  ( 1.000000000000000000, -0.000000000000000000, -0.000000000000000000 ) ) ;
#20254 = DIRECTION ( 'NONE',  ( 0.000000000000000000, -2.465190328815661892E-32, -1.000000000000000000 ) ) ;
#20255 = CYLINDRICAL_SURFACE ( 'NONE', #16077, 44.99999999999997868 ) ;
#20256 = EDGE_CURVE ( 'NONE', #2574, #25012, #11210, .T. ) ;
#20257 = EDGE_LOOP ( 'NONE', ( #23629, #27646, #17965, #18946 ) ) ;
#20258 = ADVANCED_FACE ( 'NONE', ( #27392 ), #5840, .T. ) ;
#20259 = EDGE_CURVE ( 'NONE', #33397, #8951, #23151, .T. ) ;
#20260 = VECTOR ( 'NONE', #9317, 1000.000000000000000 ) ;
#20261 = DIRECTION ( 'NONE',  ( -1.111053370210468842E-15, -4.567041301615147026E-14, 1.000000000000000000 ) ) ;
#20262 = CARTESIAN_POINT ( 'NONE',  ( 2.765921099433442887, -23.70329957282599764, 20.11932597908820242 ) ) ;
#20263 = EDGE_LOOP ( 'NONE', ( #4698, #22160, #33730, #34439 ) ) ;
#20264 = CIRCLE ( 'NONE', #23107, 8.000000000000000000 ) ;
#20265 = CARTESIAN_POINT ( 'NONE',  ( 12.00000000000001066, -64.99999999999997158, -154.9999999999999716 ) ) ;
#20266 = EDGE_CURVE ( 'NONE', #21471, #16703, #19575, .T. ) ;
#20267 = CARTESIAN_POINT ( 'NONE',  ( 145.0000000000000568, -97.56119630548165844, -180.0000000000000000 ) ) ;
#20268 = LINE ( 'NONE', #34299, #6085 ) ;
#20269 = DIRECTION ( 'NONE',  ( -1.000000000000000000, 0.000000000000000000, 1.232595164407831220E-32 ) ) ;
#20270 = ORIENTED_EDGE ( 'NONE', *, *, #27164, .F. ) ;
#20271 = VERTEX_POINT ( 'NONE', #27570 ) ;
#20272 = ORIENTED_EDGE ( 'NONE', *, *, #14398, .F. ) ;
#20273 = DIRECTION ( 'NONE',  ( -0.000000000000000000, -0.000000000000000000, -1.000000000000000000 ) ) ;
#20274 = DIRECTION ( 'NONE',  ( 0.000000000000000000, 1.836970198721029688E-16, -1.000000000000000000 ) ) ;
#20275 = DIRECTION ( 'NONE',  ( -3.469446951953832974E-18, -1.000000000000000000, -7.888609052210116302E-31 ) ) ;
#20276 = EDGE_CURVE ( 'NONE', #33086, #29943, #8525, .T. ) ;
#20277 = FACE_OUTER_BOUND ( 'NONE', #26775, .T. ) ;
#20278 = CARTESIAN_POINT ( 'NONE',  ( 1.040000000000000924, 0.000000000000000000, 0.000000000000000000 ) ) ;
#20279 = VERTEX_POINT ( 'NONE', #30236 ) ;
#20280 = PRODUCT_DEFINITION_SHAPE ( 'NONE', 'NONE',  #35157 ) ;
#20281 = CARTESIAN_POINT ( 'NONE',  ( 103.4967993190871169, 5.550581019792739212, 11.20035861729703086 ) ) ;
#20282 = VERTEX_POINT ( 'NONE', #16734 ) ;
#20283 = VECTOR ( 'NONE', #22455, 1000.000000000000000 ) ;
#20284 = CYLINDRICAL_SURFACE ( 'NONE', #28819, 7.999999999999979572 ) ;
#20285 = LINE ( 'NONE', #31474, #27998 ) ;
#20286 = EDGE_LOOP ( 'NONE', ( #4473, #26560, #5124, #30752 ) ) ;
#20287 = VECTOR ( 'NONE', #3144, 1000.000000000000000 ) ;
#20288 = CARTESIAN_POINT ( 'NONE',  ( 5.390701026406702567, -37.47456861236020131, 68.31122994652405112 ) ) ;
#20289 = LINE ( 'NONE', #14429, #9212 ) ;
#20290 = DIRECTION ( 'NONE',  ( 1.000000000000000000, 0.000000000000000000, 0.000000000000000000 ) ) ;
#20291 = CARTESIAN_POINT ( 'NONE',  ( 1.749999999999999778, 22.14447232807545163, -26.34405054495532639 ) ) ;
#20292 = UNCERTAINTY_MEASURE_WITH_UNIT (LENGTH_MEASURE( 1.000000000000000082E-05 ), #22824, 'distance_accuracy_value', 'NONE');
#20293 = DIRECTION ( 'NONE',  ( -2.736911063134582149E-48, 7.888609052210118054E-31, 1.000000000000000000 ) ) ;
#20294 = CARTESIAN_POINT ( 'NONE',  ( 34.58310883014599568, -15.42890216704097206, 68.31122994652405112 ) ) ;
#20295 = EDGE_CURVE ( 'NONE', #6345, #8526, #8332, .T. ) ;
#20296 = CIRCLE ( 'NONE', #35055, 3.999999999999982681 ) ;
#20297 = EDGE_LOOP ( 'NONE', ( #20821, #18595, #32905, #8148, #4495, #5231, #22582, #6213, #4325, #18534, #34205, #11408, #27848, #11017, #6054, #24346, #30464, #10647, #7818, #92, #4637, #32928, #357, #6729, #17685, #27987, #9574, #14931, #32194, #17798, #21285, #14518, #11910, #35037, #12377, #25947, #6048, #21483, #3362, #23701, #8861, #34528, #25404, #18164, #23310, #25243 ) ) ;
#20298 = EDGE_CURVE ( 'NONE', #27718, #11639, #21998, .T. ) ;
#20299 = EDGE_CURVE ( 'NONE', #34042, #34303, #11920, .T. ) ;
#20300 = VERTEX_POINT ( 'NONE', #33437 ) ;
#20301 = CARTESIAN_POINT ( 'NONE',  ( 799.5825435092968974, 972.2896973994317023, 1753.598338701303874 ) ) ;
#20302 = ORIENTED_EDGE ( 'NONE', *, *, #31682, .F. ) ;
#20303 = VECTOR ( 'NONE', #30996, 1000.000000000000000 ) ;
#20304 = CARTESIAN_POINT ( 'NONE',  ( -349.0000000000000000, 134.9999999999999716, 111.9999999999999858 ) ) ;
#20305 = CIRCLE ( 'NONE', #4344, 2.033421858999711951 ) ;
#20306 = AXIS2_PLACEMENT_3D ( 'NONE', #5486, #24521, #24002 ) ;
#20307 = CARTESIAN_POINT ( 'NONE',  ( -32.37866696771086339, 3.290334066652078171, 68.31122994652405112 ) ) ;
#20308 = CONTEXT_DEPENDENT_SHAPE_REPRESENTATION ( #19894, #4392 ) ;
#20309 = ORIENTED_EDGE ( 'NONE', *, *, #28997, .F. ) ;
#20310 = DIRECTION ( 'NONE',  ( 1.000000000000000000, 3.469446951953834515E-18, -2.736911063134582149E-48 ) ) ;
#20311 = CARTESIAN_POINT ( 'NONE',  ( -30.91434716440808472, 10.17386417614053151, 68.31122994652405112 ) ) ;
#20313 = LINE ( 'NONE', #17308, #23218 ) ;
#20312 = DIRECTION ( 'NONE',  ( 0.000000000000000000, 0.000000000000000000, -1.000000000000000000 ) ) ;
#20314 = ORIENTED_EDGE ( 'NONE', *, *, #2520, .F. ) ;
#20315 = EDGE_LOOP ( 'NONE', ( #17896, #30988, #33444, #32401 ) ) ;
#20316 = CARTESIAN_POINT ( 'NONE',  ( -355.0000000000000000, -119.0000000000000000, 109.9999999999999858 ) ) ;
#20317 = CARTESIAN_POINT ( 'NONE',  ( 2.765921099433442887, 24.20451283648829133, 19.51346322004938827 ) ) ;
#20318 = DIRECTION ( 'NONE',  ( -0.000000000000000000, 1.000000000000000000, 1.224646799147353207E-16 ) ) ;
#20319 = ORIENTED_EDGE ( 'NONE', *, *, #17593, .F. ) ;
#20320 = CARTESIAN_POINT ( 'NONE',  ( 1.040000000000001146, -25.27164158951551087, -23.36088151536945645 ) ) ;
#20321 = VECTOR ( 'NONE', #9545, 1000.000000000000000 ) ;
#20322 = VERTEX_POINT ( 'NONE', #14595 ) ;
#20323 = EDGE_CURVE ( 'NONE', #28711, #19987, #6894, .T. ) ;
#20324 = DIRECTION ( 'NONE',  ( -1.000000000000000000, -0.000000000000000000, -0.000000000000000000 ) ) ;
#20325 = LINE ( 'NONE', #14816, #1781 ) ;
#20326 = DIRECTION ( 'NONE',  ( 0.9289767198167914186, -0.3701381553399144542, 0.000000000000000000 ) ) ;
#20328 = LINE ( 'NONE', #1623, #28188 ) ;
#20327 = CARTESIAN_POINT ( 'NONE',  ( 0.000000000000000000, -32.54542015209057126, 87.50000000000000000 ) ) ;
#20329 = AXIS2_PLACEMENT_3D ( 'NONE', #34311, #15988, #26299 ) ;
#20330 = CIRCLE ( 'NONE', #9528, 2.000000000000001776 ) ;
#20331 = CARTESIAN_POINT ( 'NONE',  ( 11.99999999999999645, 104.9999999999999858, -175.0000000000000284 ) ) ;
#20332 = CARTESIAN_POINT ( 'NONE',  ( 2.397606348813468014, 30.27116788627787614, 13.00174666746673324 ) ) ;
#20333 = ORIENTED_EDGE ( 'NONE', *, *, #27300, .F. ) ;
#20334 = PLANE ( 'NONE',  #4785 ) ;
#20335 = SURFACE_SIDE_STYLE ('',( #12500 ) ) ;
#20336 = EDGE_CURVE ( 'NONE', #7906, #1533, #20305, .T. ) ;
#20337 = AXIS2_PLACEMENT_3D ( 'NONE', #2258, #31976, #32328 ) ;
#20338 = ADVANCED_FACE ( 'NONE', ( #15114 ), #14768, .T. ) ;
#20339 = ADVANCED_FACE ( 'NONE', ( #20277 ), #9233, .T. ) ;
#20340 = ORIENTED_EDGE ( 'NONE', *, *, #12466, .F. ) ;
#20341 = EDGE_CURVE ( 'NONE', #18803, #18049, #17622, .T. ) ;
#20342 = VERTEX_POINT ( 'NONE', #17791 ) ;
#20343 = VECTOR ( 'NONE', #18988, 1000.000000000000000 ) ;
#20344 = CARTESIAN_POINT ( 'NONE',  ( -105.0000000000000000, 0.000000000000000000, -57.49999999999999289 ) ) ;
#20345 = ORIENTED_EDGE ( 'NONE', *, *, #12797, .F. ) ;
#20346 = VERTEX_POINT ( 'NONE', #14419 ) ;
#20347 = ORIENTED_EDGE ( 'NONE', *, *, #381, .T. ) ;
#20348 = DIRECTION ( 'NONE',  ( 0.000000000000000000, -1.131431318426415506E-52, -1.000000000000000000 ) ) ;
#20349 = CONTEXT_DEPENDENT_SHAPE_REPRESENTATION ( #4891, #13016 ) ;
#20350 = AXIS2_PLACEMENT_3D ( 'NONE', #29883, #24513, #16372 ) ;
#20351 = AXIS2_PLACEMENT_3D ( 'NONE', #11223, #27228, #3013 ) ;
#20352 = VERTEX_POINT ( 'NONE', #1224 ) ;
#20353 = CARTESIAN_POINT ( 'NONE',  ( 9.199999999999999289, 0.000000000000000000, 13.50000000000000178 ) ) ;
#20354 = CARTESIAN_POINT ( 'NONE',  ( 0.02407890056655868569, 24.20451283648829133, 19.51346322004938827 ) ) ;
#20355 = ORIENTED_EDGE ( 'NONE', *, *, #8643, .T. ) ;
#20356 = ORIENTED_EDGE ( 'NONE', *, *, #24609, .F. ) ;
#20357 =( REPRESENTATION_RELATIONSHIP ('NONE','NONE', #23037, #15767 ) REPRESENTATION_RELATIONSHIP_WITH_TRANSFORMATION ( #28440 )SHAPE_REPRESENTATION_RELATIONSHIP( ) );
#20358 = DIRECTION ( 'NONE',  ( -1.000000000000000000, -3.469446951953834515E-18, 0.000000000000000000 ) ) ;
#20359 = DIRECTION ( 'NONE',  ( -1.000000000000000000, 0.000000000000000000, -5.546364386991661285E-52 ) ) ;
#20360 = DIRECTION ( 'NONE',  ( 0.000000000000000000, -0.000000000000000000, 1.000000000000000000 ) ) ;
#20361 = CARTESIAN_POINT ( 'NONE',  ( -20.00000000000007461, 144.9999999999999432, 162.9999999999999716 ) ) ;
#20362 = CARTESIAN_POINT ( 'NONE',  ( 8.986540508143576744, 33.69708579775584667, -36.68877005347592757 ) ) ;
#20363 = ORIENTED_EDGE ( 'NONE', *, *, #34707, .F. ) ;
#20364=STYLED_ITEM('',(#35254),#11835);
#20365 = DIRECTION ( 'NONE',  ( 1.232595164407830946E-32, 3.421138828918010427E-49, -1.000000000000000000 ) ) ;
#20366 = CYLINDRICAL_SURFACE ( 'NONE', #337, 7.999999999999979572 ) ;
#20367 = CYLINDRICAL_SURFACE ( 'NONE', #34093, 4.000000000000003553 ) ;
#20368 = EDGE_LOOP ( 'NONE', ( #4554, #32766, #31195, #12725 ) ) ;
#20369 = CARTESIAN_POINT ( 'NONE',  ( -7.920605089774962471E-15, 12.02207793746705455, 6.177150199754207094 ) ) ;
#20370 = CARTESIAN_POINT ( 'NONE',  ( 7.056651121978252318E-16, 23.76428138080773422, -19.37504760381629865 ) ) ;
#20371 = DIRECTION ( 'NONE',  ( 0.000000000000000000, 1.836970198721029441E-16, -1.000000000000000000 ) ) ;
#20372 = CARTESIAN_POINT ( 'NONE',  ( -143.0000000000000568, -187.5436536988702017, -180.0000000000000284 ) ) ;
#20374 = LINE ( 'NONE', #1153, #33265 ) ;
#20373 = CARTESIAN_POINT ( 'NONE',  ( -19.99999999999998934, 4.559999999999908127, -177.7400000000000091 ) ) ;
#20375 = VECTOR ( 'NONE', #24967, 1000.000000000000000 ) ;
#20376 = EDGE_CURVE ( 'NONE', #31329, #1812, #2105, .T. ) ;
#20377 = CARTESIAN_POINT ( 'NONE',  ( 1.749999999999999778, -1.891117961020238436, 34.36292081097831641 ) ) ;
#20378 = ORIENTED_EDGE ( 'NONE', *, *, #28651, .F. ) ;
#20379 = LINE ( 'NONE', #22701, #3070 ) ;
#20381 = CARTESIAN_POINT ( 'NONE',  ( 143.0000000000000568, -97.49999999999998579, 51.88904920397793319 ) ) ;
#20380 = DIRECTION ( 'NONE',  ( -0.000000000000000000, 1.836970198721029688E-16, -1.000000000000000000 ) ) ;
#20382 = EDGE_CURVE ( 'NONE', #31298, #16780, #13017, .T. ) ;
#20383 = VECTOR ( 'NONE', #16764, 1000.000000000000000 ) ;
#20384 = ORIENTED_EDGE ( 'NONE', *, *, #9724, .F. ) ;
#20385 = VECTOR ( 'NONE', #28827, 1000.000000000000000 ) ;
#20386 = CYLINDRICAL_SURFACE ( 'NONE', #15440, 34.41491905851385269 ) ;
#20387 = EDGE_CURVE ( 'NONE', #9427, #22681, #29953, .T. ) ;
#20388 = ORIENTED_EDGE ( 'NONE', *, *, #27113, .T. ) ;
#20389 = EDGE_CURVE ( 'NONE', #24880, #31033, #20103, .T. ) ;
#20390 = ORIENTED_EDGE ( 'NONE', *, *, #20872, .T. ) ;
#20391 = DIRECTION ( 'NONE',  ( 0.000000000000000000, 1.000000000000000000, 1.934419779023891545E-16 ) ) ;
#20392 = VERTEX_POINT ( 'NONE', #28449 ) ;
#20393 = VERTEX_POINT ( 'NONE', #6557 ) ;
#20394 = DIRECTION ( 'NONE',  ( 0.000000000000000000, 0.000000000000000000, 1.000000000000000000 ) ) ;
#20395 = EDGE_CURVE ( 'NONE', #33264, #24034, #17270, .T. ) ;
#20396 = AXIS2_PLACEMENT_3D ( 'NONE', #14421, #22596, #3880 ) ;
#20397 = EDGE_CURVE ( 'NONE', #28359, #30843, #8907, .T. ) ;
#20398 = DIRECTION ( 'NONE',  ( -0.000000000000000000, -0.000000000000000000, 1.000000000000000000 ) ) ;
#20399 = DIRECTION ( 'NONE',  ( 0.000000000000000000, -1.000000000000000000, -2.465190328815662439E-32 ) ) ;
#20400 = CARTESIAN_POINT ( 'NONE',  ( -442.0000000000000000, -145.0000000000000000, -155.0000000000000000 ) ) ;
#20401 = ORIENTED_EDGE ( 'NONE', *, *, #30047, .T. ) ;
#20402 = ORIENTED_EDGE ( 'NONE', *, *, #33677, .T. ) ;
#20403 = CARTESIAN_POINT ( 'NONE',  ( -347.0000000000000000, -125.0000000000000284, 126.0000000000000000 ) ) ;
#20404 = CARTESIAN_POINT ( 'NONE',  ( 0.0001801434340936737804, -25.83993731729792742, -16.24881338200996694 ) ) ;
#20405 = CARTESIAN_POINT ( 'NONE',  ( -355.0000000000000000, 118.9999999999999716, 126.0000000000000000 ) ) ;
#20406 = LINE ( 'NONE', #15070, #31213 ) ;
#20407 = DIRECTION ( 'NONE',  ( 0.000000000000000000, -3.435095992033281961E-15, -1.000000000000000000 ) ) ;
#20408 = CIRCLE ( 'NONE', #7287, 7.999999999999979572 ) ;
#20409 = FACE_OUTER_BOUND ( 'NONE', #2055, .T. ) ;
#20410 = CARTESIAN_POINT ( 'NONE',  ( 0.5355294694855750048, -9.071383756617063199, 11.28790243858421505 ) ) ;
#20411 = VERTEX_POINT ( 'NONE', #9420 ) ;
#20412 = CARTESIAN_POINT ( 'NONE',  ( -6.500000000000000000, 0.000000000000000000, -0.7500000000000000000 ) ) ;
#20413 = FACE_BOUND ( 'NONE', #16860, .T. ) ;
#20414 = VECTOR ( 'NONE', #29855, 1000.000000000000000 ) ;
#20415 = DIRECTION ( 'NONE',  ( -0.000000000000000000, -0.000000000000000000, 1.000000000000000000 ) ) ;
#20416 = ORIENTED_EDGE ( 'NONE', *, *, #31153, .F. ) ;
#20417 = DIRECTION ( 'NONE',  ( 0.000000000000000000, 0.000000000000000000, 1.000000000000000000 ) ) ;
#20418 = VERTEX_POINT ( 'NONE', #9592 ) ;
#20420 = DIRECTION ( 'NONE',  ( -0.000000000000000000, 1.000000000000000000, 1.224646799147353207E-16 ) ) ;
#20419 = FACE_OUTER_BOUND ( 'NONE', #16281, .T. ) ;
#20421 = CARTESIAN_POINT ( 'NONE',  ( -109.0615761322723785, 3.126956236148902946, 12.10589691785418509 ) ) ;
#20422 = CIRCLE ( 'NONE', #11352, 1.649999999999999467 ) ;
#20423 = ORIENTED_EDGE ( 'NONE', *, *, #9086, .F. ) ;
#20424 = LINE ( 'NONE', #33943, #31355 ) ;
#20425 = PLANE ( 'NONE',  #34408 ) ;
#20426 = ADVANCED_FACE ( 'NONE', ( #25242 ), #3795, .T. ) ;
#20427 = ORIENTED_EDGE ( 'NONE', *, *, #32617, .F. ) ;
#20428 = CIRCLE ( 'NONE', #20980, 32.54542015209056416 ) ;
#20429 = ADVANCED_FACE ( 'NONE', ( #20448 ), #28797, .F. ) ;
#20430 = EDGE_CURVE ( 'NONE', #17427, #143, #34131, .T. ) ;
#20431 = DIRECTION ( 'NONE',  ( -0.8101611041189152873, -0.5862072887407836497, -2.767246121501470101E-14 ) ) ;
#20432 = CARTESIAN_POINT ( 'NONE',  ( 101.2097724487970964, -4.324042002361276005, 11.73155476838175559 ) ) ;
#20433 = ORIENTED_EDGE ( 'NONE', *, *, #28445, .T. ) ;
#20434 = CYLINDRICAL_SURFACE ( 'NONE', #4172, 4.306175033202026547 ) ;
#20435 = AXIS2_PLACEMENT_3D ( 'NONE', #21091, #28587, #12753 ) ;
#20436 = CYLINDRICAL_SURFACE ( 'NONE', #27197, 2.000000000000001776 ) ;
#20437 = DIRECTION ( 'NONE',  ( -0.5155538571770215128, 0.8568571761675894960, 1.574021097180117283E-16 ) ) ;
#20438 = DIRECTION ( 'NONE',  ( 0.000000000000000000, 1.836970198721030181E-16, -1.000000000000000000 ) ) ;
#20439 = VERTEX_POINT ( 'NONE', #4563 ) ;
#20440 = ORIENTED_EDGE ( 'NONE', *, *, #15963, .F. ) ;
#20441 = VERTEX_POINT ( 'NONE', #1911 ) ;
#20442 = DIRECTION ( 'NONE',  ( 1.000000000000000000, 0.000000000000000000, 5.546364386991661285E-52 ) ) ;
#20443 = EDGE_CURVE ( 'NONE', #18486, #16556, #29508, .T. ) ;
#20444 = DIRECTION ( 'NONE',  ( 0.000000000000000000, -5.053935297177146739E-49, -1.000000000000000000 ) ) ;
#20445 = DIRECTION ( 'NONE',  ( -0.000000000000000000, 0.000000000000000000, 1.000000000000000000 ) ) ;
#20446 = AXIS2_PLACEMENT_3D ( 'NONE', #12922, #22972, #7910 ) ;
#20447 = CYLINDRICAL_SURFACE ( 'NONE', #33565, 3.999999999999976019 ) ;
#20448 = FACE_OUTER_BOUND ( 'NONE', #6381, .T. ) ;
#20449 = CYLINDRICAL_SURFACE ( 'NONE', #10159, 3.999999999999976019 ) ;
#20450 = EDGE_LOOP ( 'NONE', ( #33372, #598, #11321, #13793 ) ) ;
#20451 = EDGE_CURVE ( 'NONE', #21855, #17151, #31466, .T. ) ;
#20452 = CARTESIAN_POINT ( 'NONE',  ( 101.2030210553239726, 4.317991217963452755, 11.73376546078469040 ) ) ;
#20454 = EDGE_CURVE ( 'NONE', #22009, #3503, #18149, .T. ) ;
#20453 = VERTEX_POINT ( 'NONE', #32166 ) ;
#20455 = EDGE_CURVE ( 'NONE', #12627, #26996, #29147, .T. ) ;
#20456 = CARTESIAN_POINT ( 'NONE',  ( 2.765921099433442887, -30.46391896562411716, 6.211548095912460710 ) ) ;
#20457 = ORIENTED_EDGE ( 'NONE', *, *, #18846, .T. ) ;
#20458 = CARTESIAN_POINT ( 'NONE',  ( -15.99999999999998579, 144.9999999999999716, -162.9999999999999432 ) ) ;
#20459 = DIRECTION ( 'NONE',  ( 0.000000000000000000, -1.000000000000000000, -1.224646799147353207E-16 ) ) ;
#20460 = AXIS2_PLACEMENT_3D ( 'NONE', #17071, #30582, #25042 ) ;
#20461 = CYLINDRICAL_SURFACE ( 'NONE', #18845, 15.00000000000000000 ) ;
#20462 = CARTESIAN_POINT ( 'NONE',  ( 129.3530333899765594, -6.000000000000000000, 62.49999999999999289 ) ) ;
#20463 = DIRECTION ( 'NONE',  ( 1.000000000000000000, 0.000000000000000000, 0.000000000000000000 ) ) ;
#20464 = ORIENTED_EDGE ( 'NONE', *, *, #8713, .T. ) ;
#20465 = ORIENTED_EDGE ( 'NONE', *, *, #15161, .F. ) ;
#20466 = EDGE_CURVE ( 'NONE', #10873, #11323, #34489, .T. ) ;
#20467 = EDGE_CURVE ( 'NONE', #27028, #2439, #4401, .T. ) ;
#20468 = DIRECTION ( 'NONE',  ( -7.893605728314050488E-14, 1.618803117314786135E-15, 0.9999999999999998890 ) ) ;
#20469 = ORIENTED_EDGE ( 'NONE', *, *, #21309, .T. ) ;
#20470 = EDGE_CURVE ( 'NONE', #32964, #32317, #11805, .T. ) ;
#20471 = CARTESIAN_POINT ( 'NONE',  ( 1.040000000000001590, -33.39989884085085947, -8.296590337300607132 ) ) ;
#20472 = CARTESIAN_POINT ( 'NONE',  ( 2.789999999999999147, -2.530647759431734922, 30.33427519320593646 ) ) ;
#20473 = ITEM_DEFINED_TRANSFORMATION ( 'NONE', 'NONE', #10979,  #28566 ) ;
#20474 = EDGE_LOOP ( 'NONE', ( #5013, #11858, #34553, #28702 ) ) ;
#20475 = PLANE ( 'NONE',  #30406 ) ;
#20476 = DIRECTION ( 'NONE',  ( 1.000000000000000000, -0.000000000000000000, -0.000000000000000000 ) ) ;
#20477 = VECTOR ( 'NONE', #17117, 1000.000000000000000 ) ;
#20478 = ITEM_DEFINED_TRANSFORMATION ( 'NONE', 'NONE', #4728,  #28566 ) ;
#20480 = CARTESIAN_POINT ( 'NONE',  ( 11.99999999999999645, 124.9999999999999716, 187.0000000000000000 ) ) ;
#20479 = CARTESIAN_POINT ( 'NONE',  ( 2.606461852600250317, 25.37843598539274126, 19.93397194544903073 ) ) ;
#20481 = ORIENTED_EDGE ( 'NONE', *, *, #33947, .F. ) ;
#20482 = ORIENTED_EDGE ( 'NONE', *, *, #25983, .F. ) ;
#20483 = DIRECTION ( 'NONE',  ( -1.000000000000000000, -0.000000000000000000, -0.000000000000000000 ) ) ;
#20484 = DIRECTION ( 'NONE',  ( -0.000000000000000000, 1.000000000000000000, -0.000000000000000000 ) ) ;
#20485 = FACE_OUTER_BOUND ( 'NONE', #9398, .T. ) ;
#20486 = ORIENTED_EDGE ( 'NONE', *, *, #12465, .F. ) ;
#20487 = EDGE_CURVE ( 'NONE', #21040, #28354, #2679, .T. ) ;
#20488 = EDGE_CURVE ( 'NONE', #5474, #25766, #18662, .T. ) ;
#20489 = CARTESIAN_POINT ( 'NONE',  ( -5.038454199367317976, -32.15304576796696523, 68.31122994652405112 ) ) ;
#20490 = EDGE_LOOP ( 'NONE', ( #29786, #9693, #33946, #31878, #34450, #30111, #14490, #10196 ) ) ;
#20491 = CYLINDRICAL_SURFACE ( 'NONE', #25419, 7.999999999999979572 ) ;
#20492 = FILL_AREA_STYLE_COLOUR ( '', #18297 ) ;
#20493 = ADVANCED_FACE ( 'NONE', ( #21137 ), #23454, .T. ) ;
#20494 = CARTESIAN_POINT ( 'NONE',  ( 1.749999999999999778, 28.00026196654270905, 20.00929742917132970 ) ) ;
#20496 = LINE ( 'NONE', #15698, #17424 ) ;
#20495 = CARTESIAN_POINT ( 'NONE',  ( 4.979875012683824487, -33.69708579775584667, -36.68877005347592757 ) ) ;
#20498 = EDGE_CURVE ( 'NONE', #33253, #29665, #14653, .T. ) ;
#20497 = CARTESIAN_POINT ( 'NONE',  ( 34.14795412574902400, 16.36947364650383818, 68.31122994652405112 ) ) ;
#20499 = CARTESIAN_POINT ( 'NONE',  ( -4.875000000000000000, 2.702098422956710877, -0.7500000000000000000 ) ) ;
#20500 = DIRECTION ( 'NONE',  ( 0.000000000000000000, -1.000000000000000000, 0.000000000000000000 ) ) ;
#20501 = CIRCLE ( 'NONE', #3514, 32.54542015209057126 ) ;
#20502 = CIRCLE ( 'NONE', #30742, 7.999999999999979572 ) ;
#20503 = ORIENTED_EDGE ( 'NONE', *, *, #21100, .F. ) ;
#20504 = ORIENTED_EDGE ( 'NONE', *, *, #7802, .T. ) ;
#20505 = ORIENTED_EDGE ( 'NONE', *, *, #14167, .T. ) ;
#20506 = AXIS2_PLACEMENT_3D ( 'NONE', #21493, #782, #24974 ) ;
#20507 = FACE_OUTER_BOUND ( 'NONE', #25906, .T. ) ;
#20508 = AXIS2_PLACEMENT_3D ( 'NONE', #12417, #12582, #9900 ) ;
#20509 = VERTEX_POINT ( 'NONE', #9932 ) ;
#20510 = AXIS2_PLACEMENT_3D ( 'NONE', #33937, #28768, #31780 ) ;
#20511 = ORIENTED_EDGE ( 'NONE', *, *, #18281, .F. ) ;
#20512 = ORIENTED_EDGE ( 'NONE', *, *, #27413, .T. ) ;
#20513 = EDGE_CURVE ( 'NONE', #16209, #10508, #15159, .T. ) ;
#20514 = LINE ( 'NONE', #31536, #33839 ) ;
#20515 = ORIENTED_EDGE ( 'NONE', *, *, #6355, .T. ) ;
#20516 = CARTESIAN_POINT ( 'NONE',  ( 35.63428259149704758, -12.79065496477508823, 68.31122994652405112 ) ) ;
#20517 = FACE_OUTER_BOUND ( 'NONE', #17906, .T. ) ;
#20518 = ORIENTED_EDGE ( 'NONE', *, *, #7901, .T. ) ;
#20519 = VERTEX_POINT ( 'NONE', #20965 ) ;
#20520 = LINE ( 'NONE', #4132, #7729 ) ;
#20521 = CARTESIAN_POINT ( 'NONE',  ( 1.039999999999999591, -30.28730148581173864, 16.34215476954022606 ) ) ;
#20522 = EDGE_CURVE ( 'NONE', #32414, #6402, #29418, .T. ) ;
#20523 = DIRECTION ( 'NONE',  ( -0.000000000000000000, -0.000000000000000000, -1.000000000000000000 ) ) ;
#20524 = DIRECTION ( 'NONE',  ( -1.000000000000000000, -0.000000000000000000, 0.000000000000000000 ) ) ;
#20525 = PLANE ( 'NONE',  #21104 ) ;
#20526 = EDGE_LOOP ( 'NONE', ( #1906, #24159, #28632, #14837 ) ) ;
#20527 = CIRCLE ( 'NONE', #1766, 30.47050528711511674 ) ;
#20528 = EDGE_CURVE ( 'NONE', #6277, #15141, #12966, .T. ) ;
#20529 = LINE ( 'NONE', #23368, #4953 ) ;
#20530 = CARTESIAN_POINT ( 'NONE',  ( 5.510910596163087978E-15, 45.00000000000000711, -85.22165320886809070 ) ) ;
#20531 = EDGE_CURVE ( 'NONE', #26588, #25102, #18493, .T. ) ;
#20532 = DIRECTION ( 'NONE',  ( 0.000000000000000000, 0.000000000000000000, 1.000000000000000000 ) ) ;
#20533 = VERTEX_POINT ( 'NONE', #26652 ) ;
#20534 = CARTESIAN_POINT ( 'NONE',  ( -410.0000000000000568, -104.9999999999999716, -187.0000000000000000 ) ) ;
#20535 = DIRECTION ( 'NONE',  ( -0.9476531711828025673, 0.3193015301359797831, 5.865473952658197586E-17 ) ) ;
#20536 = LINE ( 'NONE', #8222, #12718 ) ;
#20537 = CARTESIAN_POINT ( 'NONE',  ( 107.5878283054233293, 5.134660333356495521, -5.470525374126623319 ) ) ;
#20539 = CARTESIAN_POINT ( 'NONE',  ( -110.1150203881707910, 3.829664765295703645E-16, -7.500000000000000000 ) ) ;
#20538 = DIRECTION ( 'NONE',  ( -0.000000000000000000, -0.000000000000000000, 1.000000000000000000 ) ) ;
#20540 = AXIS2_PLACEMENT_3D ( 'NONE', #17315, #20660, #6769 ) ;
#20541 = VECTOR ( 'NONE', #16752, 1000.000000000000000 ) ;
#20542 = DIRECTION ( 'NONE',  ( 0.000000000000000000, 1.000000000000000000, 0.000000000000000000 ) ) ;
#20544 = ORIENTED_EDGE ( 'NONE', *, *, #18078, .F. ) ;
#20543 = AXIS2_PLACEMENT_3D ( 'NONE', #8994, #19865, #17559 ) ;
#20546 = PRESENTATION_LAYER_ASSIGNMENT (  '', '', ( #651 ) ) ;
#20545 = DIRECTION ( 'NONE',  ( 0.000000000000000000, -0.7071067811865489050, -0.7071067811865462405 ) ) ;
#20548 = CARTESIAN_POINT ( 'NONE',  ( -363.0000000000000000, 124.9999999999999432, 168.9999999999999716 ) ) ;
#20547 = DIRECTION ( 'NONE',  ( 1.232595164407830946E-32, 0.000000000000000000, 1.000000000000000000 ) ) ;
#20549 = ORIENTED_EDGE ( 'NONE', *, *, #7630, .T. ) ;
#20550 = CARTESIAN_POINT ( 'NONE',  ( -12.00000000000006573, -145.0000000000000000, -194.9999999999999432 ) ) ;
#20551 = AXIS2_PLACEMENT_3D ( 'NONE', #24054, #24235, #31525 ) ;
#20552 = ORIENTED_EDGE ( 'NONE', *, *, #21125, .T. ) ;
#20553 = CONICAL_SURFACE ( 'NONE', #23391, 2.499999999999825473, 0.7853981633974538301 ) ;
#20554 =( REPRESENTATION_RELATIONSHIP ('NONE','NONE', #23037, #1195 ) REPRESENTATION_RELATIONSHIP_WITH_TRANSFORMATION ( #4257 )SHAPE_REPRESENTATION_RELATIONSHIP( ) );
#20555 = ORIENTED_EDGE ( 'NONE', *, *, #21210, .F. ) ;
#20556 = CARTESIAN_POINT ( 'NONE',  ( -20.00000000000007461, 112.9999999999999574, -190.9999999999999716 ) ) ;
#20557 = ORIENTED_EDGE ( 'NONE', *, *, #27717, .T. ) ;
#20558 = EDGE_LOOP ( 'NONE', ( #11632, #25571, #2225, #20503 ) ) ;
#20559 = CARTESIAN_POINT ( 'NONE',  ( 22.89764159710615132, -5.651112684911597128, -77.50000000000000000 ) ) ;
#20560 = PRODUCT_DEFINITION_SHAPE ( 'NONE', 'NONE',  #35150 ) ;
#20561 = FACE_OUTER_BOUND ( 'NONE', #22670, .T. ) ;
#20562 = DIRECTION ( 'NONE',  ( -1.000000000000000000, 0.000000000000000000, 0.000000000000000000 ) ) ;
#20563 = EDGE_LOOP ( 'NONE', ( #28441, #15220, #2926, #12479 ) ) ;
#20564 = EDGE_LOOP ( 'NONE', ( #880, #24190, #20029, #11654 ) ) ;
#20565 = AXIS2_PLACEMENT_3D ( 'NONE', #12074, #11537, #25034 ) ;
#20566 = EDGE_CURVE ( 'NONE', #16065, #28035, #2262, .T. ) ;
#20567 = DIRECTION ( 'NONE',  ( 0.000000000000000000, 3.374343856708137958E-53, -1.000000000000000000 ) ) ;
#20568 = DIRECTION ( 'NONE',  ( -3.040835319149746528E-31, -1.000000000000000000, 0.000000000000000000 ) ) ;
#20569 = VECTOR ( 'NONE', #23227, 1000.000000000000000 ) ;
#20570 = AXIS2_PLACEMENT_3D ( 'NONE', #17282, #20114, #17100 ) ;
#20571 = CARTESIAN_POINT ( 'NONE',  ( 0.000000000000000000, 0.000000000000000000, 0.000000000000000000 ) ) ;
#20572 = EDGE_CURVE ( 'NONE', #32765, #28025, #22018, .T. ) ;
#20573 = CARTESIAN_POINT ( 'NONE',  ( 2.790000000000083524, -30.61525927030270822, 1.705757817505451523 ) ) ;
#20574 = DIRECTION ( 'NONE',  ( 1.000000000000000000, 0.000000000000000000, 1.300283923313630633E-47 ) ) ;
#20575 = ORIENTED_EDGE ( 'NONE', *, *, #31080, .T. ) ;
#20576 = PLANE ( 'NONE',  #27589 ) ;
#20577 = ADVANCED_FACE ( 'NONE', ( #16344 ), #22192, .F. ) ;
#20578 = DIRECTION ( 'NONE',  ( -1.000000000000000000, 0.000000000000000000, 0.000000000000000000 ) ) ;
#20579 = ORIENTED_EDGE ( 'NONE', *, *, #11507, .T. ) ;
#20580 = EDGE_CURVE ( 'NONE', #21426, #27971, #8654, .T. ) ;
#20581 = CARTESIAN_POINT ( 'NONE',  ( -5.038454199367317088, -32.15304576796697233, 68.31122994652405112 ) ) ;
#20582 = CARTESIAN_POINT ( 'NONE',  ( 0.000000000000000000, 0.000000000000000000, 0.000000000000000000 ) ) ;
#20583 = AXIS2_PLACEMENT_3D ( 'NONE', #8832, #33393, #12232 ) ;
#20584 = DIRECTION ( 'NONE',  ( 0.000000000000000000, -1.000000000000000000, 3.421138828918010427E-49 ) ) ;
#20585 = ORIENTED_EDGE ( 'NONE', *, *, #6889, .F. ) ;
#20586 = DIRECTION ( 'NONE',  ( 0.000000000000000000, -1.000000000000000000, 0.000000000000000000 ) ) ;
#20587 = ORIENTED_EDGE ( 'NONE', *, *, #34135, .T. ) ;
#20588 = CARTESIAN_POINT ( 'NONE',  ( 0.000000000000000000, 6.992329373473909019E-15, 49.43553178847298568 ) ) ;
#20589 = DIRECTION ( 'NONE',  ( 1.000000000000000000, 3.469446951953834515E-18, 0.000000000000000000 ) ) ;
#20590 = EDGE_CURVE ( 'NONE', #4766, #8764, #126, .T. ) ;
#20591 = VECTOR ( 'NONE', #13671, 1000.000000000000114 ) ;
#20593 = ORIENTED_EDGE ( 'NONE', *, *, #28915, .F. ) ;
#20592 = VECTOR ( 'NONE', #8615, 1000.000000000000000 ) ;
#20594 = AXIS2_PLACEMENT_3D ( 'NONE', #13808, #26977, #24118 ) ;
#20595 = CARTESIAN_POINT ( 'NONE',  ( 0.000000000000000000, 3.172845296185191895E-14, -85.22165320886810491 ) ) ;
#20596 = FACE_OUTER_BOUND ( 'NONE', #15624, .T. ) ;
#20597 = ORIENTED_EDGE ( 'NONE', *, *, #31544, .F. ) ;
#20598 = DIRECTION ( 'NONE',  ( -0.9802816614883508306, -0.1976053241935505356, -3.235836659273368021E-14 ) ) ;
#20599 = EDGE_LOOP ( 'NONE', ( #17885, #3358, #6619, #22965 ) ) ;
#20600 = CARTESIAN_POINT ( 'NONE',  ( 99.26191511054629757, -0.3789272201562040587, 12.50000000000000178 ) ) ;
#20601 = EDGE_LOOP ( 'NONE', ( #15755, #2450, #7410, #32445, #30881, #16371, #33306, #6442 ) ) ;
#20602 = DIRECTION ( 'NONE',  ( 0.000000000000000000, 1.000000000000000000, 1.224646799147353207E-16 ) ) ;
#20603 = CARTESIAN_POINT ( 'NONE',  ( 212.5000000000000000, 0.000000000000000000, 0.000000000000000000 ) ) ;
#20604 = CARTESIAN_POINT ( 'NONE',  ( 0.1835381808019326266, -27.67670874042560669, 16.59602520068856180 ) ) ;
#20605 = CARTESIAN_POINT ( 'NONE',  ( 129.3530333899765594, 6.000000000000000000, 62.49999999999999289 ) ) ;
#20606 = CONTEXT_DEPENDENT_SHAPE_REPRESENTATION ( #21494, #12616 ) ;
#20607 = ORIENTED_EDGE ( 'NONE', *, *, #27436, .F. ) ;
#20608 = ORIENTED_EDGE ( 'NONE', *, *, #2089, .T. ) ;
#20609 = EDGE_LOOP ( 'NONE', ( #7934, #17231, #33199, #1692 ) ) ;
#20610 = PRODUCT_DEFINITION_SHAPE ( 'NONE', 'NONE',  #35117 ) ;
#20611 = PLANE ( 'NONE',  #6674 ) ;
#20612 = EDGE_CURVE ( 'NONE', #23038, #26511, #5454, .T. ) ;
#20613 = LINE ( 'NONE', #2259, #31293 ) ;
#20614 = AXIS2_PLACEMENT_3D ( 'NONE', #13246, #32795, #24423 ) ;
#20615 = DIRECTION ( 'NONE',  ( 3.697785493223492838E-32, 1.934419779023891545E-16, -1.000000000000000000 ) ) ;
#20616 = DIRECTION ( 'NONE',  ( 1.000000000000000000, 0.000000000000000000, 5.546364386991661285E-52 ) ) ;
#20617 = CIRCLE ( 'NONE', #34852, 2.036051781435508801 ) ;
#20618 = AXIS2_PLACEMENT_3D ( 'NONE', #20891, #28728, #15217 ) ;
#20619 = DIRECTION ( 'NONE',  ( 0.000000000000000000, 1.310824597558155437E-49, 1.000000000000000000 ) ) ;
#20620 = VECTOR ( 'NONE', #16170, 1000.000000000000000 ) ;
#20621 = CARTESIAN_POINT ( 'NONE',  ( 0.000000000000000000, 0.000000000000000000, 0.000000000000000000 ) ) ;
#20622 = EDGE_LOOP ( 'NONE', ( #13127, #22542, #8085, #351 ) ) ;
#20623 = ADVANCED_FACE ( 'NONE', ( #8129 ), #10983, .T. ) ;
#20624 = EDGE_CURVE ( 'NONE', #5775, #32496, #5619, .T. ) ;
#20625 = CARTESIAN_POINT ( 'NONE',  ( 0.5288002434240788308, 31.32081674369885960, -11.57089561809639733 ) ) ;
#20626 = EDGE_LOOP ( 'NONE', ( #2935, #27326, #29066, #11888 ) ) ;
#20627 = EDGE_CURVE ( 'NONE', #23024, #501, #11345, .T. ) ;
#20628 = ADVANCED_FACE ( 'NONE', ( #19354 ), #3317, .T. ) ;
#20629 = DIRECTION ( 'NONE',  ( 0.000000000000000000, 0.000000000000000000, 1.000000000000000000 ) ) ;
#20630 = VERTEX_POINT ( 'NONE', #35029 ) ;
#20631 = LINE ( 'NONE', #6741, #26248 ) ;
#20632 = DIRECTION ( 'NONE',  ( 0.000000000000000000, 0.000000000000000000, 1.000000000000000000 ) ) ;
#20633 = DIRECTION ( 'NONE',  ( 0.000000000000000000, 0.000000000000000000, 1.000000000000000000 ) ) ;
#20634 = FACE_OUTER_BOUND ( 'NONE', #16388, .T. ) ;
#20635 = CARTESIAN_POINT ( 'NONE',  ( 129.3530333899765594, 6.000000000000000000, 57.49999999999999289 ) ) ;
#20637 = ADVANCED_FACE ( 'NONE', ( #30194 ), #21495, .T. ) ;
#20636 = VERTEX_POINT ( 'NONE', #32686 ) ;
#20638 = AXIS2_PLACEMENT_3D ( 'NONE', #26538, #29741, #13380 ) ;
#20640 = ORIENTED_EDGE ( 'NONE', *, *, #14231, .F. ) ;
#20639 = B_SPLINE_CURVE_WITH_KNOTS ( 'NONE', 3,
 ( #27662, #2921, #447, #32644 ),
 .UNSPECIFIED., .F., .F.,
 ( 4, 4 ),
 ( 0.005298356295608612834, 0.005985224943342816982 ),
 .UNSPECIFIED. ) ;
#20641 = CIRCLE ( 'NONE', #8687, 2.036051781435517682 ) ;
#20642 = DIRECTION ( 'NONE',  ( -3.375645805091040053E-14, -5.156639094876775151E-14, 0.9999999999999998890 ) ) ;
#20643 = VECTOR ( 'NONE', #6287, 1000.000000000000000 ) ;
#20644 = ORIENTED_EDGE ( 'NONE', *, *, #32845, .F. ) ;
#20645 = CARTESIAN_POINT ( 'NONE',  ( 0.000000000000000000, -32.54542015209051442, -87.50000000000000000 ) ) ;
#20646 = CARTESIAN_POINT ( 'NONE',  ( 2.765921099433441999, -3.506335382740735529, 30.89238256715863784 ) ) ;
#20647 = CARTESIAN_POINT ( 'NONE',  ( 108.4960439411449897, -4.564063043377788453, 5.956988494001920209 ) ) ;
#20648 = ITEM_DEFINED_TRANSFORMATION ( 'NONE', 'NONE', #33686,  #28566 ) ;
#20649 = ORIENTED_EDGE ( 'NONE', *, *, #19604, .T. ) ;
#20650 = CARTESIAN_POINT ( 'NONE',  ( -12.00000000000001066, -145.0000000000000000, 187.0000000000000000 ) ) ;
#20651 = LINE ( 'NONE', #18003, #30615 ) ;
#20652 = VECTOR ( 'NONE', #3802, 1000.000000000000000 ) ;
#20654 = CARTESIAN_POINT ( 'NONE',  ( 2.765921099433441999, -3.506335382740735529, 30.89238256715863784 ) ) ;
#20653 = CARTESIAN_POINT ( 'NONE',  ( -418.0000000000000000, -145.0000000000000000, -155.0000000000000000 ) ) ;
#20655 = ORIENTED_EDGE ( 'NONE', *, *, #8191, .T. ) ;
#20656 = ORIENTED_EDGE ( 'NONE', *, *, #19838, .T. ) ;
#20657 = DIRECTION ( 'NONE',  ( 0.000000000000000000, 0.000000000000000000, -1.000000000000000000 ) ) ;
#20658 = ORIENTED_EDGE ( 'NONE', *, *, #34359, .T. ) ;
#20659 = CARTESIAN_POINT ( 'NONE',  ( -445.9999999999999432, 105.0000000000000142, 107.9999999999999858 ) ) ;
#20660 = DIRECTION ( 'NONE',  ( 0.000000000000000000, 1.000000000000000000, -2.465190328815661892E-32 ) ) ;
#20661 = VERTEX_POINT ( 'NONE', #16875 ) ;
#20662 = AXIS2_PLACEMENT_3D ( 'NONE', #31311, #14962, #4419 ) ;
#20663 = CARTESIAN_POINT ( 'NONE',  ( -37.71145559917817280, 3.353962854566121088, -15.81122994652406355 ) ) ;
#20664 = VECTOR ( 'NONE', #31394, 1000.000000000000114 ) ;
#20665 = EDGE_CURVE ( 'NONE', #18227, #20630, #14012, .T. ) ;
#20666 = EDGE_CURVE ( 'NONE', #16671, #20721, #1572, .T. ) ;
#20667 = PRODUCT_DEFINITION_SHAPE ( 'NONE', 'NONE',  #35209 ) ;
#20668 = VERTEX_POINT ( 'NONE', #29854 ) ;
#20669 = CARTESIAN_POINT ( 'NONE',  ( 0.000000000000000000, 3.524919873834583163E-15, 68.31122994652405112 ) ) ;
#20670 = FACE_OUTER_BOUND ( 'NONE', #25482, .T. ) ;
#20671 = CARTESIAN_POINT ( 'NONE',  ( 0.02407890056655695096, 30.61125888652969707, -5.439165181698684570 ) ) ;
#20673 = CARTESIAN_POINT ( 'NONE',  ( -20.72055270933794446, 25.09707290294329951, 68.31122994652405112 ) ) ;
#20672 = CARTESIAN_POINT ( 'NONE',  ( 2.789999999999999147, 17.11426446101236820, -24.44276559937708271 ) ) ;
#20674 = DIRECTION ( 'NONE',  ( -0.4198891015602644883, -0.9075754196709571175, -0.000000000000000000 ) ) ;
#20675 = CARTESIAN_POINT ( 'NONE',  ( 0.000000000000000000, 11.69134295108991140, -6.750000000000015987 ) ) ;
#20676 = CARTESIAN_POINT ( 'NONE',  ( -418.0000000000000000, 109.0000000000000142, -155.0000000000000000 ) ) ;
#20677 = EDGE_CURVE ( 'NONE', #4360, #30105, #27526, .T. ) ;
#20678 = AXIS2_PLACEMENT_3D ( 'NONE', #24872, #29879, #5819 ) ;
#20679 = ORIENTED_EDGE ( 'NONE', *, *, #32440, .T. ) ;
#20680 = EDGE_LOOP ( 'NONE', ( #13847, #14828, #3573, #11646, #26317, #3955, #20710, #3256 ) ) ;
#20682 = VERTEX_POINT ( 'NONE', #11655 ) ;
#20681 = ADVANCED_FACE ( 'NONE', ( #27342 ), #3139, .F. ) ;
#20683 = EDGE_CURVE ( 'NONE', #11568, #24757, #29674, .T. ) ;
#20684 = AXIS2_PLACEMENT_3D ( 'NONE', #1892, #26631, #23791 ) ;
#20685 = EDGE_CURVE ( 'NONE', #25215, #29230, #427, .T. ) ;
#20686 = VECTOR ( 'NONE', #22656, 1000.000000000000000 ) ;
#20687 = DIRECTION ( 'NONE',  ( 0.000000000000000000, 0.000000000000000000, 1.000000000000000000 ) ) ;
#20688 = AXIS2_PLACEMENT_3D ( 'NONE', #30436, #23137, #23648 ) ;
#20689 = ORIENTED_EDGE ( 'NONE', *, *, #5813, .T. ) ;
#20690 = ORIENTED_EDGE ( 'NONE', *, *, #23141, .T. ) ;
#20691 = ORIENTED_EDGE ( 'NONE', *, *, #26475, .F. ) ;
#20692 = CARTESIAN_POINT ( 'NONE',  ( -414.0000000000000568, 137.0000000000000000, 154.9999999999999716 ) ) ;
#20693 = EDGE_CURVE ( 'NONE', #6940, #25387, #19010, .T. ) ;
#20694 = CONTEXT_DEPENDENT_SHAPE_REPRESENTATION ( #26727, #1616 ) ;
#20695 = EDGE_LOOP ( 'NONE', ( #810, #4457, #5119, #14571 ) ) ;
#20696 = DIRECTION ( 'NONE',  ( 0.000000000000000000, 0.000000000000000000, 1.000000000000000000 ) ) ;
#20697 = PLANE ( 'NONE',  #11454 ) ;
#20698 = ORIENTED_EDGE ( 'NONE', *, *, #31273, .T. ) ;
#20699 = ORIENTED_EDGE ( 'NONE', *, *, #806, .T. ) ;
#20700 = CARTESIAN_POINT ( 'NONE',  ( 1.205771365940041306, -7.794228634059936489, 13.50000000000000000 ) ) ;
#20701 = CARTESIAN_POINT ( 'NONE',  ( -45.05956070192387841, -20.15143121711730245, 20.00000000000000000 ) ) ;
#20702 = DIRECTION ( 'NONE',  ( 0.000000000000000000, 0.000000000000000000, 1.000000000000000000 ) ) ;
#20703 = LINE ( 'NONE', #31550, #12568 ) ;
#20704 = CYLINDRICAL_SURFACE ( 'NONE', #29046, 10.00000000000000000 ) ;
#20705 = ORIENTED_EDGE ( 'NONE', *, *, #2133, .F. ) ;
#20706 = FACE_OUTER_BOUND ( 'NONE', #34784, .T. ) ;
#20707 = DIRECTION ( 'NONE',  ( 1.000000000000000000, 0.000000000000000000, 0.000000000000000000 ) ) ;
#20708 = AXIS2_PLACEMENT_3D ( 'NONE', #7400, #21478, #5436 ) ;
#20709 = CARTESIAN_POINT ( 'NONE',  ( -442.0000000000000000, -124.9999999999999716, 132.0000000000000000 ) ) ;
#20710 = ORIENTED_EDGE ( 'NONE', *, *, #9993, .F. ) ;
#20711 = AXIS2_PLACEMENT_3D ( 'NONE', #21264, #31590, #32112 ) ;
#20712 = CARTESIAN_POINT ( 'NONE',  ( 1.532562817202168137, 33.69708579775584667, 68.31122994652405112 ) ) ;
#20713 = DIRECTION ( 'NONE',  ( -0.000000000000000000, -1.000000000000000000, -0.000000000000000000 ) ) ;
#20714 = EDGE_CURVE ( 'NONE', #22911, #25849, #16452, .T. ) ;
#20715 = CARTESIAN_POINT ( 'NONE',  ( -499.9999999999999432, 112.9999999999999574, -159.0000000000000000 ) ) ;
#20717 = CARTESIAN_POINT ( 'NONE',  ( -108.3758620253048974, 3.856339488913134605, -6.437882550241565305 ) ) ;
#20716 = CARTESIAN_POINT ( 'NONE',  ( 1.749999999999999778, 0.000000000000000000, 0.000000000000000000 ) ) ;
#20718 = AXIS2_PLACEMENT_3D ( 'NONE', #30481, #19811, #13757 ) ;
#20719 = AXIS2_PLACEMENT_3D ( 'NONE', #10382, #10915, #24951 ) ;
#20720 = CYLINDRICAL_SURFACE ( 'NONE', #28636, 2.036051781435517682 ) ;
#20721 = VERTEX_POINT ( 'NONE', #34050 ) ;
#20722 = CARTESIAN_POINT ( 'NONE',  ( 108.5065519622470021, 4.557154561855114139, -11.64184170122661932 ) ) ;
#20724 = LINE ( 'NONE', #31568, #32195 ) ;
#20723 = CARTESIAN_POINT ( 'NONE',  ( 1.040000000000001368, 6.714005886385424837, -33.75364837705166110 ) ) ;
#20725 = CIRCLE ( 'NONE', #1932, 3.999999999999976019 ) ;
#20726 = EDGE_LOOP ( 'NONE', ( #14759, #19361, #16916 ) ) ;
#20727 = DIRECTION ( 'NONE',  ( 0.000000000000000000, -0.000000000000000000, -1.000000000000000000 ) ) ;
#20728 = VERTEX_POINT ( 'NONE', #25869 ) ;
#20729 = EDGE_CURVE ( 'NONE', #13520, #7715, #20529, .T. ) ;
#20730 = ADVANCED_FACE ( 'NONE', ( #31211 ), #26041, .T. ) ;
#20731 = VECTOR ( 'NONE', #34257, 1000.000000000000000 ) ;
#20732 = ORIENTED_EDGE ( 'NONE', *, *, #23047, .F. ) ;
#20733 = CARTESIAN_POINT ( 'NONE',  ( 2.123179190381537129, -33.69708579775584667, 49.43553178847298568 ) ) ;
#20734 = ORIENTED_EDGE ( 'NONE', *, *, #27031, .T. ) ;
#20735 = VERTEX_POINT ( 'NONE', #34228 ) ;
#20736 = CARTESIAN_POINT ( 'NONE',  ( -15.64512930492131382, -28.53829535743844659, -36.68877005347593467 ) ) ;
#20737 = AXIS2_PLACEMENT_3D ( 'NONE', #33965, #34309, #9930 ) ;
#20738 = CARTESIAN_POINT ( 'NONE',  ( 0.006871226506761134167, -7.987145637396054987, -29.81833655972106456 ) ) ;
#20739 = VECTOR ( 'NONE', #25210, 1000.000000000000000 ) ;
#20740 = PLANE ( 'NONE',  #7158 ) ;
#20741 = CARTESIAN_POINT ( 'NONE',  ( -349.0000000000000000, -125.0000000000000284, 166.9999999999999716 ) ) ;
#20742 = ORIENTED_EDGE ( 'NONE', *, *, #1524, .F. ) ;
#20743 = ORIENTED_EDGE ( 'NONE', *, *, #24854, .T. ) ;
#20744 = AXIS2_PLACEMENT_3D ( 'NONE', #5507, #3021, #34910 ) ;
#20745 = CARTESIAN_POINT ( 'NONE',  ( 0.5288002590641972533, 7.012902549147048248, -32.64503617578034778 ) ) ;
#20746 = LINE ( 'NONE', #18611, #18075 ) ;
#20747 = PLANE ( 'NONE',  #8974 ) ;
#20748 = CARTESIAN_POINT ( 'NONE',  ( -20.00000000000001776, -124.9999999999999432, -194.9999999999999432 ) ) ;
#20749 = CARTESIAN_POINT ( 'NONE',  ( 11.62236370382047745, -30.39942490923500529, 49.43553178847298568 ) ) ;
#20750 = EDGE_LOOP ( 'NONE', ( #18798, #25060, #27462, #457, #354, #26721, #9912, #12333 ) ) ;
#20751 = ORIENTED_EDGE ( 'NONE', *, *, #12397, .F. ) ;
#20752 = CARTESIAN_POINT ( 'NONE',  ( 2.789999999999999147, 29.94779062842794559, -5.619744560738758388 ) ) ;
#20753 = FACE_OUTER_BOUND ( 'NONE', #8737, .T. ) ;
#20754 = ORIENTED_EDGE ( 'NONE', *, *, #32523, .F. ) ;
#20755 = LINE ( 'NONE', #12756, #28150 ) ;
#20756 = CARTESIAN_POINT ( 'NONE',  ( 2.765921099433442887, -8.112136323389137260, 30.01377904834206589 ) ) ;
#20757 = FACE_BOUND ( 'NONE', #5720, .T. ) ;
#20758 = ORIENTED_EDGE ( 'NONE', *, *, #8700, .T. ) ;
#20759 = CARTESIAN_POINT ( 'NONE',  ( -27.76765758629847980, -16.97532223688792996, 68.31122994652405112 ) ) ;
#20760 = VERTEX_POINT ( 'NONE', #9505 ) ;
#20761 = CARTESIAN_POINT ( 'NONE',  ( -5.021133111224782120, 18.16264470403145026, -67.50000000000000000 ) ) ;
#20762 = AXIS2_PLACEMENT_3D ( 'NONE', #23925, #18262, #7730 ) ;
#20763 = LINE ( 'NONE', #31609, #27896 ) ;
#20764 = ORIENTED_EDGE ( 'NONE', *, *, #10486, .F. ) ;
#20765 = AXIS2_PLACEMENT_3D ( 'NONE', #13335, #5291, #13670 ) ;
#20766 = FACE_OUTER_BOUND ( 'NONE', #16882, .T. ) ;
#20767 = CARTESIAN_POINT ( 'NONE',  ( 2.789999999999999147, 2.005524111408653720, -29.35189292423236296 ) ) ;
#20768 = AXIS2_PLACEMENT_3D ( 'NONE', #11848, #3626, #978 ) ;
#20769 = EDGE_CURVE ( 'NONE', #8593, #5081, #6813, .T. ) ;
#20770 = ORIENTED_EDGE ( 'NONE', *, *, #16755, .T. ) ;
#20771 = ADVANCED_FACE ( 'NONE', ( #33701, #4139 ), #12524, .T. ) ;
#20772 = CARTESIAN_POINT ( 'NONE',  ( 827.6310116856627701, 959.0072173888904672, 1753.598338701303192 ) ) ;
#20773 = ORIENTED_EDGE ( 'NONE', *, *, #23109, .T. ) ;
#20774 = CARTESIAN_POINT ( 'NONE',  ( 105.3748796498063030, -5.728975534391926416, 11.10987307012756631 ) ) ;
#20775 = EDGE_CURVE ( 'NONE', #15499, #20760, #9841, .T. ) ;
#20776 = ORIENTED_EDGE ( 'NONE', *, *, #9970, .T. ) ;
#20777 = DIRECTION ( 'NONE',  ( 1.000000000000000000, 0.000000000000000000, 0.000000000000000000 ) ) ;
#20778 = DIRECTION ( 'NONE',  ( -0.000000000000000000, -1.836970198721029688E-16, 1.000000000000000000 ) ) ;
#20779 = AXIS2_PLACEMENT_3D ( 'NONE', #9620, #20310, #9453 ) ;
#20780 = CARTESIAN_POINT ( 'NONE',  ( -110.1150203881707910, -0.3503014826537210746, -7.500000000000000888 ) ) ;
#20781 = FACE_OUTER_BOUND ( 'NONE', #16167, .T. ) ;
#20782 = CONTEXT_DEPENDENT_SHAPE_REPRESENTATION ( #8283, #33328 ) ;
#20783 = ORIENTED_EDGE ( 'NONE', *, *, #7047, .T. ) ;
#20784 = VERTEX_POINT ( 'NONE', #6639 ) ;
#20785 = ORIENTED_EDGE ( 'NONE', *, *, #2968, .F. ) ;
#20786 = VECTOR ( 'NONE', #79, 1000.000000000000000 ) ;
#20787 = LINE ( 'NONE', #29504, #14258 ) ;
#20788 = DIRECTION ( 'NONE',  ( 1.000000000000000000, 0.000000000000000000, 0.000000000000000000 ) ) ;
#20789 = LINE ( 'NONE', #7591, #26163 ) ;
#20790 = CARTESIAN_POINT ( 'NONE',  ( 0.02407890056655738464, -27.96208973699912548, 13.59246946040177129 ) ) ;
#20791 = CARTESIAN_POINT ( 'NONE',  ( 2.789819856565905809, -25.83993731729781373, -16.24881338200996694 ) ) ;
#20792 = ORIENTED_EDGE ( 'NONE', *, *, #8747, .F. ) ;
#20793 = VECTOR ( 'NONE', #26745, 1000.000000000000000 ) ;
#20794 = B_SPLINE_CURVE_WITH_KNOTS ( 'NONE', 3,
 ( #16900, #16720, #3342, #14039, #14220, #22396 ),
 .UNSPECIFIED., .F., .F.,
 ( 4, 2, 4 ),
 ( 4.404817104921089305E-07, 0.001874269682437042228, 0.003748098883163592659 ),
 .UNSPECIFIED. ) ;
#20795 = CARTESIAN_POINT ( 'NONE',  ( 0.02407890056655695096, -21.56796757982795043, -22.39322359481629476 ) ) ;
#20796 = CARTESIAN_POINT ( 'NONE',  ( 0.07094832170561987672, 26.43909160613385723, -17.47815001432893922 ) ) ;
#20797 = PLANE ( 'NONE',  #24555 ) ;
#20798 = ORIENTED_EDGE ( 'NONE', *, *, #2238, .F. ) ;
#20799 = FACE_OUTER_BOUND ( 'NONE', #5429, .T. ) ;
#20800 = ORIENTED_EDGE ( 'NONE', *, *, #5450, .F. ) ;
#20801 = CARTESIAN_POINT ( 'NONE',  ( 29.44023756548697079, 13.87360028845406212, 49.43553178847298568 ) ) ;
#20802 = FACE_OUTER_BOUND ( 'NONE', #24467, .T. ) ;
#20803 = AXIS2_PLACEMENT_3D ( 'NONE', #31205, #4475, #12347 ) ;
#20804 = DIRECTION ( 'NONE',  ( -1.000000000000000000, -0.000000000000000000, 0.000000000000000000 ) ) ;
#20805 = DIRECTION ( 'NONE',  ( 1.000000000000000000, 0.000000000000000000, -1.848892746611746966E-32 ) ) ;
#20806 = CARTESIAN_POINT ( 'NONE',  ( -442.0000000000000000, 137.0000000000000000, -155.0000000000000000 ) ) ;
#20807 = AXIS2_PLACEMENT_3D ( 'NONE', #5103, #24488, #4747 ) ;
#20808 = ADVANCED_FACE ( 'NONE', ( #20706 ), #28372, .F. ) ;
#20809 = ORIENTED_EDGE ( 'NONE', *, *, #22098, .F. ) ;
#20810 = ORIENTED_EDGE ( 'NONE', *, *, #22356, .F. ) ;
#20811 = DIRECTION ( 'NONE',  ( -7.893605728314050488E-14, 1.618803117314786135E-15, 0.9999999999999998890 ) ) ;
#20812 =( REPRESENTATION_RELATIONSHIP ('NONE','NONE', #23037, #28231 ) REPRESENTATION_RELATIONSHIP_WITH_TRANSFORMATION ( #24567 )SHAPE_REPRESENTATION_RELATIONSHIP( ) );
#20813 = ADVANCED_FACE ( 'NONE', ( #4312 ), #23208, .F. ) ;
#20814 = ORIENTED_EDGE ( 'NONE', *, *, #13751, .T. ) ;
#20815 = CIRCLE ( 'NONE', #33318, 3.999999999999948042 ) ;
#20816 = DIRECTION ( 'NONE',  ( -1.000000000000000000, -3.040835319149746528E-31, -1.232595164407830946E-32 ) ) ;
#20817 = CIRCLE ( 'NONE', #19135, 2.033421858999711951 ) ;
#20818 = CARTESIAN_POINT ( 'NONE',  ( 2.783107567989380193, -3.550547054313960338, 30.66493323461383369 ) ) ;
#20819 = CARTESIAN_POINT ( 'NONE',  ( 110.1062604042073474, -2.624171310066655938, 7.028111897042786715 ) ) ;
#20820 = ADVANCED_FACE ( 'NONE', ( #14856 ), #25688, .T. ) ;
#20821 = ORIENTED_EDGE ( 'NONE', *, *, #2412, .F. ) ;
#20822 = DIRECTION ( 'NONE',  ( 1.000000000000000000, 0.000000000000000000, -0.000000000000000000 ) ) ;
#20823 = ADVANCED_FACE ( 'NONE', ( #22855 ), #27116, .T. ) ;
#20824 = VECTOR ( 'NONE', #11607, 1000.000000000000000 ) ;
#20826 = CARTESIAN_POINT ( 'NONE',  ( -31.87924797510909869, -6.551177101682105430, -36.68877005347593467 ) ) ;
#20825 = DIRECTION ( 'NONE',  ( 1.000000000000000000, 0.000000000000000000, -1.848892746611746966E-32 ) ) ;
#20827 = VERTEX_POINT ( 'NONE', #28883 ) ;
#20828 = VERTEX_POINT ( 'NONE', #9322 ) ;
#20829 = CARTESIAN_POINT ( 'NONE',  ( 0.000000000000000000, 0.000000000000000000, -0.7500000000000000000 ) ) ;
#20830 = EDGE_LOOP ( 'NONE', ( #4826, #31675, #7141, #31841, #22064 ) ) ;
#20831 = AXIS2_PLACEMENT_3D ( 'NONE', #11702, #27529, #11884 ) ;
#20832 = CARTESIAN_POINT ( 'NONE',  ( -145.0000000000000568, -88.29863524074325198, -74.12844257252345415 ) ) ;
#20833 = LINE ( 'NONE', #7645, #27358 ) ;
#20834 = VERTEX_POINT ( 'NONE', #6988 ) ;
#20835 = CARTESIAN_POINT ( 'NONE',  ( 105.0000000000000000, 0.000000000000000000, 60.00000000000000000 ) ) ;
#20836 = ORIENTED_EDGE ( 'NONE', *, *, #3591, .T. ) ;
#20837 = VECTOR ( 'NONE', #10384, 1000.000000000000000 ) ;
#20838 = DIRECTION ( 'NONE',  ( 0.000000000000000000, 0.000000000000000000, -1.000000000000000000 ) ) ;
#20839 = DIRECTION ( 'NONE',  ( 1.000000000000000000, 0.000000000000000000, 0.000000000000000000 ) ) ;
#20841 = LINE ( 'NONE', #4801, #11149 ) ;
#20840 = PLANE ( 'NONE',  #26415 ) ;
#20842 = DIRECTION ( 'NONE',  ( 1.000000000000000000, 0.000000000000000000, 0.000000000000000000 ) ) ;
#20843 = CARTESIAN_POINT ( 'NONE',  ( -105.0000000000000000, 0.000000000000000000, 57.49999999999999289 ) ) ;
#20844 = LINE ( 'NONE', #9988, #26958 ) ;
#20845 = CARTESIAN_POINT ( 'NONE',  ( 22.89764159710615132, -3.615060903476079890, -77.50000000000000000 ) ) ;
#20846 = PRODUCT_DEFINITION_SHAPE ( 'NONE', 'NONE',  #35178 ) ;
#20847 = AXIS2_PLACEMENT_3D ( 'NONE', #17498, #746, #3758 ) ;
#20848 = VECTOR ( 'NONE', #7993, 1000.000000000000227 ) ;
#20849 = ORIENTED_EDGE ( 'NONE', *, *, #29812, .T. ) ;
#20850 =( LENGTH_UNIT ( ) NAMED_UNIT ( * ) SI_UNIT ( .MILLI., .METRE. ) );
#20851 = ORIENTED_EDGE ( 'NONE', *, *, #17253, .F. ) ;
#20852 = VERTEX_POINT ( 'NONE', #15374 ) ;
#20853 = EDGE_CURVE ( 'NONE', #2524, #10873, #6663, .T. ) ;
#20854 = EDGE_CURVE ( 'NONE', #9586, #16454, #3815, .T. ) ;
#20855 = CARTESIAN_POINT ( 'NONE',  ( 109.5194798111833308, 3.554679846740550264, 6.612701241491620863 ) ) ;
#20856 = ADVANCED_FACE ( 'NONE', ( #31043 ), #31723, .T. ) ;
#20857 = CARTESIAN_POINT ( 'NONE',  ( 751.4997240610829294, 1334.697290463531999, 1678.876119909286899 ) ) ;
#20858 = VERTEX_POINT ( 'NONE', #23032 ) ;
#20859 = ORIENTED_EDGE ( 'NONE', *, *, #27911, .T. ) ;
#20860 = ORIENTED_EDGE ( 'NONE', *, *, #30493, .F. ) ;
#20861 = CARTESIAN_POINT ( 'NONE',  ( -37.69926482250235722, 3.578808500140865156, 68.31122994652405112 ) ) ;
#20862 = CONTEXT_DEPENDENT_SHAPE_REPRESENTATION ( #33543, #13933 ) ;
#20863 = ORIENTED_EDGE ( 'NONE', *, *, #2955, .F. ) ;
#20864 = DIRECTION ( 'NONE',  ( 1.000000000000000000, -0.000000000000000000, -0.000000000000000000 ) ) ;
#20865 = PLANE ( 'NONE',  #13164 ) ;
#20866 = ORIENTED_EDGE ( 'NONE', *, *, #25825, .F. ) ;
#20867 = ORIENTED_EDGE ( 'NONE', *, *, #30126, .F. ) ;
#20868 = CARTESIAN_POINT ( 'NONE',  ( 0.7561992193724378364, 5.833185478271599500, -33.40977515897095884 ) ) ;
#20869 = DIRECTION ( 'NONE',  ( -0.000000000000000000, -0.000000000000000000, -1.000000000000000000 ) ) ;
#20870 = CARTESIAN_POINT ( 'NONE',  ( 0.1835380176977702282, 30.42925477731472839, 10.74656554331707170 ) ) ;
#20872 = EDGE_CURVE ( 'NONE', #11484, #33608, #33884, .T. ) ;
#20871 = LINE ( 'NONE', #17535, #7430 ) ;
#20873 = CARTESIAN_POINT ( 'NONE',  ( 1.040000000000001812, -1.891117961019736393, -34.36292081097834483 ) ) ;
#20874 = EDGE_LOOP ( 'NONE', ( #6363, #32908, #12257, #16426 ) ) ;
#20876 = VECTOR ( 'NONE', #12794, 1000.000000000000000 ) ;
#20875 = DIRECTION ( 'NONE',  ( 1.000000000000000000, 0.000000000000000000, 0.000000000000000000 ) ) ;
#20877 = CARTESIAN_POINT ( 'NONE',  ( -349.0000000000000000, 124.9999999999999432, 181.0000000000000000 ) ) ;
#20878 = EDGE_LOOP ( 'NONE', ( #10082, #30140, #12175, #32351 ) ) ;
#20879 = CARTESIAN_POINT ( 'NONE',  ( 32.05156013847309993, -20.15193397489277771, 68.31122994652405112 ) ) ;
#20880 = ADVANCED_FACE ( 'NONE', ( #16078, #16258, #4652 ), #29762, .T. ) ;
#20881 = DIRECTION ( 'NONE',  ( 2.530127506375325574E-80, -1.000000000000000000, -6.842277657836020854E-49 ) ) ;
#20882 = CARTESIAN_POINT ( 'NONE',  ( 109.8329508816931366, 3.098707215121725422, -6.832002823648420708 ) ) ;
#20883 = VECTOR ( 'NONE', #15108, 1000.000000000000000 ) ;
#20885 = CARTESIAN_POINT ( 'NONE',  ( -109.4140444411644921, 2.605551551359102547, -7.039079951515507361 ) ) ;
#20884 = CARTESIAN_POINT ( 'NONE',  ( -355.0000000000000000, 114.9999999999999574, 113.9999999999999858 ) ) ;
#20886 = EDGE_CURVE ( 'NONE', #26364, #2476, #31660, .T. ) ;
#20887 = EDGE_CURVE ( 'NONE', #16498, #10319, #13054, .T. ) ;
#20888 = CARTESIAN_POINT ( 'NONE',  ( 2.789999999999999147, -20.92506858792740587, -22.14933852381698642 ) ) ;
#20889 = ORIENTED_EDGE ( 'NONE', *, *, #22948, .F. ) ;
#20890 = CARTESIAN_POINT ( 'NONE',  ( 102.4416090844097482, 5.149687040066283750, -11.39104704602383933 ) ) ;
#20892 = CARTESIAN_POINT ( 'NONE',  ( -35.55956070192387841, -17.65143121711728469, 14.30932821646982411 ) ) ;
#20891 = CARTESIAN_POINT ( 'NONE',  ( -70.00000000000000000, 4.559999999999908127, -172.9900000000000091 ) ) ;
#20893 = EDGE_CURVE ( 'NONE', #12400, #27222, #10197, .T. ) ;
#20894 = CIRCLE ( 'NONE', #23167, 9.999999999999994671 ) ;
#20895 = VERTEX_POINT ( 'NONE', #10368 ) ;
#20896 = FACE_OUTER_BOUND ( 'NONE', #20601, .T. ) ;
#20897 = ORIENTED_EDGE ( 'NONE', *, *, #175, .F. ) ;
#20898 = VECTOR ( 'NONE', #11084, 1000.000000000000000 ) ;
#20899 = AXIS2_PLACEMENT_3D ( 'NONE', #2669, #13889, #24376 ) ;
#20900 = EDGE_CURVE ( 'NONE', #26996, #8677, #3259, .T. ) ;
#20901 = ADVANCED_FACE ( 'NONE', ( #18399 ), #2348, .F. ) ;
#20902 = VERTEX_POINT ( 'NONE', #7689 ) ;
#20903 = DIRECTION ( 'NONE',  ( 0.000000000000000000, 0.000000000000000000, -1.000000000000000000 ) ) ;
#20904 = ORIENTED_EDGE ( 'NONE', *, *, #10859, .T. ) ;
#20905 = ORIENTED_EDGE ( 'NONE', *, *, #30814, .T. ) ;
#20906 = DIRECTION ( 'NONE',  ( 0.000000000000000000, 0.000000000000000000, 1.000000000000000000 ) ) ;
#20907 = CARTESIAN_POINT ( 'NONE',  ( 2.789999999999999147, -27.96208973699893008, -13.59246946040217630 ) ) ;
#20908 = CARTESIAN_POINT ( 'NONE',  ( 1.749999999999999778, 32.09669216789236401, 12.41728656686386500 ) ) ;
#20909 = ORIENTED_EDGE ( 'NONE', *, *, #22232, .F. ) ;
#20910 = VERTEX_POINT ( 'NONE', #29417 ) ;
#20911 = CARTESIAN_POINT ( 'NONE',  ( -9.410814080250917257, 36.67205378194066867, -36.68877005347593467 ) ) ;
#20912 = CARTESIAN_POINT ( 'NONE',  ( 10.00000000000000000, 0.000000000000000000, 0.000000000000000000 ) ) ;
#20913 = CARTESIAN_POINT ( 'NONE',  ( 3.235562306570555532E-30, 18.16264470403145026, -67.50000000000000000 ) ) ;
#20914 = DIRECTION ( 'NONE',  ( -0.000000000000000000, -0.000000000000000000, -1.000000000000000000 ) ) ;
#20915 = DIRECTION ( 'NONE',  ( 1.000000000000000000, 0.000000000000000000, 0.000000000000000000 ) ) ;
#20916 = UNCERTAINTY_MEASURE_WITH_UNIT (LENGTH_MEASURE( 1.000000000000000082E-05 ), #5764, 'distance_accuracy_value', 'NONE');
#20917 = ORIENTED_EDGE ( 'NONE', *, *, #25635, .T. ) ;
#20918 = ORIENTED_EDGE ( 'NONE', *, *, #22209, .T. ) ;
#20919 = FACE_OUTER_BOUND ( 'NONE', #16884, .T. ) ;
#20920 = AXIS2_PLACEMENT_3D ( 'NONE', #13603, #5398, #5565 ) ;
#20921 = CARTESIAN_POINT ( 'NONE',  ( -442.0000000000000000, -112.9999999999999858, -174.9999999999999716 ) ) ;
#20922 = VERTEX_POINT ( 'NONE', #34757 ) ;
#20923 = DIRECTION ( 'NONE',  ( 0.000000000000000000, -1.000000000000000000, -1.224646799147353207E-16 ) ) ;
#20924 = DIRECTION ( 'NONE',  ( -1.000000000000000000, 0.000000000000000000, -0.000000000000000000 ) ) ;
#20925 = DIRECTION ( 'NONE',  ( 1.000000000000000000, 3.040835319149746090E-31, 1.232595164407830946E-32 ) ) ;
#20926 = ORIENTED_EDGE ( 'NONE', *, *, #30453, .T. ) ;
#20927 = EDGE_CURVE ( 'NONE', #3499, #24998, #7804, .T. ) ;
#20928 = CARTESIAN_POINT ( 'NONE',  ( -20.00000000000004619, 124.9999999999999716, 155.0000000000000000 ) ) ;
#20929 = ORIENTED_EDGE ( 'NONE', *, *, #32824, .F. ) ;
#20930 = CIRCLE ( 'NONE', #23224, 4.750000000000004441 ) ;
#20931 = ADVANCED_FACE ( 'NONE', ( #21582 ), #18583, .T. ) ;
#20932 = VECTOR ( 'NONE', #25982, 1000.000000000000000 ) ;
#20933 = DIRECTION ( 'NONE',  ( 0.000000000000000000, 0.000000000000000000, -1.000000000000000000 ) ) ;
#20934 = ORIENTED_EDGE ( 'NONE', *, *, #20299, .T. ) ;
#20936 = DIRECTION ( 'NONE',  ( 0.000000000000000000, -6.870191984066554061E-16, -1.000000000000000000 ) ) ;
#20935 = FACE_OUTER_BOUND ( 'NONE', #18864, .T. ) ;
#20938 = B_SPLINE_CURVE_WITH_KNOTS ( 'NONE', 3,
 ( #30741, #3501, #28249, #498, #14390, #846, #8498, #3676, #6342, #11892, #11711, #3848, #28067, #25390, #14742, #11182, #22739, #22032, #32874, #19365, #30206, #5809, #16705, #27537, #23428, #34285, #33938, #29116, #20421, #15261, #1374, #17592, #28600, #12066, #15087, #18120, #7215, #34105 ),
 .UNSPECIFIED., .F., .F.,
 ( 4, 2, 2, 2, 2, 2, 2, 2, 2, 2, 2, 2, 2, 2, 2, 2, 2, 2, 4 ),
 ( 1.577487858758373578E-18, 0.001010717872208361260, 0.002021435744416721220, 0.003032153616625081396, 0.004042871488833440705, 0.005053589361041800447, 0.006064307233250161057, 0.006569666169354321412, 0.007075025105458481768, 0.008085742977666759979, 0.009096460849875040791, 0.01010717872208332160, 0.01111789659429160242, 0.01212861446649988323, 0.01313933233870816578, 0.01364469127481231572, 0.01415005021091646741, 0.01516076808312478118, 0.01617148595533309322 ),
 .UNSPECIFIED. ) ;
#20937 = CARTESIAN_POINT ( 'NONE',  ( 0.000000000000000000, 0.000000000000000000, 0.000000000000000000 ) ) ;
#20939 = AXIS2_PLACEMENT_3D ( 'NONE', #20701, #1310, #17533 ) ;
#20940 = ORIENTED_EDGE ( 'NONE', *, *, #26178, .F. ) ;
#20941 = CARTESIAN_POINT ( 'NONE',  ( -19.99999999999996092, -141.0000000000000000, 187.0000000000000000 ) ) ;
#20942 = EDGE_CURVE ( 'NONE', #7557, #169, #10900, .T. ) ;
#20943 = DIRECTION ( 'NONE',  ( 0.000000000000000000, 1.000000000000000000, -3.374343856708137958E-53 ) ) ;
#20944 = ORIENTED_EDGE ( 'NONE', *, *, #6523, .F. ) ;
#20945 = AXIS2_PLACEMENT_3D ( 'NONE', #24532, #8169, #8527 ) ;
#20946 = DIRECTION ( 'NONE',  ( -7.893605728314051750E-14, 1.618803117314786530E-15, 1.000000000000000000 ) ) ;
#20947 = ORIENTED_EDGE ( 'NONE', *, *, #2911, .F. ) ;
#20948 = LINE ( 'NONE', #34652, #3390 ) ;
#20949 = EDGE_LOOP ( 'NONE', ( #27707, #24008, #20122, #25422 ) ) ;
#20950 = CARTESIAN_POINT ( 'NONE',  ( 35.44043929807611448, -32.65143121711728469, 5.690671783530174999 ) ) ;
#20951 = CARTESIAN_POINT ( 'NONE',  ( 19.99999999999998934, 136.9999999999999716, 155.0000000000000000 ) ) ;
#20952 = VECTOR ( 'NONE', #23623, 1000.000000000000000 ) ;
#20953 = DIRECTION ( 'NONE',  ( 0.000000000000000000, -1.000000000000000000, 0.000000000000000000 ) ) ;
#20954 = PLANE ( 'NONE',  #15969 ) ;
#20955 = EDGE_LOOP ( 'NONE', ( #4735, #19049, #16542, #6006, #19324, #23383, #1840, #27599 ) ) ;
#20956 = ORIENTED_EDGE ( 'NONE', *, *, #21355, .F. ) ;
#20957 = PRODUCT_DEFINITION_SHAPE ( 'NONE', 'NONE',  #35208 ) ;
#20958 = ORIENTED_EDGE ( 'NONE', *, *, #28480, .T. ) ;
#20959 = EDGE_CURVE ( 'NONE', #11922, #9216, #15913, .T. ) ;
#20960 = CARTESIAN_POINT ( 'NONE',  ( 5.021133111224679091, 26.05646109878476224, -67.50000000000000000 ) ) ;
#20961 = CARTESIAN_POINT ( 'NONE',  ( 212.5000000000000000, 0.000000000000000000, 0.000000000000000000 ) ) ;
#20962 = AXIS2_PLACEMENT_3D ( 'NONE', #6687, #8837, #6151 ) ;
#20963 = DIRECTION ( 'NONE',  ( 0.000000000000000000, 1.836970198721029441E-16, -1.000000000000000000 ) ) ;
#20964 = CARTESIAN_POINT ( 'NONE',  ( -20.00000000000007461, -113.0000000000000000, -187.0000000000000000 ) ) ;
#20965 = CARTESIAN_POINT ( 'NONE',  ( 10.96230482721425403, -16.64466345897532662, -87.50000000000000000 ) ) ;
#20966 = FILL_AREA_STYLE ('',( #31467 ) ) ;
#20967 = ORIENTED_EDGE ( 'NONE', *, *, #34712, .T. ) ;
#20968 = ADVANCED_FACE ( 'NONE', ( #8042 ), #2182, .T. ) ;
#20969 = DIRECTION ( 'NONE',  ( -0.000000000000000000, -0.000000000000000000, -1.000000000000000000 ) ) ;
#20970 = PLANE ( 'NONE',  #34791 ) ;
#20971 = ADVANCED_FACE ( 'NONE', ( #21227 ), #32071, .F. ) ;
#20972 = LINE ( 'NONE', #10469, #30831 ) ;
#20973 = ORIENTED_EDGE ( 'NONE', *, *, #30172, .F. ) ;
#20974 = ADVANCED_FACE ( 'NONE', ( #26735 ), #27089, .F. ) ;
#20975 = VECTOR ( 'NONE', #15242, 1000.000000000000000 ) ;
#20976 = LINE ( 'NONE', #32177, #29173 ) ;
#20977 = ORIENTED_EDGE ( 'NONE', *, *, #4199, .T. ) ;
#20978 = DIRECTION ( 'NONE',  ( -1.000000000000000000, -0.000000000000000000, -0.000000000000000000 ) ) ;
#20979 = FACE_BOUND ( 'NONE', #32470, .T. ) ;
#20980 = AXIS2_PLACEMENT_3D ( 'NONE', #32846, #16506, #17217 ) ;
#20981 = VERTEX_POINT ( 'NONE', #29239 ) ;
#20982 = CARTESIAN_POINT ( 'NONE',  ( -361.0000000000000000, 124.9999999999999432, 185.0000000000000000 ) ) ;
#20983 = LINE ( 'NONE', #31651, #5380 ) ;
#20984 = DIRECTION ( 'NONE',  ( 0.000000000000000000, 0.000000000000000000, 1.000000000000000000 ) ) ;
#20985 = EDGE_LOOP ( 'NONE', ( #29135, #23054, #10001, #17088 ) ) ;
#20986 = AXIS2_PLACEMENT_3D ( 'NONE', #12405, #23415, #14901 ) ;
#20987 = EDGE_LOOP ( 'NONE', ( #9890, #23394, #21672, #6775 ) ) ;
#20988 = DIRECTION ( 'NONE',  ( -0.1063910735369017202, 0.9943243633099136947, -1.000770725407181676E-14 ) ) ;
#20989 = ORIENTED_EDGE ( 'NONE', *, *, #18077, .F. ) ;
#20990 = LINE ( 'NONE', #31828, #34567 ) ;
#20991 = VECTOR ( 'NONE', #4647, 1000.000000000000000 ) ;
#20992 = DIRECTION ( 'NONE',  ( 2.891205793294675861E-16, 0.000000000000000000, -1.000000000000000000 ) ) ;
#20993 = CARTESIAN_POINT ( 'NONE',  ( 104.0208154834590744, -5.657186516187210579, 4.924400946180165661 ) ) ;
#20994 = ITEM_DEFINED_TRANSFORMATION ( 'NONE', 'NONE', #4122,  #28566 ) ;
#20995 = ORIENTED_EDGE ( 'NONE', *, *, #18901, .T. ) ;
#20996 = LINE ( 'NONE', #4261, #20932 ) ;
#20998 = CARTESIAN_POINT ( 'NONE',  ( 2.789999999999999147, 24.25608676732976221, 18.39061402768369291 ) ) ;
#20997 = CARTESIAN_POINT ( 'NONE',  ( 2.789999999999999147, 18.59128259035472297, 24.91982945642928016 ) ) ;
#20999 = ORIENTED_EDGE ( 'NONE', *, *, #16173, .T. ) ;
#21000 = ORIENTED_EDGE ( 'NONE', *, *, #5123, .F. ) ;
#21001 = CARTESIAN_POINT ( 'NONE',  ( 12.00000000000001066, 144.9999999999999716, -154.9999999999999716 ) ) ;
#21002 = EDGE_CURVE ( 'NONE', #17675, #5983, #32272, .T. ) ;
#21003 = ORIENTED_EDGE ( 'NONE', *, *, #16365, .F. ) ;
#21004 = ADVANCED_FACE ( 'NONE', ( #32252 ), #2871, .T. ) ;
#21005 = DIRECTION ( 'NONE',  ( 0.000000000000000000, 0.000000000000000000, 1.000000000000000000 ) ) ;
#21006 = DIRECTION ( 'NONE',  ( 0.000000000000000000, 0.000000000000000000, 1.000000000000000000 ) ) ;
#21007 = EDGE_LOOP ( 'NONE', ( #7184, #33587, #32200, #17329 ) ) ;
#21008 = VECTOR ( 'NONE', #10441, 1000.000000000000114 ) ;
#21009 = CARTESIAN_POINT ( 'NONE',  ( 1.395000000000002238, -25.27164158951584838, 23.36088151536909763 ) ) ;
#21011 = EDGE_CURVE ( 'NONE', #29721, #30812, #6063, .T. ) ;
#21010 = B_SPLINE_CURVE_WITH_KNOTS ( 'NONE', 3,
 ( #14064, #19237, #11387, #25069 ),
 .UNSPECIFIED., .F., .F.,
 ( 4, 4 ),
 ( 0.005298347429621228476, 0.005985216133920623523 ),
 .UNSPECIFIED. ) ;
#21012 = ORIENTED_EDGE ( 'NONE', *, *, #9292, .T. ) ;
#21013 = EDGE_CURVE ( 'NONE', #7844, #14586, #22283, .T. ) ;
#21014 = CARTESIAN_POINT ( 'NONE',  ( 22.89764159710615132, -3.615060903476079890, -77.50000000000000000 ) ) ;
#21015 = DIRECTION ( 'NONE',  ( 1.000000000000000000, 0.000000000000000000, 0.000000000000000000 ) ) ;
#21016 = DIRECTION ( 'NONE',  ( 1.000000000000000000, 0.000000000000000000, 0.000000000000000000 ) ) ;
#21018 = PLANE ( 'NONE',  #27039 ) ;
#21017 = LINE ( 'NONE', #4979, #19052 ) ;
#21019 = AXIS2_PLACEMENT_3D ( 'NONE', #12836, #6938, #15154 ) ;
#21020 =( REPRESENTATION_RELATIONSHIP ('NONE','NONE', #23037, #28231 ) REPRESENTATION_RELATIONSHIP_WITH_TRANSFORMATION ( #8597 )SHAPE_REPRESENTATION_RELATIONSHIP( ) );
#21021 = CARTESIAN_POINT ( 'NONE',  ( -20.63749999999999574, 0.000000000000000000, 0.000000000000000000 ) ) ;
#21022 = LINE ( 'NONE', #15883, #14867 ) ;
#21023 = CARTESIAN_POINT ( 'NONE',  ( 15.99999999999998579, -55.00000000000000711, 0.000000000000000000 ) ) ;
#21024 = CARTESIAN_POINT ( 'NONE',  ( 2.789999999999999147, 2.005524111408653720, -29.35189292423236296 ) ) ;
#21025 = EDGE_CURVE ( 'NONE', #8593, #21855, #30586, .T. ) ;
#21026 = ORIENTED_EDGE ( 'NONE', *, *, #24615, .T. ) ;
#21027 = ORIENTED_EDGE ( 'NONE', *, *, #13064, .F. ) ;
#21028 = ORIENTED_EDGE ( 'NONE', *, *, #24987, .T. ) ;
#21029 = CARTESIAN_POINT ( 'NONE',  ( 107.5863203406750870, 5.135442232304142429, 5.469792608531489186 ) ) ;
#21030 = ORIENTED_EDGE ( 'NONE', *, *, #19293, .F. ) ;
#21031 = ORIENTED_EDGE ( 'NONE', *, *, #32221, .F. ) ;
#21032 = ORIENTED_EDGE ( 'NONE', *, *, #30453, .F. ) ;
#21033 = CARTESIAN_POINT ( 'NONE',  ( 2.789999999999999147, 19.87737664170488827, 23.05346671160913985 ) ) ;
#21034 = CARTESIAN_POINT ( 'NONE',  ( 0.7564103444947344324, -10.98355401466475811, 32.08778326629999356 ) ) ;
#21035 = CONTEXT_DEPENDENT_SHAPE_REPRESENTATION ( #14707, #4737 ) ;
#21036 = ORIENTED_EDGE ( 'NONE', *, *, #12534, .T. ) ;
#21037 = DIRECTION ( 'NONE',  ( 0.000000000000000000, 0.000000000000000000, -1.000000000000000000 ) ) ;
#21038 = DIRECTION ( 'NONE',  ( 0.000000000000000000, 0.000000000000000000, 1.000000000000000000 ) ) ;
#21039 = VERTEX_POINT ( 'NONE', #22461 ) ;
#21040 = VERTEX_POINT ( 'NONE', #30112 ) ;
#21041 = CARTESIAN_POINT ( 'NONE',  ( 0.1835381215211869255, 4.854340785353490340, -31.90397497931449067 ) ) ;
#21042 = DIRECTION ( 'NONE',  ( 0.000000000000000000, -0.000000000000000000, 1.000000000000000000 ) ) ;
#21043 = LINE ( 'NONE', #29413, #20991 ) ;
#21044 = DIRECTION ( 'NONE',  ( -0.9985334138511239299, -0.05413890858541756113, 0.000000000000000000 ) ) ;
#21045 = LINE ( 'NONE', #23883, #15428 ) ;
#21046 = ORIENTED_EDGE ( 'NONE', *, *, #28223, .T. ) ;
#21047 = DIRECTION ( 'NONE',  ( 1.000000000000000000, 0.000000000000000000, 0.000000000000000000 ) ) ;
#21048 = DIRECTION ( 'NONE',  ( 1.000000000000000000, 3.469446951953834515E-18, 0.000000000000000000 ) ) ;
#21049 = EDGE_CURVE ( 'NONE', #3348, #18796, #16786, .T. ) ;
#21050 = DIRECTION ( 'NONE',  ( -0.5611870653623822758, -0.8276889981568905652, 0.000000000000000000 ) ) ;
#21051 = DIRECTION ( 'NONE',  ( -0.000000000000000000, -0.000000000000000000, -1.000000000000000000 ) ) ;
#21052 = EDGE_CURVE ( 'NONE', #29922, #1478, #1592, .T. ) ;
#21053 = CIRCLE ( 'NONE', #25601, 1.154999999999999805 ) ;
#21054 = FACE_BOUND ( 'NONE', #31197, .T. ) ;
#21056 = DIRECTION ( 'NONE',  ( 0.000000000000000000, 1.000000000000000000, 5.145227585319922065E-49 ) ) ;
#21055 = LINE ( 'NONE', #4847, #2538 ) ;
#21057 = EDGE_CURVE ( 'NONE', #14037, #8068, #24289, .T. ) ;
#21058 = EDGE_CURVE ( 'NONE', #22052, #11199, #24935, .T. ) ;
#21059 = CARTESIAN_POINT ( 'NONE',  ( -37.55078559520313775, -4.831299144296465897, -15.81122994652406355 ) ) ;
#21060 = ORIENTED_EDGE ( 'NONE', *, *, #22945, .T. ) ;
#21061 = CARTESIAN_POINT ( 'NONE',  ( 109.9646280168875023, 2.883232572601705179, -12.16410353805738609 ) ) ;
#21062 = CARTESIAN_POINT ( 'NONE',  ( -8.176201638302029277E-14, 30.16006060148113832, 5.529416874852006281 ) ) ;
#21063 = ORIENTED_EDGE ( 'NONE', *, *, #417, .F. ) ;
#21064 = AXIS2_PLACEMENT_3D ( 'NONE', #14593, #22936, #8874 ) ;
#21065 = FACE_OUTER_BOUND ( 'NONE', #14166, .T. ) ;
#21066 = AXIS2_PLACEMENT_3D ( 'NONE', #33495, #28160, #14995 ) ;
#21067 = B_SPLINE_CURVE_WITH_KNOTS ( 'NONE', 3,
 ( #34353, #5140, #24010, #34892, #34530, #7280 ),
 .UNSPECIFIED., .F., .F.,
 ( 4, 2, 4 ),
 ( 4.404817061063498359E-07, 0.001874269649560073936, 0.003748098817414041457 ),
 .UNSPECIFIED. ) ;
#21068 = ORIENTED_EDGE ( 'NONE', *, *, #19004, .T. ) ;
#21069 = EDGE_CURVE ( 'NONE', #26408, #34260, #455, .T. ) ;
#21070 = ORIENTED_EDGE ( 'NONE', *, *, #8881, .F. ) ;
#21071 = DIRECTION ( 'NONE',  ( -0.000000000000000000, -0.000000000000000000, -1.000000000000000000 ) ) ;
#21072 = VERTEX_POINT ( 'NONE', #11424 ) ;
#21073 = EDGE_LOOP ( 'NONE', ( #1817, #2068, #3738, #21432 ) ) ;
#21074 = CIRCLE ( 'NONE', #33575, 4.000000000000003553 ) ;
#21075 = CARTESIAN_POINT ( 'NONE',  ( -442.0000000000000000, 109.0000000000000142, -175.0000000000000000 ) ) ;
#21076 = VECTOR ( 'NONE', #9364, 1000.000000000000114 ) ;
#21077 = ADVANCED_FACE ( 'NONE', ( #22111 ), #14284, .T. ) ;
#21079 = EDGE_CURVE ( 'NONE', #7819, #19171, #19277, .T. ) ;
#21078 = CARTESIAN_POINT ( 'NONE',  ( -34.66645501699844090, -15.21971901163155216, 68.31122994652405112 ) ) ;
#21080 = CARTESIAN_POINT ( 'NONE',  ( 2.789999999999999591, 4.060282914029383683, 30.39157201494050398 ) ) ;
#21081 = VERTEX_POINT ( 'NONE', #16609 ) ;
#21082 = ORIENTED_EDGE ( 'NONE', *, *, #26719, .F. ) ;
#21083 = FACE_OUTER_BOUND ( 'NONE', #23349, .T. ) ;
#21084 = DIRECTION ( 'NONE',  ( 0.000000000000000000, 0.000000000000000000, -1.000000000000000000 ) ) ;
#21085 = FACE_OUTER_BOUND ( 'NONE', #8171, .T. ) ;
#21086 = DIRECTION ( 'NONE',  ( -0.9075754196709575616, -0.4198891015602634891, -0.000000000000000000 ) ) ;
#21087 = CARTESIAN_POINT ( 'NONE',  ( 11.99999999999999645, 108.9999999999999858, -155.0000000000000000 ) ) ;
#21088 = ORIENTED_EDGE ( 'NONE', *, *, #8700, .F. ) ;
#21089 = CARTESIAN_POINT ( 'NONE',  ( -449.9999999999999432, -112.9999999999999858, 155.0000000000000000 ) ) ;
#21090 = CIRCLE ( 'NONE', #31302, 7.999999999999986677 ) ;
#21091 = CARTESIAN_POINT ( 'NONE',  ( -8.000000000000000000, 14.77499999999999858, 0.000000000000000000 ) ) ;
#21092 = ORIENTED_EDGE ( 'NONE', *, *, #24817, .F. ) ;
#21093 = CIRCLE ( 'NONE', #16005, 7.999999999999979572 ) ;
#21094 = CARTESIAN_POINT ( 'NONE',  ( -0.9727285265192152641, -1.747512292859696670, -0.7500000000000000000 ) ) ;
#21095 = DIRECTION ( 'NONE',  ( 1.000000000000000000, 0.000000000000000000, 0.000000000000000000 ) ) ;
#21096 = FACE_OUTER_BOUND ( 'NONE', #4250, .T. ) ;
#21097 = ORIENTED_EDGE ( 'NONE', *, *, #21902, .T. ) ;
#21098 = LINE ( 'NONE', #34455, #29148 ) ;
#21099 = ORIENTED_EDGE ( 'NONE', *, *, #25588, .T. ) ;
#21100 = EDGE_CURVE ( 'NONE', #2320, #30770, #24876, .T. ) ;
#21101 = EDGE_CURVE ( 'NONE', #17981, #8902, #3052, .T. ) ;
#21102 = DIRECTION ( 'NONE',  ( -0.000000000000000000, -5.053935297177146739E-49, -1.000000000000000000 ) ) ;
#21103 = EDGE_LOOP ( 'NONE', ( #29544, #17126, #13174, #26870 ) ) ;
#21104 = AXIS2_PLACEMENT_3D ( 'NONE', #23205, #12354, #18397 ) ;
#21106 = CARTESIAN_POINT ( 'NONE',  ( 2.789999999999999147, -13.59935610937951900, -26.37510281771846365 ) ) ;
#21105 = CARTESIAN_POINT ( 'NONE',  ( 1.749999999999999778, -24.90160365674851306, -23.75493189058367349 ) ) ;
#21107 = SURFACE_SIDE_STYLE ('',( #10613 ) ) ;
#21108 = EDGE_CURVE ( 'NONE', #14721, #5262, #3401, .T. ) ;
#21109 = ORIENTED_EDGE ( 'NONE', *, *, #6706, .T. ) ;
#21110 = CYLINDRICAL_SURFACE ( 'NONE', #8052, 7.999999999999986677 ) ;
#21111 = PLANE ( 'NONE',  #7459 ) ;
#21112 = ORIENTED_EDGE ( 'NONE', *, *, #11783, .F. ) ;
#21113 = CIRCLE ( 'NONE', #12590, 1.799999999999999600 ) ;
#21114 = DIRECTION ( 'NONE',  ( -7.893605728314051750E-14, 1.618803117314786530E-15, 1.000000000000000000 ) ) ;
#21115 = VECTOR ( 'NONE', #34107, 1000.000000000000000 ) ;
#21117 = ORIENTED_EDGE ( 'NONE', *, *, #2620, .F. ) ;
#21116 = CIRCLE ( 'NONE', #28517, 34.41491905851385269 ) ;
#21118 = CARTESIAN_POINT ( 'NONE',  ( 108.7903099957938480, -4.324196401257810685, 11.73154709691606001 ) ) ;
#21119 = ORIENTED_EDGE ( 'NONE', *, *, #16988, .T. ) ;
#21120 = CIRCLE ( 'NONE', #5752, 14.77499999999999858 ) ;
#21121 = DIRECTION ( 'NONE',  ( 0.000000000000000000, 0.000000000000000000, -1.000000000000000000 ) ) ;
#21122 = EDGE_CURVE ( 'NONE', #7363, #28204, #19801, .T. ) ;
#21123 = ADVANCED_FACE ( 'NONE', ( #13746 ), #217, .F. ) ;
#21124 = LINE ( 'NONE', #2775, #18733 ) ;
#21125 = EDGE_CURVE ( 'NONE', #12453, #19297, #21350, .T. ) ;
#21126 = LINE ( 'NONE', #23798, #27106 ) ;
#21127 = DIRECTION ( 'NONE',  ( -0.000000000000000000, 0.000000000000000000, -1.000000000000000000 ) ) ;
#21128 = ORIENTED_EDGE ( 'NONE', *, *, #553, .F. ) ;
#21129 = VERTEX_POINT ( 'NONE', #2643 ) ;
#21130 = ORIENTED_EDGE ( 'NONE', *, *, #8588, .T. ) ;
#21131 = LINE ( 'NONE', #10807, #15798 ) ;
#21132 = EDGE_CURVE ( 'NONE', #9350, #6574, #13510, .T. ) ;
#21133 = DIRECTION ( 'NONE',  ( -0.9985334138511239299, -0.05413890858541774848, 0.000000000000000000 ) ) ;
#21135 = EDGE_CURVE ( 'NONE', #18597, #11323, #5301, .T. ) ;
#21134 = CYLINDRICAL_SURFACE ( 'NONE', #5397, 4.000000000000003553 ) ;
#21136 = CARTESIAN_POINT ( 'NONE',  ( -355.0000000000000000, 130.9999999999999716, 126.0000000000000000 ) ) ;
#21137 = FACE_OUTER_BOUND ( 'NONE', #23483, .T. ) ;
#21138 = ORIENTED_EDGE ( 'NONE', *, *, #6962, .F. ) ;
#21139 = PRODUCT_DEFINITION_SHAPE ( 'NONE', 'NONE',  #35131 ) ;
#21140 = PLANE ( 'NONE',  #5449 ) ;
#21141 = CARTESIAN_POINT ( 'NONE',  ( -1.155000000000000027, 0.000000000000000000, 4.679999999999999716 ) ) ;
#21142 = VECTOR ( 'NONE', #9253, 1000.000000000000000 ) ;
#21143 = FACE_BOUND ( 'NONE', #12728, .T. ) ;
#21144 = ORIENTED_EDGE ( 'NONE', *, *, #719, .T. ) ;
#21145 = ADVANCED_FACE ( 'NONE', ( #2118 ), #24177, .T. ) ;
#21146 = VECTOR ( 'NONE', #6514, 1000.000000000000000 ) ;
#21147 = CIRCLE ( 'NONE', #6376, 7.999999999999979572 ) ;
#21148 = LINE ( 'NONE', #31992, #4706 ) ;
#21149 = ORIENTED_EDGE ( 'NONE', *, *, #4803, .F. ) ;
#21150 = AXIS2_PLACEMENT_3D ( 'NONE', #15301, #23301, #15651 ) ;
#21151 = CARTESIAN_POINT ( 'NONE',  ( -365.0000000000000000, -119.0000000000000000, 111.9999999999999858 ) ) ;
#21152 = PLANE ( 'NONE',  #3628 ) ;
#21153 = ORIENTED_EDGE ( 'NONE', *, *, #14813, .F. ) ;
#21154 = CARTESIAN_POINT ( 'NONE',  ( -5.866068224042683378E-16, 7.412728658108713731, 29.75205777216491398 ) ) ;
#21155 = CARTESIAN_POINT ( 'NONE',  ( -361.0000000000000000, 134.9999999999999716, 130.0000000000000000 ) ) ;
#21156 = LINE ( 'NONE', #29524, #14912 ) ;
#21157 = ORIENTED_EDGE ( 'NONE', *, *, #8191, .F. ) ;
#21158 = VERTEX_POINT ( 'NONE', #10491 ) ;
#21159 = DIRECTION ( 'NONE',  ( -3.363824698650303406E-14, 5.266234518492289948E-14, 0.9999999999999998890 ) ) ;
#21160 = ORIENTED_EDGE ( 'NONE', *, *, #34012, .F. ) ;
#21161 = LINE ( 'NONE', #34879, #2149 ) ;
#21162 = ADVANCED_FACE ( 'NONE', ( #24347 ), #5478, .T. ) ;
#21163 = AXIS2_PLACEMENT_3D ( 'NONE', #23901, #5033, #15932 ) ;
#21164 = DIRECTION ( 'NONE',  ( 0.000000000000000000, -0.000000000000000000, -1.000000000000000000 ) ) ;
#21165 = EDGE_CURVE ( 'NONE', #28091, #23681, #21161, .T. ) ;
#21166 = VECTOR ( 'NONE', #10416, 1000.000000000000000 ) ;
#21167 = CARTESIAN_POINT ( 'NONE',  ( -1.030735741678193262, 1.713938105891546382, 5.429999999999999716 ) ) ;
#21168 = CARTESIAN_POINT ( 'NONE',  ( 105.7855116681631245, -5.687452395779748038, 4.889156772952023999 ) ) ;
#21170 = VECTOR ( 'NONE', #26927, 1000.000000000000000 ) ;
#21169 = CONTEXT_DEPENDENT_SHAPE_REPRESENTATION ( #12612, #12662 ) ;
#21171 = VECTOR ( 'NONE', #460, 1000.000000000000000 ) ;
#21172 = EDGE_LOOP ( 'NONE', ( #11492, #15944, #24103, #23015 ) ) ;
#21173 = B_SPLINE_CURVE_WITH_KNOTS ( 'NONE', 3,
 ( #2843, #18550, #13709, #21188, #15879, #26703 ),
 .UNSPECIFIED., .F., .F.,
 ( 4, 2, 4 ),
 ( 4.404817019066348049E-07, 0.001874269618538362478, 0.003748098755374818306 ),
 .UNSPECIFIED. ) ;
#21174 = LINE ( 'NONE', #34522, #3242 ) ;
#21176 = DIRECTION ( 'NONE',  ( -8.433758354584418579E-81, 1.000000000000000000, 3.421138828918010427E-49 ) ) ;
#21175 = DIRECTION ( 'NONE',  ( 1.000000000000000000, 0.000000000000000000, 0.000000000000000000 ) ) ;
#21177 = ORIENTED_EDGE ( 'NONE', *, *, #29153, .F. ) ;
#21178 = VERTEX_POINT ( 'NONE', #21683 ) ;
#21179 = CARTESIAN_POINT ( 'NONE',  ( 2.606461875633085068, 21.48816195191898970, -24.07669289167323967 ) ) ;
#21180 = ORIENTED_EDGE ( 'NONE', *, *, #33674, .F. ) ;
#21181 = CARTESIAN_POINT ( 'NONE',  ( 37.55078559520313775, -4.831299144296470338, 68.31122994652405112 ) ) ;
#21182 = DIRECTION ( 'NONE',  ( 0.000000000000000000, 0.000000000000000000, 1.000000000000000000 ) ) ;
#21183 = ORIENTED_EDGE ( 'NONE', *, *, #28915, .T. ) ;
#21184 = DIRECTION ( 'NONE',  ( 1.000000000000000000, 0.000000000000000000, 0.000000000000000000 ) ) ;
#21185 = DIRECTION ( 'NONE',  ( 0.7621620551276372391, -0.6473862847818265820, -0.000000000000000000 ) ) ;
#21186 = EDGE_LOOP ( 'NONE', ( #25795, #29377, #31531, #24047 ) ) ;
#21187 = DIRECTION ( 'NONE',  ( 1.000000000000000000, 0.000000000000000000, -0.000000000000000000 ) ) ;
#21188 = CARTESIAN_POINT ( 'NONE',  ( 2.604019708608551031, -27.68787216339173085, 16.59794162419580132 ) ) ;
#21191 = LINE ( 'NONE', #10521, #21359 ) ;
#21190 = CARTESIAN_POINT ( 'NONE',  ( -418.0000000000000000, -125.0000000000000000, 187.0000000000000000 ) ) ;
#21189 = AXIS2_PLACEMENT_3D ( 'NONE', #17110, #27943, #3552 ) ;
#21192 = B_SPLINE_CURVE_WITH_KNOTS ( 'NONE', 3,
 ( #18435, #34263, #9879, #2217 ),
 .UNSPECIFIED., .F., .F.,
 ( 4, 4 ),
 ( 0.005298352430873783797, 0.005985221104152193584 ),
 .UNSPECIFIED. ) ;
#21193 = VECTOR ( 'NONE', #362, 1000.000000000000000 ) ;
#21194 = AXIS2_PLACEMENT_3D ( 'NONE', #14300, #14476, #6433 ) ;
#21195 = VECTOR ( 'NONE', #22905, 1000.000000000000000 ) ;
#21196 = DIRECTION ( 'NONE',  ( -0.9941379571543593752, -0.1081190184239432944, 0.000000000000000000 ) ) ;
#21197 = LINE ( 'NONE', #15884, #17894 ) ;
#21198 = DIRECTION ( 'NONE',  ( 0.000000000000000000, -1.000000000000000000, 0.000000000000000000 ) ) ;
#21199 = ORIENTED_EDGE ( 'NONE', *, *, #2870, .F. ) ;
#21200 = DIRECTION ( 'NONE',  ( 0.1063910735368947813, -0.9943243633099144718, -3.335902418024520312E-15 ) ) ;
#21201 = ORIENTED_EDGE ( 'NONE', *, *, #16898, .T. ) ;
#21202 = ORIENTED_EDGE ( 'NONE', *, *, #18176, .T. ) ;
#21203 = EDGE_CURVE ( 'NONE', #34376, #27996, #22046, .T. ) ;
#21204 = EDGE_CURVE ( 'NONE', #6833, #9096, #8156, .T. ) ;
#21205 = VECTOR ( 'NONE', #20713, 1000.000000000000000 ) ;
#21206 = DIRECTION ( 'NONE',  ( 0.000000000000000000, 0.000000000000000000, -1.000000000000000000 ) ) ;
#21207 = CARTESIAN_POINT ( 'NONE',  ( 819.7091759353768339, 1323.609930034304398, 1753.598338701304101 ) ) ;
#21208 = ORIENTED_EDGE ( 'NONE', *, *, #33742, .F. ) ;
#21209 = ORIENTED_EDGE ( 'NONE', *, *, #16051, .F. ) ;
#21210 = EDGE_CURVE ( 'NONE', #21769, #32541, #16016, .T. ) ;
#21211 = DIRECTION ( 'NONE',  ( 0.000000000000000000, 1.000000000000000000, 0.000000000000000000 ) ) ;
#21212 = DIRECTION ( 'NONE',  ( 0.000000000000000000, 0.000000000000000000, 1.000000000000000000 ) ) ;
#21214 = AXIS2_PLACEMENT_3D ( 'NONE', #23145, #7092, #28474 ) ;
#21213 = CONTEXT_DEPENDENT_SHAPE_REPRESENTATION ( #18338, #29200 ) ;
#21215 = CARTESIAN_POINT ( 'NONE',  ( 145.0000000000000568, -167.8552739801376390, -46.75049602362128809 ) ) ;
#21216 = VECTOR ( 'NONE', #18116, 1000.000000000000000 ) ;
#21217 = CARTESIAN_POINT ( 'NONE',  ( 2.604019748081172203, -28.85000931094332444, -14.48402167767649296 ) ) ;
#21218 = ORIENTED_EDGE ( 'NONE', *, *, #17226, .F. ) ;
#21219 = ORIENTED_EDGE ( 'NONE', *, *, #1546, .T. ) ;
#21220 = VECTOR ( 'NONE', #29950, 1000.000000000000000 ) ;
#21221 = DIRECTION ( 'NONE',  ( 0.000000000000000000, -1.310824597558155437E-49, -1.000000000000000000 ) ) ;
#21222 = CARTESIAN_POINT ( 'NONE',  ( -35.00000000000000000, -46.95407462254104303, 36.69637551990492597 ) ) ;
#21223 = DIRECTION ( 'NONE',  ( 0.000000000000000000, -1.000000000000000000, -1.131431318426415506E-52 ) ) ;
#21224 = DIRECTION ( 'NONE',  ( 0.000000000000000000, 1.836970198721029441E-16, -1.000000000000000000 ) ) ;
#21225 = DIRECTION ( 'NONE',  ( -0.8835120444460229372, -0.4684084406997900407, 0.000000000000000000 ) ) ;
#21226 = ORIENTED_EDGE ( 'NONE', *, *, #8466, .F. ) ;
#21227 = FACE_OUTER_BOUND ( 'NONE', #32895, .T. ) ;
#21228 = CARTESIAN_POINT ( 'NONE',  ( -28.00450684652666311, 16.58167570419054115, 68.31122994652405112 ) ) ;
#21229 = APPLICATION_CONTEXT ( 'automotive_design' ) ;
#21230 = LINE ( 'NONE', #10739, #17968 ) ;
#21231 = CYLINDRICAL_SURFACE ( 'NONE', #1328, 7.999999999999979572 ) ;
#21232 = CARTESIAN_POINT ( 'NONE',  ( 110.7380848894536740, 0.3953117532656757471, -7.500000000000019540 ) ) ;
#21234 = CARTESIAN_POINT ( 'NONE',  ( 20.00000000000001776, -145.0000000000000000, -162.9999999999999432 ) ) ;
#21233 = DIRECTION ( 'NONE',  ( -1.000000000000000000, 0.000000000000000000, 0.000000000000000000 ) ) ;
#21235 = AXIS2_PLACEMENT_3D ( 'NONE', #32888, #19381, #5821 ) ;
#21236 = DIRECTION ( 'NONE',  ( 0.000000000000000000, 0.000000000000000000, -1.000000000000000000 ) ) ;
#21237 = VERTEX_POINT ( 'NONE', #7975 ) ;
#21238 = DIRECTION ( 'NONE',  ( 0.000000000000000000, 0.000000000000000000, -1.000000000000000000 ) ) ;
#21240 = DIRECTION ( 'NONE',  ( 0.000000000000000000, -1.000000000000000000, -2.465190328815662439E-32 ) ) ;
#21239 = CARTESIAN_POINT ( 'NONE',  ( 0.000000000000000000, 0.000000000000000000, 20.00000000000000000 ) ) ;
#21241 = AXIS2_PLACEMENT_3D ( 'NONE', #30926, #17433, #20084 ) ;
#21243 = ORIENTED_EDGE ( 'NONE', *, *, #222, .F. ) ;
#21242 = AXIS2_PLACEMENT_3D ( 'NONE', #27309, #16133, #16843 ) ;
#21244 = CIRCLE ( 'NONE', #13283, 7.999999999999979572 ) ;
#21245 = PRODUCT_DEFINITION_SHAPE ( 'NONE', 'NONE',  #35235 ) ;
#21246 = B_SPLINE_CURVE_WITH_KNOTS ( 'NONE', 3,
 ( #18023, #26005, #23337, #10161 ),
 .UNSPECIFIED., .F., .F.,
 ( 4, 4 ),
 ( 0.005362286937562653344, 0.005985250355243621097 ),
 .UNSPECIFIED. ) ;
#21247 = ORIENTED_EDGE ( 'NONE', *, *, #7238, .T. ) ;
#21248 = ADVANCED_FACE ( 'NONE', ( #10303 ), #11255, .T. ) ;
#21249 = ORIENTED_EDGE ( 'NONE', *, *, #13495, .T. ) ;
#21250 = DIRECTION ( 'NONE',  ( -0.05413890858541543089, -0.9985334138511240409, -0.000000000000000000 ) ) ;
#21251 = VERTEX_POINT ( 'NONE', #26850 ) ;
#21252 = EDGE_LOOP ( 'NONE', ( #22324, #26243, #9894, #25661 ) ) ;
#21253 = EDGE_CURVE ( 'NONE', #18600, #14486, #16808, .T. ) ;
#21254 = CARTESIAN_POINT ( 'NONE',  ( 10.00000000000000000, 7.794228634059941818, 13.49999999999999645 ) ) ;
#21255 = EDGE_CURVE ( 'NONE', #27132, #26055, #15818, .T. ) ;
#21256 = AXIS2_PLACEMENT_3D ( 'NONE', #25182, #18089, #14885 ) ;
#21257 = CARTESIAN_POINT ( 'NONE',  ( 0.000000000000000000, 3.524919873834583163E-15, 68.31122994652405112 ) ) ;
#21258 = DIRECTION ( 'NONE',  ( 0.000000000000000000, 0.000000000000000000, -1.000000000000000000 ) ) ;
#21259 = EDGE_CURVE ( 'NONE', #3590, #15373, #33986, .T. ) ;
#21260 = ORIENTED_EDGE ( 'NONE', *, *, #23529, .T. ) ;
#21261 = EDGE_CURVE ( 'NONE', #18426, #7713, #7624, .T. ) ;
#21262 = ORIENTED_EDGE ( 'NONE', *, *, #5750, .T. ) ;
#21263 = CARTESIAN_POINT ( 'NONE',  ( 15.99999999999997868, -145.0000000000000000, 187.0000000000000000 ) ) ;
#21264 = CARTESIAN_POINT ( 'NONE',  ( 11.99999999999999645, -137.0000000000000000, 155.0000000000000000 ) ) ;
#21265 = CARTESIAN_POINT ( 'NONE',  ( -36.80830595996284416, 8.862931941313787476, -24.65111515542802323 ) ) ;
#21266 = EDGE_CURVE ( 'NONE', #15011, #2208, #15253, .T. ) ;
#21267 = CYLINDRICAL_SURFACE ( 'NONE', #16462, 4.000000000000003553 ) ;
#21268 = CARTESIAN_POINT ( 'NONE',  ( 5.021133111224162171, -23.57973016998034765, -67.50000000000000000 ) ) ;
#21269 = VERTEX_POINT ( 'NONE', #15846 ) ;
#21270 = CARTESIAN_POINT ( 'NONE',  ( 0.000000000000000000, -0.09145294252700143789, 30.47036804522410236 ) ) ;
#21271 = CARTESIAN_POINT ( 'NONE',  ( -445.9999999999999432, -105.0000000000000142, -101.9999999999999858 ) ) ;
#21272 = VECTOR ( 'NONE', #19813, 1000.000000000000000 ) ;
#21273 = CIRCLE ( 'NONE', #11606, 3.999999999999976019 ) ;
#21274 = DIRECTION ( 'NONE',  ( 0.000000000000000000, 2.309213040847544338E-50, 1.000000000000000000 ) ) ;
#21275 = ORIENTED_EDGE ( 'NONE', *, *, #6665, .F. ) ;
#21276 = AXIS2_PLACEMENT_3D ( 'NONE', #14488, #15317, #26147 ) ;
#21277 = CARTESIAN_POINT ( 'NONE',  ( -445.9999999999999432, 137.0000000000000000, 154.9999999999999716 ) ) ;
#21278 = CARTESIAN_POINT ( 'NONE',  ( -349.0000000000000000, 124.9999999999999432, 166.9999999999999716 ) ) ;
#21279 = FACE_OUTER_BOUND ( 'NONE', #21679, .T. ) ;
#21280 = ORIENTED_EDGE ( 'NONE', *, *, #28565, .T. ) ;
#21281 = CARTESIAN_POINT ( 'NONE',  ( 11.99999999999999645, -115.0000000000000000, 162.9999999999999716 ) ) ;
#21282 = VERTEX_POINT ( 'NONE', #26677 ) ;
#21283 =( REPRESENTATION_RELATIONSHIP ('NONE','NONE', #23037, #8672 ) REPRESENTATION_RELATIONSHIP_WITH_TRANSFORMATION ( #8206 )SHAPE_REPRESENTATION_RELATIONSHIP( ) );
#21284 = CARTESIAN_POINT ( 'NONE',  ( -418.0000000000000000, 137.0000000000000000, 154.9999999999999716 ) ) ;
#21285 = ORIENTED_EDGE ( 'NONE', *, *, #16162, .F. ) ;
#21287 = LINE ( 'NONE', #7214, #12297 ) ;
#21286 =( NAMED_UNIT ( * ) PLANE_ANGLE_UNIT ( ) SI_UNIT ( $, .RADIAN. ) );
#21288 = FACE_OUTER_BOUND ( 'NONE', #24927, .T. ) ;
#21289 = CIRCLE ( 'NONE', #4802, 7.999999999999979572 ) ;
#21290 = ORIENTED_EDGE ( 'NONE', *, *, #21135, .F. ) ;
#21291 = FILL_AREA_STYLE_COLOUR ( '', #2969 ) ;
#21292 = CARTESIAN_POINT ( 'NONE',  ( 10.00000000000000000, 2.296212748401288367E-15, 47.49999999999999289 ) ) ;
#21293 = VECTOR ( 'NONE', #20825, 1000.000000000000000 ) ;
#21294 = ORIENTED_EDGE ( 'NONE', *, *, #21699, .F. ) ;
#21295 = ADVANCED_FACE ( 'NONE', ( #21065 ), #18419, .T. ) ;
#21296 = CIRCLE ( 'NONE', #26983, 2.500000000000002220 ) ;
#21297 = CARTESIAN_POINT ( 'NONE',  ( 773.2897220451554858, 1184.641347914391645, 1753.598338701303419 ) ) ;
#21298 = CIRCLE ( 'NONE', #14483, 7.999999999999979572 ) ;
#21299 = VERTEX_POINT ( 'NONE', #8569 ) ;
#21300 = CARTESIAN_POINT ( 'NONE',  ( -99.88497961182919482, -2.585407550593147656E-15, 7.500000000000000000 ) ) ;
#21301 = EDGE_LOOP ( 'NONE', ( #28815, #32671, #11155, #6142 ) ) ;
#21302 = CARTESIAN_POINT ( 'NONE',  ( 2.765921099434983876, -15.32140196853734970, -27.05343472113007763 ) ) ;
#21303 = EDGE_CURVE ( 'NONE', #30541, #196, #21932, .T. ) ;
#21304 = LINE ( 'NONE', #15806, #533 ) ;
#21305 = LINE ( 'NONE', #29320, #3249 ) ;
#21306 = LINE ( 'NONE', #7763, #1168 ) ;
#21307 = EDGE_CURVE ( 'NONE', #29646, #20682, #8404, .T. ) ;
#21308 = ORIENTED_EDGE ( 'NONE', *, *, #23486, .F. ) ;
#21309 = EDGE_CURVE ( 'NONE', #28119, #30776, #18082, .T. ) ;
#21310 = EDGE_LOOP ( 'NONE', ( #33622, #17109, #6261, #2030 ) ) ;
#21311 = ORIENTED_EDGE ( 'NONE', *, *, #33182, .F. ) ;
#21312 = CARTESIAN_POINT ( 'NONE',  ( -499.9999999999999432, 112.9999999999999574, 162.9999999999999716 ) ) ;
#21313 = DIRECTION ( 'NONE',  ( -0.4198891015602651544, 0.9075754196709567845, 0.000000000000000000 ) ) ;
#21314 = PLANE ( 'NONE',  #25108 ) ;
#21315 = VECTOR ( 'NONE', #18738, 1000.000000000000000 ) ;
#21316 = CARTESIAN_POINT ( 'NONE',  ( -1.307386931792819285, 37.83772838912469894, 68.31122994652405112 ) ) ;
#21317 = DIRECTION ( 'NONE',  ( 0.000000000000000000, 0.000000000000000000, -1.000000000000000000 ) ) ;
#21318 = CARTESIAN_POINT ( 'NONE',  ( -347.0000000000000000, 134.9999999999999716, 125.9999999999999716 ) ) ;
#21319 = CARTESIAN_POINT ( 'NONE',  ( 0.000000000000000000, 3.524919873834583163E-15, 68.31122994652405112 ) ) ;
#21320 = ORIENTED_EDGE ( 'NONE', *, *, #10314, .T. ) ;
#21321 = AXIS2_PLACEMENT_3D ( 'NONE', #3526, #14415, #2997 ) ;
#21322 = DIRECTION ( 'NONE',  ( -1.000000000000000000, 0.000000000000000000, 0.000000000000000000 ) ) ;
#21323 = CARTESIAN_POINT ( 'NONE',  ( 0.000000000000000000, -29.91351748324107973, 5.799410679710550021 ) ) ;
#21324 = ADVANCED_FACE ( 'NONE', ( #29946 ), #7874, .T. ) ;
#21325 = CARTESIAN_POINT ( 'NONE',  ( -15.99999999999998579, 136.9999999999999716, -155.0000000000000000 ) ) ;
#21326 = ORIENTED_EDGE ( 'NONE', *, *, #12979, .F. ) ;
#21327 = B_SPLINE_CURVE_WITH_KNOTS ( 'NONE', 3,
 ( #2711, #18404, #29219, #7698, #29249, #12892 ),
 .UNSPECIFIED., .F., .F.,
 ( 4, 2, 4 ),
 ( 2.434544809778055946E-07, 0.001873441796234163017, 0.003746640137987347977 ),
 .UNSPECIFIED. ) ;
#21328 = AXIS2_PLACEMENT_3D ( 'NONE', #34906, #9984, #8497 ) ;
#21329 = VECTOR ( 'NONE', #29167, 1000.000000000000000 ) ;
#21330 = DIRECTION ( 'NONE',  ( 0.000000000000000000, 1.836970198721029688E-16, -1.000000000000000000 ) ) ;
#21331 = ORIENTED_EDGE ( 'NONE', *, *, #28209, .T. ) ;
#21333 = AXIS2_PLACEMENT_3D ( 'NONE', #31222, #22516, #6288 ) ;
#21332 = CARTESIAN_POINT ( 'NONE',  ( -108.3810596861186610, 3.852356953585670318, -11.89405885704114141 ) ) ;
#21334 = EDGE_CURVE ( 'NONE', #17164, #30600, #32948, .T. ) ;
#21335 = DIRECTION ( 'NONE',  ( 0.000000000000000000, 1.000000000000000000, 1.224646799147353207E-16 ) ) ;
#21336 = ADVANCED_FACE ( 'NONE', ( #18755 ), #3054, .F. ) ;
#21337 = EDGE_CURVE ( 'NONE', #22114, #19079, #9155, .T. ) ;
#21338 = EDGE_LOOP ( 'NONE', ( #2556, #1855, #19465, #35011 ) ) ;
#21339 = CARTESIAN_POINT ( 'NONE',  ( 32.30227131129396412, -3.970848902647437395, 68.31122994652405112 ) ) ;
#21340 = FACE_OUTER_BOUND ( 'NONE', #9883, .T. ) ;
#21341 = B_SPLINE_CURVE_WITH_KNOTS ( 'NONE', 3,
 ( #9593, #34312, #33970, #20791 ),
 .UNSPECIFIED., .F., .F.,
 ( 4, 4 ),
 ( 0.005298382169618340125, 0.005362286937562653344 ),
 .UNSPECIFIED. ) ;
#21342 = DIRECTION ( 'NONE',  ( -1.000000000000000000, 0.000000000000000000, 0.000000000000000000 ) ) ;
#21343 = ADVANCED_FACE ( 'NONE', ( #29421 ), #21584, .T. ) ;
#21344 = ORIENTED_EDGE ( 'NONE', *, *, #11001, .T. ) ;
#21345 = VECTOR ( 'NONE', #8478, 1000.000000000000000 ) ;
#21346 = ORIENTED_EDGE ( 'NONE', *, *, #20251, .T. ) ;
#21347 = DIRECTION ( 'NONE',  ( -7.893605728314050488E-14, 1.618803117314786135E-15, 0.9999999999999998890 ) ) ;
#21348 = CIRCLE ( 'NONE', #8839, 15.00000000000000000 ) ;
#21349 = ORIENTED_EDGE ( 'NONE', *, *, #626, .T. ) ;
#21350 = LINE ( 'NONE', #13163, #32830 ) ;
#21351 = DIRECTION ( 'NONE',  ( -0.000000000000000000, -0.000000000000000000, 1.000000000000000000 ) ) ;
#21352 = LINE ( 'NONE', #21167, #11634 ) ;
#21353 = CARTESIAN_POINT ( 'NONE',  ( 99.58179902723867372, -1.926730348087509981, 7.257477599627513598 ) ) ;
#21354 = CONTEXT_DEPENDENT_SHAPE_REPRESENTATION ( #22846, #7237 ) ;
#21355 = EDGE_CURVE ( 'NONE', #4287, #9216, #32777, .T. ) ;
#21356 = AXIS2_PLACEMENT_3D ( 'NONE', #328, #7615, #8146 ) ;
#21357 = ORIENTED_EDGE ( 'NONE', *, *, #11781, .F. ) ;
#21358 = DIRECTION ( 'NONE',  ( 0.000000000000000000, 0.000000000000000000, -1.000000000000000000 ) ) ;
#21359 = VECTOR ( 'NONE', #2672, 1000.000000000000227 ) ;
#21361 = DIRECTION ( 'NONE',  ( 0.000000000000000000, 0.000000000000000000, -1.000000000000000000 ) ) ;
#21360 = CARTESIAN_POINT ( 'NONE',  ( 22.10765473302597073, -12.47301499840864025, -77.50000000000000000 ) ) ;
#21362 = ORIENTED_EDGE ( 'NONE', *, *, #5624, .T. ) ;
#21363 = ORIENTED_EDGE ( 'NONE', *, *, #3107, .F. ) ;
#21364 = CARTESIAN_POINT ( 'NONE',  ( 37.09133285470120711, -7.633836879289874311, 68.31122994652405112 ) ) ;
#21365 = ORIENTED_EDGE ( 'NONE', *, *, #19305, .F. ) ;
#21366 = CARTESIAN_POINT ( 'NONE',  ( -35.00000000000000000, 42.49491490430484220, 36.69637551990492597 ) ) ;
#21367 = CARTESIAN_POINT ( 'NONE',  ( -1.649999999999999911, 0.000000000000000000, 3.180000000000000160 ) ) ;
#21368 = ORIENTED_EDGE ( 'NONE', *, *, #30326, .F. ) ;
#21369 = AXIS2_PLACEMENT_3D ( 'NONE', #15367, #17354, #3789 ) ;
#21370 = DIRECTION ( 'NONE',  ( 0.000000000000000000, 0.000000000000000000, -1.000000000000000000 ) ) ;
#21371 = DIRECTION ( 'NONE',  ( 0.000000000000000000, 1.836970198721029688E-16, -1.000000000000000000 ) ) ;
#21372 = EDGE_LOOP ( 'NONE', ( #22123, #25472, #12046, #20754 ) ) ;
#21373 = VECTOR ( 'NONE', #10369, 1000.000000000000000 ) ;
#21374 = CARTESIAN_POINT ( 'NONE',  ( -449.9999999999999432, -105.0000000000000142, 187.0000000000000000 ) ) ;
#21375 = CARTESIAN_POINT ( 'NONE',  ( -10.84269519964070305, -36.27449394610876965, -36.68877005347593467 ) ) ;
#21376 = CARTESIAN_POINT ( 'NONE',  ( 15.99999999999997868, 144.9999999999999716, -186.9999999999999716 ) ) ;
#21377 = ADVANCED_FACE ( 'NONE', ( #13578 ), #11259, .F. ) ;
#21379 = CARTESIAN_POINT ( 'NONE',  ( -19.99999999999998934, 144.9999999999999716, -186.9999999999999716 ) ) ;
#21378 = DIRECTION ( 'NONE',  ( 1.000000000000000000, 0.000000000000000000, 0.000000000000000000 ) ) ;
#21380 = EDGE_CURVE ( 'NONE', #28865, #30842, #5017, .T. ) ;
#21381 = CARTESIAN_POINT ( 'NONE',  ( -365.0000000000000000, -135.0000000000000000, 126.0000000000000000 ) ) ;
#21382 = LINE ( 'NONE', #27236, #12251 ) ;
#21383 = CARTESIAN_POINT ( 'NONE',  ( 2.606461878478813166, 4.854340785353028487, 31.90397497931456883 ) ) ;
#21384 = ORIENTED_EDGE ( 'NONE', *, *, #15762, .F. ) ;
#21385 = DIRECTION ( 'NONE',  ( 0.000000000000000000, 0.000000000000000000, 1.000000000000000000 ) ) ;
#21386 = DIRECTION ( 'NONE',  ( 0.1063910735368947813, -0.9943243633099144718, -3.335902418024520312E-15 ) ) ;
#21387 = PRODUCT_DEFINITION_CONTEXT ( 'detailed design', #4841, 'design' ) ;
#21388 = ORIENTED_EDGE ( 'NONE', *, *, #26542, .T. ) ;
#21389 = VERTEX_POINT ( 'NONE', #2350 ) ;
#21390 = VECTOR ( 'NONE', #20483, 1000.000000000000000 ) ;
#21391 = CARTESIAN_POINT ( 'NONE',  ( 108.4949890547536455, 4.564908081027950537, 5.956352141036524550 ) ) ;
#21392 = ORIENTED_EDGE ( 'NONE', *, *, #16096, .T. ) ;
#21393 = CARTESIAN_POINT ( 'NONE',  ( -20.00000000000004619, -134.9999999999999716, -186.9999999999999716 ) ) ;
#21394 = AXIS2_PLACEMENT_3D ( 'NONE', #14285, #22810, #3757 ) ;
#21395 = CONTEXT_DEPENDENT_SHAPE_REPRESENTATION ( #11044, #29499 ) ;
#21396 = DIRECTION ( 'NONE',  ( -1.000000000000000000, -0.000000000000000000, 0.000000000000000000 ) ) ;
#21397 = EDGE_LOOP ( 'NONE', ( #4714, #24406, #26374, #29962 ) ) ;
#21398 = EDGE_LOOP ( 'NONE', ( #13697, #33656, #26846, #32380 ) ) ;
#21399 = CARTESIAN_POINT ( 'NONE',  ( -32.54223829851970606, 0.4550817492056113966, 68.31122994652405112 ) ) ;
#21401 = EDGE_CURVE ( 'NONE', #33010, #1712, #2874, .T. ) ;
#21400 = LINE ( 'NONE', #30107, #31722 ) ;
#21402 = COLOUR_RGB ( '',0.7921568627450980005, 0.8196078431372548767, 0.9333333333333333481 ) ;
#21403 = CARTESIAN_POINT ( 'NONE',  ( -414.0000000000000568, 113.0000000000000000, -155.0000000000000000 ) ) ;
#21404 = CARTESIAN_POINT ( 'NONE',  ( -36.80830595996284416, 8.862931941313773265, 68.31122994652405112 ) ) ;
#21405 = PLANE ( 'NONE',  #14876 ) ;
#21406 = ORIENTED_EDGE ( 'NONE', *, *, #2039, .F. ) ;
#21407 = DIRECTION ( 'NONE',  ( 1.000000000000000000, -0.000000000000000000, -0.000000000000000000 ) ) ;
#21408 = FACE_OUTER_BOUND ( 'NONE', #3798, .T. ) ;
#21409 = CARTESIAN_POINT ( 'NONE',  ( -442.0000000000000000, 113.0000000000000000, 154.9999999999999716 ) ) ;
#21410 = DIRECTION ( 'NONE',  ( -1.000000000000000000, -0.000000000000000000, -0.000000000000000000 ) ) ;
#21411 = AXIS2_PLACEMENT_3D ( 'NONE', #2837, #21184, #16219 ) ;
#21412 = EDGE_CURVE ( 'NONE', #19565, #27398, #10738, .T. ) ;
#21413 = DIRECTION ( 'NONE',  ( 0.000000000000000000, 0.000000000000000000, 1.000000000000000000 ) ) ;
#21414 = FACE_OUTER_BOUND ( 'NONE', #27104, .T. ) ;
#21415 = EDGE_CURVE ( 'NONE', #22892, #21604, #27091, .T. ) ;
#21417 = LINE ( 'NONE', #8411, #20793 ) ;
#21416 = DIRECTION ( 'NONE',  ( -1.000000000000000000, 0.000000000000000000, 0.000000000000000000 ) ) ;
#21418 = AXIS2_PLACEMENT_3D ( 'NONE', #25956, #28625, #25773 ) ;
#21419 = ADVANCED_FACE ( 'NONE', ( #29764, #24411 ), #38, .T. ) ;
#21420 = DIRECTION ( 'NONE',  ( -0.000000000000000000, 1.000000000000000000, -0.000000000000000000 ) ) ;
#21421 = ORIENTED_EDGE ( 'NONE', *, *, #10566, .T. ) ;
#21422 = PRODUCT_DEFINITION ( 'UNKNOWN', '', #19554, #21387 ) ;
#21423 = CARTESIAN_POINT ( 'NONE',  ( 104.2390490158698526, 5.700015625666662089, -11.12505441474362478 ) ) ;
#21425 = PLANE ( 'NONE',  #15162 ) ;
#21424 = FACE_OUTER_BOUND ( 'NONE', #4367, .T. ) ;
#21426 = VERTEX_POINT ( 'NONE', #19105 ) ;
#21427 = DIRECTION ( 'NONE',  ( -0.000000000000000000, -0.000000000000000000, 1.000000000000000000 ) ) ;
#21428 = ORIENTED_EDGE ( 'NONE', *, *, #21846, .F. ) ;
#21429 = VERTEX_POINT ( 'NONE', #5708 ) ;
#21430 = DIRECTION ( 'NONE',  ( 0.000000000000000000, -2.309213040847544338E-50, -1.000000000000000000 ) ) ;
#21431 = VERTEX_POINT ( 'NONE', #16612 ) ;
#21432 = ORIENTED_EDGE ( 'NONE', *, *, #27234, .F. ) ;
#21433 = CARTESIAN_POINT ( 'NONE',  ( -355.0000000000000000, -114.9999999999999858, 113.9999999999999858 ) ) ;
#21434 = CIRCLE ( 'NONE', #9499, 13.49999999999999822 ) ;
#21435 = VECTOR ( 'NONE', #24355, 999.9999999999998863 ) ;
#21436 = DIRECTION ( 'NONE',  ( 0.000000000000000000, 0.000000000000000000, 1.000000000000000000 ) ) ;
#21437 = FACE_OUTER_BOUND ( 'NONE', #23311, .T. ) ;
#21438 = EDGE_LOOP ( 'NONE', ( #15604, #14243, #7638, #21183, #1230, #2477, #19994, #32962 ) ) ;
#21439 = ORIENTED_EDGE ( 'NONE', *, *, #8407, .F. ) ;
#21440 = CARTESIAN_POINT ( 'NONE',  ( 5.021133111224162171, -25.61315202898006049, -67.50000000000000000 ) ) ;
#21441 = CYLINDRICAL_SURFACE ( 'NONE', #24295, 2.033421858999711507 ) ;
#21442 = CARTESIAN_POINT ( 'NONE',  ( 0.006892390059616927689, 11.66157578832105557, -28.58237449055226165 ) ) ;
#21443 = CARTESIAN_POINT ( 'NONE',  ( 2.790000000000081304, 7.412271713510841131, 29.75335163721786103 ) ) ;
#21444 = ORIENTED_EDGE ( 'NONE', *, *, #27637, .F. ) ;
#21445 = PRESENTATION_LAYER_ASSIGNMENT (  '', '', ( #27759 ) ) ;
#21446 = DIRECTION ( 'NONE',  ( 0.000000000000000000, 0.000000000000000000, -1.000000000000000000 ) ) ;
#21447 = DIRECTION ( 'NONE',  ( 0.000000000000000000, 1.836970198721029441E-16, -1.000000000000000000 ) ) ;
#21448 = VERTEX_POINT ( 'NONE', #6237 ) ;
#21449 = EDGE_CURVE ( 'NONE', #6749, #8018, #18030, .T. ) ;
#21450 = CARTESIAN_POINT ( 'NONE',  ( -449.9999999999999432, -105.0000000000000142, 131.9999999999999716 ) ) ;
#21451 = FACE_OUTER_BOUND ( 'NONE', #20599, .T. ) ;
#21452 = ADVANCED_FACE ( 'NONE', ( #17319 ), #25111, .F. ) ;
#21453 = CARTESIAN_POINT ( 'NONE',  ( -8.149999999999998579, 2.020667218593133001E-16, 0.000000000000000000 ) ) ;
#21454 = EDGE_LOOP ( 'NONE', ( #17910, #11056, #23189, #19658 ) ) ;
#21455 = CYLINDRICAL_SURFACE ( 'NONE', #27448, 2.524999999999999467 ) ;
#21456 = VERTEX_POINT ( 'NONE', #22285 ) ;
#21457 = VECTOR ( 'NONE', #14241, 1000.000000000000000 ) ;
#21458 = DIRECTION ( 'NONE',  ( 0.000000000000000000, 1.000000000000000000, -3.374343856708137958E-53 ) ) ;
#21459 = VECTOR ( 'NONE', #15763, 1000.000000000000000 ) ;
#21460 = ORIENTED_EDGE ( 'NONE', *, *, #25872, .F. ) ;
#21461 = ADVANCED_FACE ( 'NONE', ( #14286 ), #11426, .F. ) ;
#21463 = LINE ( 'NONE', #7389, #19131 ) ;
#21462 = CARTESIAN_POINT ( 'NONE',  ( 0.3923936511923831194, 30.27116788629744804, 13.00174666746672969 ) ) ;
#21464 = SURFACE_STYLE_USAGE ( .BOTH. , #21107 ) ;
#21465 = VECTOR ( 'NONE', #12708, 1000.000000000000000 ) ;
#21466 = CIRCLE ( 'NONE', #34517, 1.999999999999999556 ) ;
#21467 = ORIENTED_EDGE ( 'NONE', *, *, #9330, .T. ) ;
#21468 =( LENGTH_UNIT ( ) NAMED_UNIT ( * ) SI_UNIT ( .MILLI., .METRE. ) );
#21469 = PLANE ( 'NONE',  #10322 ) ;
#21470 = ADVANCED_FACE ( 'NONE', ( #17137 ), #33316, .T. ) ;
#21471 = VERTEX_POINT ( 'NONE', #24937 ) ;
#21472 = EDGE_CURVE ( 'NONE', #30456, #17724, #22811, .T. ) ;
#21473 = MECHANICAL_DESIGN_GEOMETRIC_PRESENTATION_REPRESENTATION (  '', ( #27759 ), #9536 ) ;
#21474 = DIRECTION ( 'NONE',  ( -0.1063910735369225230, 0.9943243633099118073, -1.000770725407345128E-14 ) ) ;
#21475 = VERTEX_POINT ( 'NONE', #33658 ) ;
#21476 = CARTESIAN_POINT ( 'NONE',  ( -105.6885685459855893, 5.080227507390848274, 5.518150456212836730 ) ) ;
#21477 = ORIENTED_EDGE ( 'NONE', *, *, #6848, .F. ) ;
#21478 = DIRECTION ( 'NONE',  ( 1.000000000000000000, 3.040835319149746528E-31, 1.232595164407830946E-32 ) ) ;
#21479 = CARTESIAN_POINT ( 'NONE',  ( -20.00000000000007461, 140.9999999999999716, 187.0000000000000000 ) ) ;
#21480 = AXIS2_PLACEMENT_3D ( 'NONE', #956, #28533, #25501 ) ;
#21481 = CARTESIAN_POINT ( 'NONE',  ( -109.7700750224988582, -1.854090048725078432, -7.268955362025010025 ) ) ;
#21482 = PLANE ( 'NONE',  #608 ) ;
#21483 = ORIENTED_EDGE ( 'NONE', *, *, #4722, .F. ) ;
#21484 = ORIENTED_EDGE ( 'NONE', *, *, #29737, .F. ) ;
#21485 = EDGE_LOOP ( 'NONE', ( #5887, #12363, #19445, #7353, #27921, #18744 ) ) ;
#21486 = CARTESIAN_POINT ( 'NONE',  ( -10.00000000000000000, 0.000000000000000000, 0.000000000000000000 ) ) ;
#21487 = B_SPLINE_CURVE_WITH_KNOTS ( 'NONE', 3,
 ( #30346, #17031, #5948, #33544 ),
 .UNSPECIFIED., .F., .F.,
 ( 4, 4 ),
 ( 0.005298558704933876984, 0.005985424570307887326 ),
 .UNSPECIFIED. ) ;
#21488 = DIRECTION ( 'NONE',  ( -0.9766205557100864354, 0.2149704402110247659, -0.000000000000000000 ) ) ;
#21489 = CARTESIAN_POINT ( 'NONE',  ( -430.0000000000000000, -117.0000000000000000, 113.9999999999999858 ) ) ;
#21490 = VECTOR ( 'NONE', #27263, 1000.000000000000000 ) ;
#21491 = VECTOR ( 'NONE', #31680, 1000.000000000000000 ) ;
#21492 = LINE ( 'NONE', #2093, #8247 ) ;
#21493 = CARTESIAN_POINT ( 'NONE',  ( -418.0000000000000000, 104.9999999999999858, -187.0000000000000000 ) ) ;
#21495 = PLANE ( 'NONE',  #990 ) ;
#21494 =( REPRESENTATION_RELATIONSHIP ('NONE','NONE', #23037, #15767 ) REPRESENTATION_RELATIONSHIP_WITH_TRANSFORMATION ( #1902 )SHAPE_REPRESENTATION_RELATIONSHIP( ) );
#21496 = CARTESIAN_POINT ( 'NONE',  ( -1.625000000000000000, 2.702098422956710877, 3.930000000000000160 ) ) ;
#21497 = ORIENTED_EDGE ( 'NONE', *, *, #2377, .T. ) ;
#21498 = LINE ( 'NONE', #5458, #3193 ) ;
#21499 = CARTESIAN_POINT ( 'NONE',  ( 22.89764159710615132, -1.579009122040562207, -77.50000000000000000 ) ) ;
#21500 = VECTOR ( 'NONE', #434, 1000.000000000000000 ) ;
#21501 = CARTESIAN_POINT ( 'NONE',  ( -418.0000000000000000, -105.0000000000000142, 139.9999999999999716 ) ) ;
#21502 = VERTEX_POINT ( 'NONE', #11615 ) ;
#21503 = DIRECTION ( 'NONE',  ( -3.469446951953832974E-18, -1.000000000000000000, -7.888609052210116302E-31 ) ) ;
#21504 = ORIENTED_EDGE ( 'NONE', *, *, #24634, .T. ) ;
#21505 = CARTESIAN_POINT ( 'NONE',  ( -100.6601417511032395, 2.712336548677835246, -12.20300697856195882 ) ) ;
#21506 = ADVANCED_FACE ( 'NONE', ( #33129 ), #572, .T. ) ;
#21507 = FACE_BOUND ( 'NONE', #25855, .T. ) ;
#21508 = VECTOR ( 'NONE', #6764, 1000.000000000000000 ) ;
#21509 = EDGE_LOOP ( 'NONE', ( #34616, #28966, #12254, #29796 ) ) ;
#21510 = EDGE_CURVE ( 'NONE', #16280, #33055, #4416, .T. ) ;
#21511 = EDGE_CURVE ( 'NONE', #14283, #32317, #21811, .T. ) ;
#21512 = DIRECTION ( 'NONE',  ( -1.000000000000000000, -0.000000000000000000, -0.000000000000000000 ) ) ;
#21513 = PLANE ( 'NONE',  #878 ) ;
#21514 = LINE ( 'NONE', #16008, #7478 ) ;
#21515 = ORIENTED_EDGE ( 'NONE', *, *, #19216, .T. ) ;
#21516 = AXIS2_PLACEMENT_3D ( 'NONE', #30020, #11693, #477 ) ;
#21517 = ORIENTED_EDGE ( 'NONE', *, *, #23900, .F. ) ;
#21518 = CARTESIAN_POINT ( 'NONE',  ( 806.5733988790774447, 1365.751034482728755, 1753.598338701303646 ) ) ;
#21519 = AXIS2_PLACEMENT_3D ( 'NONE', #2291, #34886, #21358 ) ;
#21520 = CARTESIAN_POINT ( 'NONE',  ( -12.00000000000001066, -124.9999999999999432, -158.9999999999999716 ) ) ;
#21521 = ORIENTED_EDGE ( 'NONE', *, *, #30700, .T. ) ;
#21522 = CARTESIAN_POINT ( 'NONE',  ( 0.1835381473997496904, 25.37843598539303258, -19.93397194544865769 ) ) ;
#21523 = EDGE_CURVE ( 'NONE', #4201, #19566, #25294, .T. ) ;
#21524 = VECTOR ( 'NONE', #29757, 1000.000000000000000 ) ;
#21525 = DIRECTION ( 'NONE',  ( 1.000000000000000000, 3.040835319149746090E-31, 1.232595164407830946E-32 ) ) ;
#21526 = CARTESIAN_POINT ( 'NONE',  ( -20.00000000000007461, 112.9999999999999574, -162.9999999999999716 ) ) ;
#21527 = CARTESIAN_POINT ( 'NONE',  ( -41.91891556802573859, 16.36473396058513785, -36.68877005347594178 ) ) ;
#21528 = ORIENTED_EDGE ( 'NONE', *, *, #19369, .T. ) ;
#21529 = CARTESIAN_POINT ( 'NONE',  ( -418.0000000000000000, 124.9999999999999432, -159.0000000000000000 ) ) ;
#21530 = EDGE_CURVE ( 'NONE', #18207, #16944, #26393, .T. ) ;
#21531 = ADVANCED_FACE ( 'NONE', ( #14645 ), #3230, .T. ) ;
#21533 = CARTESIAN_POINT ( 'NONE',  ( 5.021133111224162171, -23.57973016998034765, -87.50000000000000000 ) ) ;
#21532 = LINE ( 'NONE', #18868, #19577 ) ;
#21534 = VECTOR ( 'NONE', #19708, 1000.000000000000000 ) ;
#21535 = EDGE_CURVE ( 'NONE', #24033, #33864, #19629, .T. ) ;
#21536 = EDGE_LOOP ( 'NONE', ( #21477, #18715, #9169, #12185 ) ) ;
#21537 = VERTEX_POINT ( 'NONE', #30288 ) ;
#21538 = LINE ( 'NONE', #31840, #15761 ) ;
#21539 = ORIENTED_EDGE ( 'NONE', *, *, #24859, .T. ) ;
#21540 = DIRECTION ( 'NONE',  ( -0.000000000000000000, 0.5288966977476834419, -0.8486862100397269959 ) ) ;
#21541 = DIRECTION ( 'NONE',  ( -0.000000000000000000, 1.000000000000000000, -0.000000000000000000 ) ) ;
#21542 = ORIENTED_EDGE ( 'NONE', *, *, #25634, .F. ) ;
#21543=STYLED_ITEM('',(#35254),#10344);
#21544 = ORIENTED_EDGE ( 'NONE', *, *, #5813, .F. ) ;
#21545 = CARTESIAN_POINT ( 'NONE',  ( 0.000000000000000000, 3.524919873834583163E-15, 68.31122994652405112 ) ) ;
#21546 = CARTESIAN_POINT ( 'NONE',  ( -25.63124651156763179, 20.05601094782695526, -36.68877005347593467 ) ) ;
#21547 = ORIENTED_EDGE ( 'NONE', *, *, #16264, .F. ) ;
#21548 = LINE ( 'NONE', #8006, #2705 ) ;
#21549 = LINE ( 'NONE', #19410, #34203 ) ;
#21550 = LINE ( 'NONE', #7832, #28058 ) ;
#21551 = DIRECTION ( 'NONE',  ( 2.891205793294675861E-16, 0.000000000000000000, -1.000000000000000000 ) ) ;
#21552 = EDGE_CURVE ( 'NONE', #6402, #5434, #5890, .T. ) ;
#21553 = EDGE_CURVE ( 'NONE', #9444, #7282, #6598, .T. ) ;
#21554 = FACE_OUTER_BOUND ( 'NONE', #1676, .T. ) ;
#21555 = DIRECTION ( 'NONE',  ( 1.000000000000000000, 0.000000000000000000, -0.000000000000000000 ) ) ;
#21556 = FACE_OUTER_BOUND ( 'NONE', #34076, .T. ) ;
#21557 = EDGE_CURVE ( 'NONE', #19179, #10465, #19163, .T. ) ;
#21558 = AXIS2_PLACEMENT_3D ( 'NONE', #18914, #32591, #19099 ) ;
#21559 = EDGE_LOOP ( 'NONE', ( #26323, #4406, #34357, #15450, #14803, #22783, #32378, #11818 ) ) ;
#21560 = DIRECTION ( 'NONE',  ( 0.000000000000000000, 1.000000000000000000, 0.000000000000000000 ) ) ;
#21561 = VERTEX_POINT ( 'NONE', #20320 ) ;
#21562 = EDGE_LOOP ( 'NONE', ( #18451, #24895, #21368, #19738 ) ) ;
#21563 = TOROIDAL_SURFACE ( 'NONE', #26105, 30.47050528711511674, 8.000000000000000000 ) ;
#21564 = ADVANCED_BREP_SHAPE_REPRESENTATION ( '', ( #827, #28566 ), #6416 ) ;
#21565 = DIRECTION ( 'NONE',  ( 0.000000000000000000, 0.000000000000000000, -1.000000000000000000 ) ) ;
#21566 = CARTESIAN_POINT ( 'NONE',  ( 816.6957136404158746, 1349.431083307295694, 1753.598338701303646 ) ) ;
#21567 = ORIENTED_EDGE ( 'NONE', *, *, #11927, .T. ) ;
#21568 = CYLINDRICAL_SURFACE ( 'NONE', #31538, 16.19999999999999218 ) ;
#21569 = CARTESIAN_POINT ( 'NONE',  ( -145.0000000000000568, -78.33668825982579165, -65.00000000000000000 ) ) ;
#21570 = EDGE_CURVE ( 'NONE', #8463, #26131, #15157, .T. ) ;
#21571 = EDGE_CURVE ( 'NONE', #28489, #4850, #7288, .T. ) ;
#21572 = DIRECTION ( 'NONE',  ( 0.000000000000000000, 1.836970198721029688E-16, -1.000000000000000000 ) ) ;
#21573 = ORIENTED_EDGE ( 'NONE', *, *, #4623, .T. ) ;
#21574 = ORIENTED_EDGE ( 'NONE', *, *, #22390, .F. ) ;
#21575 = CARTESIAN_POINT ( 'NONE',  ( -19.99999999999998934, -56.99999999999996447, 155.0000000000000000 ) ) ;
#21576 = FACE_OUTER_BOUND ( 'NONE', #10138, .T. ) ;
#21577 = EDGE_CURVE ( 'NONE', #2206, #31947, #15692, .T. ) ;
#21578 = DIRECTION ( 'NONE',  ( 0.000000000000000000, 0.000000000000000000, 1.000000000000000000 ) ) ;
#21579 = CARTESIAN_POINT ( 'NONE',  ( -19.99999999999998934, 75.55999999999990280, 168.2400000000000091 ) ) ;
#21580 = CYLINDRICAL_SURFACE ( 'NONE', #64, 34.41491905851385269 ) ;
#21581 = ORIENTED_EDGE ( 'NONE', *, *, #13680, .F. ) ;
#21582 = FACE_OUTER_BOUND ( 'NONE', #5610, .T. ) ;
#21583 = PLANE ( 'NONE',  #3752 ) ;
#21584 = CYLINDRICAL_SURFACE ( 'NONE', #25442, 34.41491905851385269 ) ;
#21585 = EDGE_CURVE ( 'NONE', #5794, #5593, #12487, .T. ) ;
#21586 = ADVANCED_FACE ( 'NONE', ( #4091 ), #28672, .T. ) ;
#21587 = LINE ( 'NONE', #23728, #23174 ) ;
#21588 = CARTESIAN_POINT ( 'NONE',  ( 2.789999999999999147, -27.96208973699912548, 13.59246946040177129 ) ) ;
#21589 = CYLINDRICAL_SURFACE ( 'NONE', #34855, 3.999999999999976019 ) ;
#21591 = CARTESIAN_POINT ( 'NONE',  ( -99.88497961182919482, 6.264093345946821604E-16, 60.00000000000000000 ) ) ;
#21590 = CARTESIAN_POINT ( 'NONE',  ( 0.000000000000000000, 17.11426446101199161, 26.96776559937732642 ) ) ;
#21592 = CARTESIAN_POINT ( 'NONE',  ( 2.790000000000000480, 25.77033216996941078, -16.61395588374042376 ) ) ;
#21593 = ORIENTED_EDGE ( 'NONE', *, *, #23673, .F. ) ;
#21594 = PLANE ( 'NONE',  #9367 ) ;
#21596 = CARTESIAN_POINT ( 'NONE',  ( 110.7380848894537166, -0.1972643383979439669, -7.500000000000013323 ) ) ;
#21595 = DIRECTION ( 'NONE',  ( 0.000000000000000000, -1.000000000000000000, -1.224646799147353207E-16 ) ) ;
#21597 = AXIS2_PLACEMENT_3D ( 'NONE', #20344, #15006, #6620 ) ;
#21598 = EDGE_LOOP ( 'NONE', ( #31022, #516, #24284, #29189 ) ) ;
#21599 = CYLINDRICAL_SURFACE ( 'NONE', #30257, 15.00000000000000000 ) ;
#21600 = EDGE_CURVE ( 'NONE', #11445, #763, #17664, .T. ) ;
#21601 = ORIENTED_EDGE ( 'NONE', *, *, #6539, .T. ) ;
#21602 = ORIENTED_EDGE ( 'NONE', *, *, #27957, .T. ) ;
#21603 = CARTESIAN_POINT ( 'NONE',  ( 1.749999999999999778, -25.27164158951585549, 23.36088151536907631 ) ) ;
#21604 = VERTEX_POINT ( 'NONE', #23849 ) ;
#21605 = VERTEX_POINT ( 'NONE', #12318 ) ;
#21606 = DIRECTION ( 'NONE',  ( 3.697785493223492838E-32, 1.934419779023891545E-16, -1.000000000000000000 ) ) ;
#21607 = ADVANCED_FACE ( 'NONE', ( #26344 ), #29196, .T. ) ;
#21608 = EDGE_CURVE ( 'NONE', #3207, #8431, #22565, .T. ) ;
#21609 = ADVANCED_FACE ( 'NONE', ( #2140 ), #4272, .F. ) ;
#21610 = FACE_OUTER_BOUND ( 'NONE', #30433, .T. ) ;
#21611 = CARTESIAN_POINT ( 'NONE',  ( 2.765921099433440222, -27.96208973699893008, -13.59246946040217630 ) ) ;
#21612 = EDGE_LOOP ( 'NONE', ( #7343, #28315, #7649, #2596 ) ) ;
#21613 = VERTEX_POINT ( 'NONE', #20663 ) ;
#21614 = DIRECTION ( 'NONE',  ( 0.4198891015602645438, -0.9075754196709570065, -0.000000000000000000 ) ) ;
#21615 = DIRECTION ( 'NONE',  ( 0.000000000000000000, -0.9510565162951545304, 0.3090169943749441206 ) ) ;
#21616 = CARTESIAN_POINT ( 'NONE',  ( 107.5565492092080859, -5.150622582557323526, -11.39062369188951251 ) ) ;
#21617 = CARTESIAN_POINT ( 'NONE',  ( -445.9999999999999432, -112.9999999999999858, 155.0000000000000000 ) ) ;
#21618 = ORIENTED_EDGE ( 'NONE', *, *, #21961, .F. ) ;
#21619 = LINE ( 'NONE', #18788, #7711 ) ;
#21620 = DIRECTION ( 'NONE',  ( -1.000000000000000000, 0.000000000000000000, 0.000000000000000000 ) ) ;
#21621 = ORIENTED_EDGE ( 'NONE', *, *, #7351, .F. ) ;
#21622 = CARTESIAN_POINT ( 'NONE',  ( -414.0000000000000568, 105.0000000000000142, -101.9999999999999858 ) ) ;
#21623 = DIRECTION ( 'NONE',  ( 0.000000000000000000, 0.000000000000000000, -1.000000000000000000 ) ) ;
#21624 = DIRECTION ( 'NONE',  ( -1.000000000000000000, -0.000000000000000000, -0.000000000000000000 ) ) ;
#21625 = CARTESIAN_POINT ( 'NONE',  ( -11.99999999999998224, -134.9999999999999716, 155.0000000000000000 ) ) ;
#21626 = ORIENTED_EDGE ( 'NONE', *, *, #32576, .T. ) ;
#21627 = CIRCLE ( 'NONE', #18876, 10.00000000000000000 ) ;
#21628 = FACE_OUTER_BOUND ( 'NONE', #2893, .T. ) ;
#21629 = EDGE_LOOP ( 'NONE', ( #30897, #24322, #14121, #9885 ) ) ;
#21631 = DIRECTION ( 'NONE',  ( 0.000000000000000000, 0.000000000000000000, -1.000000000000000000 ) ) ;
#21630 = FILL_AREA_STYLE_COLOUR ( '', #26187 ) ;
#21632 = CARTESIAN_POINT ( 'NONE',  ( 2.789999999999999147, 5.092684668492991840, -30.01061466292821933 ) ) ;
#21633 = VERTEX_POINT ( 'NONE', #18357 ) ;
#21634 = CARTESIAN_POINT ( 'NONE',  ( -449.9999999999999432, 105.0000000000000142, 162.9999999999999716 ) ) ;
#21635 = CIRCLE ( 'NONE', #6272, 14.19999999999999929 ) ;
#21636 = ORIENTED_EDGE ( 'NONE', *, *, #1524, .T. ) ;
#21637 = AXIS2_PLACEMENT_3D ( 'NONE', #4387, #12601, #31455 ) ;
#21638 = ORIENTED_EDGE ( 'NONE', *, *, #7088, .F. ) ;
#21639 = CARTESIAN_POINT ( 'NONE',  ( 22.89764159710615132, -5.651112684911597128, -77.50000000000000000 ) ) ;
#21640 = CARTESIAN_POINT ( 'NONE',  ( 1.991296462759138297, -32.48444414290483451, 49.43553178847298568 ) ) ;
#21641 = VERTEX_POINT ( 'NONE', #4444 ) ;
#21642 = EDGE_LOOP ( 'NONE', ( #16630, #31910, #29685, #28349 ) ) ;
#21643 = DIRECTION ( 'NONE',  ( 0.000000000000000000, 1.000000000000000000, 0.000000000000000000 ) ) ;
#21644 = ADVANCED_FACE ( 'NONE', ( #34008 ), #31173, .T. ) ;
#21645 = EDGE_CURVE ( 'NONE', #32274, #18981, #7366, .T. ) ;
#21646 = DIRECTION ( 'NONE',  ( 0.000000000000000000, 0.000000000000000000, 1.000000000000000000 ) ) ;
#21647 = AXIS2_PLACEMENT_3D ( 'NONE', #2700, #4833, #7867 ) ;
#21648 = DIRECTION ( 'NONE',  ( 0.000000000000000000, 0.000000000000000000, 1.000000000000000000 ) ) ;
#21649 = ORIENTED_EDGE ( 'NONE', *, *, #2532, .F. ) ;
#21650 = VERTEX_POINT ( 'NONE', #34358 ) ;
#21651 = AXIS2_PLACEMENT_3D ( 'NONE', #29642, #5240, #26974 ) ;
#21652 = DIRECTION ( 'NONE',  ( -0.000000000000000000, 1.836970198721029934E-16, -1.000000000000000000 ) ) ;
#21653 = EDGE_CURVE ( 'NONE', #29676, #7312, #11204, .T. ) ;
#21654 = CARTESIAN_POINT ( 'NONE',  ( -499.9999999999999432, 144.9999999999999716, 162.9999999999999716 ) ) ;
#21655 = CARTESIAN_POINT ( 'NONE',  ( 2.033589655516955474, 6.875279775961012696, 33.21136585175272415 ) ) ;
#21656 = CARTESIAN_POINT ( 'NONE',  ( -500.0000000000000000, -137.0000000000000000, 159.0000000000000000 ) ) ;
#21657 = CARTESIAN_POINT ( 'NONE',  ( -355.0000000000000000, 116.9999999999999716, 113.9999999999999858 ) ) ;
#21658 = CARTESIAN_POINT ( 'NONE',  ( 11.99999999999999645, 134.9999999999998863, 194.9999999999999716 ) ) ;
#21659 = DIRECTION ( 'NONE',  ( 0.000000000000000000, 1.836970198721029441E-16, -1.000000000000000000 ) ) ;
#21660 = ORIENTED_EDGE ( 'NONE', *, *, #24854, .F. ) ;
#21661 = CIRCLE ( 'NONE', #20551, 2.000000000000001776 ) ;
#21662 = CARTESIAN_POINT ( 'NONE',  ( -32.17792593279633451, -19.96555837188923022, 68.31122994652405112 ) ) ;
#21663 = EDGE_CURVE ( 'NONE', #12696, #17092, #15503, .T. ) ;
#21664 = DIRECTION ( 'NONE',  ( -0.000000000000000000, 1.000000000000000000, -0.000000000000000000 ) ) ;
#21665 = CARTESIAN_POINT ( 'NONE',  ( 0.2222207399973191444, 3.306033584726114860, -13.49999999999999645 ) ) ;
#21666 = ORIENTED_EDGE ( 'NONE', *, *, #14817, .F. ) ;
#21667 = CYLINDRICAL_SURFACE ( 'NONE', #18941, 7.999999999999952038 ) ;
#21668 = ORIENTED_EDGE ( 'NONE', *, *, #31613, .F. ) ;
#21669 = CARTESIAN_POINT ( 'NONE',  ( -106.3376375495021335, 4.939893293632461990, -11.48260997023825958 ) ) ;
#21670 = CARTESIAN_POINT ( 'NONE',  ( -19.99999999999998934, 134.9999999999999432, -162.9999999999999432 ) ) ;
#21672 = ORIENTED_EDGE ( 'NONE', *, *, #11503, .F. ) ;
#21671 = CIRCLE ( 'NONE', #24500, 34.41491905851385269 ) ;
#21673 = AXIS2_PLACEMENT_3D ( 'NONE', #7260, #31998, #1929 ) ;
#21674 = LINE ( 'NONE', #16531, #2358 ) ;
#21675 = CIRCLE ( 'NONE', #26219, 3.999999999999976019 ) ;
#21676 = CARTESIAN_POINT ( 'NONE',  ( -418.0000000000000000, -125.0000000000000000, 155.0000000000000000 ) ) ;
#21677 = CARTESIAN_POINT ( 'NONE',  ( -19.99999999999996092, -137.0000000000000284, 194.9999999999999716 ) ) ;
#21678 = ORIENTED_EDGE ( 'NONE', *, *, #21530, .T. ) ;
#21679 = EDGE_LOOP ( 'NONE', ( #21346, #31714, #25147, #82 ) ) ;
#21680 = DIRECTION ( 'NONE',  ( 0.9871130995123816865, -0.1600241505869001157, 1.938748308457283288E-14 ) ) ;
#21681 = LINE ( 'NONE', #7799, #32018 ) ;
#21682 = ORIENTED_EDGE ( 'NONE', *, *, #21334, .T. ) ;
#21683 = CARTESIAN_POINT ( 'NONE',  ( 22.10765473302597073, -12.47301499840864025, -77.50000000000000000 ) ) ;
#21684 = EDGE_CURVE ( 'NONE', #1771, #18581, #7464, .T. ) ;
#21685 = VECTOR ( 'NONE', #6890, 1000.000000000000000 ) ;
#21686 = CARTESIAN_POINT ( 'NONE',  ( 32.05156013847311414, -20.15193397489275640, 49.43553178847298568 ) ) ;
#21687 = CARTESIAN_POINT ( 'NONE',  ( -109.3194926363487269, -2.744499711777497186, 6.981349484866706590 ) ) ;
#21688 = ORIENTED_EDGE ( 'NONE', *, *, #21449, .T. ) ;
#21689 = VERTEX_POINT ( 'NONE', #4794 ) ;
#21690 = EDGE_CURVE ( 'NONE', #8215, #18536, #28497, .T. ) ;
#21691 = FACE_OUTER_BOUND ( 'NONE', #22020, .T. ) ;
#21692 = ADVANCED_FACE ( 'NONE', ( #31337 ), #17835, .F. ) ;
#21693 = AXIS2_PLACEMENT_3D ( 'NONE', #4244, #10660, #23827 ) ;
#21695 = CARTESIAN_POINT ( 'NONE',  ( 1.749999999999999778, -10.89151784028311809, 32.64600270996213283 ) ) ;
#21694 = DIRECTION ( 'NONE',  ( 0.000000000000000000, 1.000000000000000000, 0.000000000000000000 ) ) ;
#21697 = ORIENTED_EDGE ( 'NONE', *, *, #31471, .T. ) ;
#21696 = VECTOR ( 'NONE', #9554, 1000.000000000000114 ) ;
#21698 = ORIENTED_EDGE ( 'NONE', *, *, #18967, .T. ) ;
#21699 = EDGE_CURVE ( 'NONE', #32511, #9264, #29378, .T. ) ;
#21700 = EDGE_CURVE ( 'NONE', #1226, #26104, #11772, .T. ) ;
#21701 = CARTESIAN_POINT ( 'NONE',  ( 2.765921099433441110, -27.96208973699912548, 13.59246946040177129 ) ) ;
#21702 = VECTOR ( 'NONE', #19371, 1000.000000000000000 ) ;
#21703 = ORIENTED_EDGE ( 'NONE', *, *, #27209, .F. ) ;
#21704 = AXIS2_PLACEMENT_3D ( 'NONE', #11390, #9767, #12809 ) ;
#21705 = DIRECTION ( 'NONE',  ( -0.000000000000000000, -0.000000000000000000, -1.000000000000000000 ) ) ;
#21706 = ADVANCED_FACE ( 'NONE', ( #32738 ), #8174, .F. ) ;
#21707 = CARTESIAN_POINT ( 'NONE',  ( 10.96230482721425403, -12.47301499840864025, -77.50000000000000000 ) ) ;
#21708 = ORIENTED_EDGE ( 'NONE', *, *, #10878, .T. ) ;
#21709 = VERTEX_POINT ( 'NONE', #13702 ) ;
#21710 = FACE_OUTER_BOUND ( 'NONE', #7392, .T. ) ;
#21711 = CYLINDRICAL_SURFACE ( 'NONE', #13203, 9.999999999999994671 ) ;
#21712 = ORIENTED_EDGE ( 'NONE', *, *, #33703, .F. ) ;
#21713 = LINE ( 'NONE', #24901, #18659 ) ;
#21714 = CARTESIAN_POINT ( 'NONE',  ( -35.00000000000000000, -7.062798427011562019, 68.31122994652405112 ) ) ;
#21715 = ADVANCED_FACE ( 'NONE', ( #21710 ), #10694, .T. ) ;
#21716 = CARTESIAN_POINT ( 'NONE',  ( -500.0000000000000000, 104.9999999999999858, -155.0000000000000000 ) ) ;
#21717 = DIRECTION ( 'NONE',  ( -0.000000000000000000, 1.836970198721029688E-16, -1.000000000000000000 ) ) ;
#21718 = CARTESIAN_POINT ( 'NONE',  ( 9.199999999999999289, 13.50000000000000178, 0.000000000000000000 ) ) ;
#21719 = CARTESIAN_POINT ( 'NONE',  ( -442.0000000000000000, -105.0000000000000142, -105.9999999999999574 ) ) ;
#21720 = DIRECTION ( 'NONE',  ( -0.000000000000000000, -0.000000000000000000, 1.000000000000000000 ) ) ;
#21721 = VECTOR ( 'NONE', #30790, 1000.000000000000000 ) ;
#21722 = ORIENTED_EDGE ( 'NONE', *, *, #23305, .T. ) ;
#21723 = AXIS2_PLACEMENT_3D ( 'NONE', #31429, #29289, #4886 ) ;
#21724 = CARTESIAN_POINT ( 'NONE',  ( -365.0000000000000000, -125.0000000000000284, 126.0000000000000000 ) ) ;
#21725 = DIRECTION ( 'NONE',  ( 1.000000000000000000, 0.000000000000000000, 0.000000000000000000 ) ) ;
#21726 = CIRCLE ( 'NONE', #20594, 34.41491905851385269 ) ;
#21727 = EDGE_LOOP ( 'NONE', ( #5497, #17778, #8736, #31572 ) ) ;
#21728 = ORIENTED_EDGE ( 'NONE', *, *, #8064, .F. ) ;
#21729 = CARTESIAN_POINT ( 'NONE',  ( -6.500000000000000000, 0.000000000000000000, -0.7500000000000000000 ) ) ;
#21730 = SHAPE_DEFINITION_REPRESENTATION ( #14933, #15767 ) ;
#21731 = ORIENTED_EDGE ( 'NONE', *, *, #27033, .F. ) ;
#21732 = DIRECTION ( 'NONE',  ( 0.000000000000000000, 0.000000000000000000, -1.000000000000000000 ) ) ;
#21733 = CARTESIAN_POINT ( 'NONE',  ( 143.0000000000000568, -45.49999999999999289, 63.00000000000000000 ) ) ;
#21734 = CONTEXT_DEPENDENT_SHAPE_REPRESENTATION ( #19467, #11951 ) ;
#21735 = PLANE ( 'NONE',  #33447 ) ;
#21736 = ORIENTED_EDGE ( 'NONE', *, *, #22751, .T. ) ;
#21737 = ORIENTED_EDGE ( 'NONE', *, *, #6022, .T. ) ;
#21738 = ADVANCED_FACE ( 'NONE', ( #5669 ), #10857, .T. ) ;
#21739 = EDGE_CURVE ( 'NONE', #13146, #22962, #33421, .T. ) ;
#21740 = DIRECTION ( 'NONE',  ( 0.000000000000000000, 0.000000000000000000, 1.000000000000000000 ) ) ;
#21741 = DIRECTION ( 'NONE',  ( -0.000000000000000000, -0.000000000000000000, -1.000000000000000000 ) ) ;
#21742 = LINE ( 'NONE', #11420, #7903 ) ;
#21743 = DIRECTION ( 'NONE',  ( -1.000000000000000000, 0.000000000000000000, 0.000000000000000000 ) ) ;
#21744 = DIRECTION ( 'NONE',  ( 0.000000000000000000, 0.000000000000000000, 1.000000000000000000 ) ) ;
#21745 = ORIENTED_EDGE ( 'NONE', *, *, #9423, .T. ) ;
#21746 = DIRECTION ( 'NONE',  ( 0.000000000000000000, 0.000000000000000000, -1.000000000000000000 ) ) ;
#21747 = LINE ( 'NONE', #27791, #6030 ) ;
#21748 = DIRECTION ( 'NONE',  ( -1.000000000000000000, -0.000000000000000000, -0.000000000000000000 ) ) ;
#21749 = AXIS2_PLACEMENT_3D ( 'NONE', #15123, #25605, #7080 ) ;
#21750 = AXIS2_PLACEMENT_3D ( 'NONE', #19892, #3669, #28063 ) ;
#21751 = CARTESIAN_POINT ( 'NONE',  ( -130.6469666100234406, -6.000000000000000000, 62.49999999999999289 ) ) ;
#21752 = LINE ( 'NONE', #32951, #10995 ) ;
#21753 = EDGE_CURVE ( 'NONE', #16412, #6833, #16319, .T. ) ;
#21754 = DIRECTION ( 'NONE',  ( -1.000000000000000000, 0.000000000000000000, -0.000000000000000000 ) ) ;
#21756 = CARTESIAN_POINT ( 'NONE',  ( -19.99999999999998934, -113.0000000000000142, 155.0000000000000000 ) ) ;
#21755 = CARTESIAN_POINT ( 'NONE',  ( 0.000000000000000000, 0.000000000000000000, -0.7500000000000000000 ) ) ;
#21757 = B_SPLINE_CURVE_WITH_KNOTS ( 'NONE', 3,
 ( #31184, #19640, #17149, #3585 ),
 .UNSPECIFIED., .F., .F.,
 ( 4, 4 ),
 ( 0.005298419352602270690, 0.005985287046740435900 ),
 .UNSPECIFIED. ) ;
#21758 = ORIENTED_EDGE ( 'NONE', *, *, #1292, .F. ) ;
#21759 = FACE_OUTER_BOUND ( 'NONE', #10537, .T. ) ;
#21761 = DIRECTION ( 'NONE',  ( -1.000000000000000000, 0.000000000000000000, 0.000000000000000000 ) ) ;
#21760 = DIRECTION ( 'NONE',  ( -1.000000000000000000, 0.000000000000000000, 0.000000000000000000 ) ) ;
#21762 = ADVANCED_FACE ( 'NONE', ( #29906 ), #16037, .T. ) ;
#21763 = EDGE_CURVE ( 'NONE', #15781, #11675, #29553, .T. ) ;
#21764 = EDGE_CURVE ( 'NONE', #27865, #30543, #34493, .T. ) ;
#21765 = EDGE_LOOP ( 'NONE', ( #11997, #28920, #8636, #26119 ) ) ;
#21766 = CARTESIAN_POINT ( 'NONE',  ( 12.00000000000001066, -32.99999999999997158, -175.0000000000000000 ) ) ;
#21767 = B_SPLINE_CURVE_WITH_KNOTS ( 'NONE', 3,
 ( #4353, #9881, #20573, #14728 ),
 .UNSPECIFIED., .F., .F.,
 ( 4, 4 ),
 ( 2.042209043309361781E-07, 0.0006879399691689030505 ),
 .UNSPECIFIED. ) ;
#21768 = ADVANCED_FACE ( 'NONE', ( #3007 ), #5145, .F. ) ;
#21769 = VERTEX_POINT ( 'NONE', #16396 ) ;
#21770 = AXIS2_PLACEMENT_3D ( 'NONE', #29866, #21838, #16355 ) ;
#21771 = AXIS2_PLACEMENT_3D ( 'NONE', #5337, #15519, #34911 ) ;
#21772 = VECTOR ( 'NONE', #18233, 1000.000000000000000 ) ;
#21773 = ORIENTED_EDGE ( 'NONE', *, *, #20769, .F. ) ;
#21774 = LINE ( 'NONE', #21956, #19033 ) ;
#21775 = EDGE_LOOP ( 'NONE', ( #28899, #18833, #4904, #1629, #2142, #22387 ) ) ;
#21776 = EDGE_LOOP ( 'NONE', ( #15666, #30811, #33973, #3898, #27926, #34002 ) ) ;
#21777 = PLANE ( 'NONE',  #30384 ) ;
#21778 = DIRECTION ( 'NONE',  ( 0.000000000000000000, 1.000000000000000000, 0.000000000000000000 ) ) ;
#21779 = CARTESIAN_POINT ( 'NONE',  ( -5.021133111225196011, -25.61315202898005694, -87.50000000000000000 ) ) ;
#21780 = VERTEX_POINT ( 'NONE', #18881 ) ;
#21781 = VERTEX_POINT ( 'NONE', #29722 ) ;
#21782 = EDGE_CURVE ( 'NONE', #2476, #26364, #23695, .T. ) ;
#21783 = CARTESIAN_POINT ( 'NONE',  ( 0.07098925407227295314, -28.42160548755711247, -14.02701190433918121 ) ) ;
#21784 = DIRECTION ( 'NONE',  ( 0.000000000000000000, 1.000000000000000000, 0.000000000000000000 ) ) ;
#21785 = CARTESIAN_POINT ( 'NONE',  ( 110.2200992156835042, -2.389942209051219457, -12.27067588826158939 ) ) ;
#21786 = DIRECTION ( 'NONE',  ( -1.000000000000000000, -0.000000000000000000, -0.000000000000000000 ) ) ;
#21787 = EDGE_LOOP ( 'NONE', ( #14382, #21119, #2949, #14749 ) ) ;
#21788 = LINE ( 'NONE', #11298, #3731 ) ;
#21789 = VECTOR ( 'NONE', #30864, 1000.000000000000114 ) ;
#21790 = FACE_OUTER_BOUND ( 'NONE', #5314, .T. ) ;
#21791 = EDGE_LOOP ( 'NONE', ( #23127, #1762, #23558, #31120 ) ) ;
#21792 = CARTESIAN_POINT ( 'NONE',  ( 0.000000000000000000, -13.59935610937951900, -26.37510281771846365 ) ) ;
#21793 = CARTESIAN_POINT ( 'NONE',  ( 2.783107593501489951, -30.26126365281908548, 6.099214421699650224 ) ) ;
#21794 = CARTESIAN_POINT ( 'NONE',  ( 1.749999999999999778, 0.000000000000000000, 0.000000000000000000 ) ) ;
#21795 = AXIS2_PLACEMENT_3D ( 'NONE', #12987, #2283, #5121 ) ;
#21796 = DIRECTION ( 'NONE',  ( -3.040835319149746090E-31, -1.000000000000000000, 0.000000000000000000 ) ) ;
#21797 = ORIENTED_EDGE ( 'NONE', *, *, #13987, .F. ) ;
#21798 = CONICAL_SURFACE ( 'NONE', #5296, 13.50000000000000000, 1.047197551196600296 ) ;
#21799 = AXIS2_PLACEMENT_3D ( 'NONE', #25075, #9072, #6033 ) ;
#21800 = ORIENTED_EDGE ( 'NONE', *, *, #15235, .T. ) ;
#21802 = DIRECTION ( 'NONE',  ( 0.000000000000000000, -0.4817536741017159341, 0.8763066800438632509 ) ) ;
#21801 = CARTESIAN_POINT ( 'NONE',  ( -130.6469666100234406, -6.000000000000000000, -57.49999999999999289 ) ) ;
#21803 = ADVANCED_FACE ( 'NONE', ( #2665 ), #35094, .F. ) ;
#21804 = EDGE_CURVE ( 'NONE', #34687, #25412, #30079, .T. ) ;
#21805 = VERTEX_POINT ( 'NONE', #13885 ) ;
#21806 = CARTESIAN_POINT ( 'NONE',  ( 2.790000000000080860, -21.14989222980560513, 22.20103112977897197 ) ) ;
#21807 = CARTESIAN_POINT ( 'NONE',  ( 2.261199750249991869, -32.52406052302377049, -7.554116419246889258 ) ) ;
#21808 = ORIENTED_EDGE ( 'NONE', *, *, #27470, .T. ) ;
#21809 = VERTEX_POINT ( 'NONE', #26698 ) ;
#21810 = AXIS2_PLACEMENT_3D ( 'NONE', #13859, #24698, #30220 ) ;
#21811 = B_SPLINE_CURVE_WITH_KNOTS ( 'NONE', 3,
 ( #30651, #27616, #19970, #33840, #6065, #3924 ),
 .UNSPECIFIED., .F., .F.,
 ( 4, 2, 4 ),
 ( 2.380729204614569766E-07, 0.003943479449179625521, 0.007886720825438786608 ),
 .UNSPECIFIED. ) ;
#21812 = ORIENTED_EDGE ( 'NONE', *, *, #23181, .F. ) ;
#21813 = DIRECTION ( 'NONE',  ( 1.000000000000000000, 0.000000000000000000, 5.546364386991661285E-52 ) ) ;
#21814 = CARTESIAN_POINT ( 'NONE',  ( -101.6241379746951452, 3.856339488913145264, 6.437882550241559976 ) ) ;
#21815 = ORIENTED_EDGE ( 'NONE', *, *, #31611, .F. ) ;
#21816 = ORIENTED_EDGE ( 'NONE', *, *, #4331, .T. ) ;
#21817 = LINE ( 'NONE', #32673, #2496 ) ;
#21818 = AXIS2_PLACEMENT_3D ( 'NONE', #18292, #18642, #32147 ) ;
#21819 = CARTESIAN_POINT ( 'NONE',  ( 2.789999999999999147, 30.40449935640660684, -2.004522720844263084 ) ) ;
#21820 = LINE ( 'NONE', #22358, #25991 ) ;
#21821 = DIRECTION ( 'NONE',  ( 0.000000000000000000, -0.8486862100397269959, 0.5288966977476833309 ) ) ;
#21822 = ORIENTED_EDGE ( 'NONE', *, *, #4668, .F. ) ;
#21823 = ORIENTED_EDGE ( 'NONE', *, *, #23283, .F. ) ;
#21824 = CARTESIAN_POINT ( 'NONE',  ( -499.9999999999999432, 104.9999999999999858, 162.9999999999999716 ) ) ;
#21825 = CARTESIAN_POINT ( 'NONE',  ( -35.00000000000000000, -46.95407462254104303, -36.69637551990492597 ) ) ;
#21826 = CARTESIAN_POINT ( 'NONE',  ( -12.25939112814508825, 30.14816249862102637, 68.31122994652405112 ) ) ;
#21827 = VECTOR ( 'NONE', #28174, 1000.000000000000000 ) ;
#21828 = CARTESIAN_POINT ( 'NONE',  ( 2.719051659407074606, 7.308651292219749074, 30.83982692225031386 ) ) ;
#21829 = CARTESIAN_POINT ( 'NONE',  ( 31.83311414508813897, -6.771795677801495827, 68.31122994652405112 ) ) ;
#21830 = DIRECTION ( 'NONE',  ( 0.000000000000000000, 2.309213040847544338E-50, 1.000000000000000000 ) ) ;
#21831 = DIRECTION ( 'NONE',  ( 1.000000000000000000, 0.000000000000000000, 0.000000000000000000 ) ) ;
#21832 = ORIENTED_EDGE ( 'NONE', *, *, #10737, .F. ) ;
#21833 = DIRECTION ( 'NONE',  ( 0.000000000000000000, 0.000000000000000000, 1.000000000000000000 ) ) ;
#21834 = LINE ( 'NONE', #2791, #13173 ) ;
#21835 = DIRECTION ( 'NONE',  ( 0.000000000000000000, 0.000000000000000000, -1.000000000000000000 ) ) ;
#21836 = VERTEX_POINT ( 'NONE', #2302 ) ;
#21837 = VECTOR ( 'NONE', #6137, 1000.000000000000000 ) ;
#21838 = DIRECTION ( 'NONE',  ( 1.000000000000000000, 0.000000000000000000, -1.232595164407831220E-32 ) ) ;
#21839 = EDGE_LOOP ( 'NONE', ( #24171, #12758, #14387, #23352 ) ) ;
#21840 = AXIS2_PLACEMENT_3D ( 'NONE', #1433, #20312, #28318 ) ;
#21841 = CARTESIAN_POINT ( 'NONE',  ( -101.6156648126628568, 3.849558703864950804, -11.89498339909459723 ) ) ;
#21842 = ADVANCED_FACE ( 'NONE', ( #888 ), #22241, .T. ) ;
#21843 = CARTESIAN_POINT ( 'NONE',  ( 55.00000000000000711, 8.448225943918016683E-16, -6.898500000000000298 ) ) ;
#21844 = PRODUCT_DEFINITION_FORMATION_WITH_SPECIFIED_SOURCE ( 'ANY', '', #2933, .NOT_KNOWN. ) ;
#21845 = EDGE_CURVE ( 'NONE', #32964, #17480, #21434, .T. ) ;
#21846 = EDGE_CURVE ( 'NONE', #10753, #5416, #14606, .T. ) ;
#21847 = AXIS2_PLACEMENT_3D ( 'NONE', #32783, #19636, #22654 ) ;
#21848 = ORIENTED_EDGE ( 'NONE', *, *, #15400, .F. ) ;
#21849 = VECTOR ( 'NONE', #3415, 1000.000000000000000 ) ;
#21850 = LINE ( 'NONE', #10657, #6905 ) ;
#21851 = PLANE ( 'NONE',  #8254 ) ;
#21853 = EDGE_CURVE ( 'NONE', #24787, #1716, #30534, .T. ) ;
#21852 = LINE ( 'NONE', #19373, #26832 ) ;
#21854 = CIRCLE ( 'NONE', #12206, 44.99999999999998579 ) ;
#21855 = VERTEX_POINT ( 'NONE', #24896 ) ;
#21856 = ORIENTED_EDGE ( 'NONE', *, *, #18407, .T. ) ;
#21857 = DIRECTION ( 'NONE',  ( 2.631201909438060269E-14, -5.396010391056495992E-16, 0.9999999999999998890 ) ) ;
#21858 = DIRECTION ( 'NONE',  ( 0.000000000000000000, -0.8486862100397269959, -0.5288966977476834419 ) ) ;
#21859 = ORIENTED_EDGE ( 'NONE', *, *, #809, .F. ) ;
#21860 = CARTESIAN_POINT ( 'NONE',  ( -9.978866888775632660, -5.758675521474015291, -67.50000000000000000 ) ) ;
#21861 = FACE_OUTER_BOUND ( 'NONE', #22738, .T. ) ;
#21862 = CIRCLE ( 'NONE', #5366, 4.000000000000003553 ) ;
#21863 = CARTESIAN_POINT ( 'NONE',  ( -499.9999999999999432, 108.9999999999999858, -162.9999999999999716 ) ) ;
#21864 = CARTESIAN_POINT ( 'NONE',  ( -110.1062952961228376, -0.3451077285824886154, 7.494041212912380345 ) ) ;
#21865 = CONTEXT_DEPENDENT_SHAPE_REPRESENTATION ( #31260, #31351 ) ;
#21866 = VERTEX_POINT ( 'NONE', #11752 ) ;
#21867 = ORIENTED_EDGE ( 'NONE', *, *, #21253, .T. ) ;
#21868 = ORIENTED_EDGE ( 'NONE', *, *, #28970, .F. ) ;
#21869 = DIRECTION ( 'NONE',  ( 0.000000000000000000, -1.000000000000000000, 6.842277657836020854E-49 ) ) ;
#21870 = CIRCLE ( 'NONE', #20186, 7.999999999999986677 ) ;
#21871 = DIRECTION ( 'NONE',  ( 0.000000000000000000, 0.000000000000000000, 1.000000000000000000 ) ) ;
#21872 = ORIENTED_EDGE ( 'NONE', *, *, #19019, .T. ) ;
#21873 = DIRECTION ( 'NONE',  ( 3.697785493223492838E-32, 1.934419779023891545E-16, -1.000000000000000000 ) ) ;
#21874 = AXIS2_PLACEMENT_3D ( 'NONE', #17324, #1279, #33665 ) ;
#21875 = VERTEX_POINT ( 'NONE', #27578 ) ;
#21876 = ORIENTED_EDGE ( 'NONE', *, *, #20959, .T. ) ;
#21877 = VECTOR ( 'NONE', #9436, 1000.000000000000000 ) ;
#21878 = CYLINDRICAL_SURFACE ( 'NONE', #410, 2.033421858999711951 ) ;
#21879 = ORIENTED_EDGE ( 'NONE', *, *, #6070, .F. ) ;
#21880 = AXIS2_PLACEMENT_3D ( 'NONE', #2287, #7806, #16019 ) ;
#21881 = DIRECTION ( 'NONE',  ( 1.000000000000000000, 0.000000000000000000, 0.000000000000000000 ) ) ;
#21882 = DIRECTION ( 'NONE',  ( 1.000000000000000000, 0.000000000000000000, 0.000000000000000000 ) ) ;
#21883 = ORIENTED_EDGE ( 'NONE', *, *, #20256, .T. ) ;
#21884 = EDGE_LOOP ( 'NONE', ( #1997, #26231, #18573, #24163, #23961, #34463, #12120, #23314 ) ) ;
#21885 = CARTESIAN_POINT ( 'NONE',  ( 11.99999999999999645, -124.9999999999999432, -190.9999999999999432 ) ) ;
#21886 = EDGE_CURVE ( 'NONE', #28031, #28204, #28108, .T. ) ;
#21887 = CARTESIAN_POINT ( 'NONE',  ( 6.078604839177344843, 33.69708579775584667, 68.31122994652405112 ) ) ;
#21888 = ORIENTED_EDGE ( 'NONE', *, *, #10737, .T. ) ;
#21889 = CYLINDRICAL_SURFACE ( 'NONE', #20899, 16.19999999999999574 ) ;
#21890 = DIRECTION ( 'NONE',  ( -1.000000000000000000, -0.000000000000000000, -0.000000000000000000 ) ) ;
#21891 = EDGE_CURVE ( 'NONE', #31620, #21809, #9243, .T. ) ;
#21892 = DIRECTION ( 'NONE',  ( 0.000000000000000000, 0.000000000000000000, 1.000000000000000000 ) ) ;
#21893 = CARTESIAN_POINT ( 'NONE',  ( 9.199999999999999289, 0.000000000000000000, 0.000000000000000000 ) ) ;
#21894 = CIRCLE ( 'NONE', #17937, 0.3000000000000016542 ) ;
#21895 = DIRECTION ( 'NONE',  ( 1.000000000000000000, -0.000000000000000000, -0.000000000000000000 ) ) ;
#21896 = CARTESIAN_POINT ( 'NONE',  ( -365.0000000000000000, -133.0000000000000000, 126.0000000000000000 ) ) ;
#21898 = EDGE_CURVE ( 'NONE', #21805, #18796, #15192, .T. ) ;
#21897 = CARTESIAN_POINT ( 'NONE',  ( -14.84098889165990620, 28.96462362251114087, 68.31122994652405112 ) ) ;
#21899 = AXIS2_PLACEMENT_3D ( 'NONE', #18106, #20237, #3663 ) ;
#21900 = PLANE ( 'NONE',  #29526 ) ;
#21901 = ORIENTED_EDGE ( 'NONE', *, *, #13820, .F. ) ;
#21902 = EDGE_CURVE ( 'NONE', #9877, #3883, #16923, .T. ) ;
#21904 = CIRCLE ( 'NONE', #20217, 3.999999999999989786 ) ;
#21903 = CARTESIAN_POINT ( 'NONE',  ( -19.99999999999998934, 136.9999999999999716, -155.0000000000000000 ) ) ;
#21905 = CARTESIAN_POINT ( 'NONE',  ( 837.4366790669032525, 1157.929787158297358, 1753.598338701303419 ) ) ;
#21906 =( REPRESENTATION_RELATIONSHIP ('NONE','NONE', #23037, #19821 ) REPRESENTATION_RELATIONSHIP_WITH_TRANSFORMATION ( #9263 )SHAPE_REPRESENTATION_RELATIONSHIP( ) );
#21907 = AXIS2_PLACEMENT_3D ( 'NONE', #23569, #18086, #29264 ) ;
#21908 = ORIENTED_EDGE ( 'NONE', *, *, #6665, .T. ) ;
#21909 = CLOSED_SHELL ( 'NONE', ( #24742, #2774, #24777, #32077, #19491, #5440, #14573, #24557, #24947, #5770, #17238, #34467, #24812, #15935, #23672, #3515, #26767, #12433, #22683, #25541, #12588, #1454, #15933, #9640, #26585, #13828 ) ) ;
#21910 = ORIENTED_EDGE ( 'NONE', *, *, #23924, .T. ) ;
#21911 = ADVANCED_FACE ( 'NONE', ( #25430 ), #360, .F. ) ;
#21912 = EDGE_CURVE ( 'NONE', #7236, #10395, #14648, .T. ) ;
#21913 = DIRECTION ( 'NONE',  ( -0.000000000000000000, -1.000000000000000000, -0.000000000000000000 ) ) ;
#21914 = ITEM_DEFINED_TRANSFORMATION ( 'NONE', 'NONE', #18363,  #28566 ) ;
#21915 = ORIENTED_EDGE ( 'NONE', *, *, #9790, .F. ) ;
#21916 = CARTESIAN_POINT ( 'NONE',  ( 21.85761591200894216, 30.91355005303805825, 68.31122994652405112 ) ) ;
#21917 = PRESENTATION_STYLE_ASSIGNMENT (( #14091 ) ) ;
#21918 = VECTOR ( 'NONE', #18002, 1000.000000000000000 ) ;
#21920 = FACE_OUTER_BOUND ( 'NONE', #30245, .T. ) ;
#21919 = CARTESIAN_POINT ( 'NONE',  ( -70.00000000000000000, 4.559999999999908127, -172.9900000000000091 ) ) ;
#21921 = EDGE_LOOP ( 'NONE', ( #25567, #23866, #5162, #6340 ) ) ;
#21922 = ORIENTED_EDGE ( 'NONE', *, *, #34316, .T. ) ;
#21923 = LINE ( 'NONE', #211, #24805 ) ;
#21924 = DIRECTION ( 'NONE',  ( -1.000000000000000000, 0.000000000000000000, 0.000000000000000000 ) ) ;
#21925 = VECTOR ( 'NONE', #21048, 1000.000000000000000 ) ;
#21926 = CARTESIAN_POINT ( 'NONE',  ( -5.527271473480783293, -1.747512292859696226, -0.7500000000000000000 ) ) ;
#21927 = FACE_OUTER_BOUND ( 'NONE', #19888, .T. ) ;
#21928 = CARTESIAN_POINT ( 'NONE',  ( -12.00000000000001066, 124.9999999999999716, 155.0000000000000000 ) ) ;
#21929 = EDGE_LOOP ( 'NONE', ( #27289, #11286, #5686, #14534 ) ) ;
#21930 = CARTESIAN_POINT ( 'NONE',  ( -500.0000000000000000, -113.0000000000000000, 187.0000000000000000 ) ) ;
#21931 = LINE ( 'NONE', #10901, #29909 ) ;
#21932 = LINE ( 'NONE', #10902, #30567 ) ;
#21933 = AXIS2_PLACEMENT_3D ( 'NONE', #30828, #28339, #11623 ) ;
#21934 = CARTESIAN_POINT ( 'NONE',  ( 2.606461854930495203, 32.14582644238495135, -2.841494734165257885 ) ) ;
#21935 =( LENGTH_UNIT ( ) NAMED_UNIT ( * ) SI_UNIT ( .MILLI., .METRE. ) );
#21936 = DIRECTION ( 'NONE',  ( 0.000000000000000000, 0.000000000000000000, 1.000000000000000000 ) ) ;
#21938 = CARTESIAN_POINT ( 'NONE',  ( -418.0000000000000000, 145.0000000000000000, -175.0000000000000000 ) ) ;
#21937 = LINE ( 'NONE', #224, #30394 ) ;
#21939 = AXIS2_PLACEMENT_3D ( 'NONE', #17918, #12222, #23071 ) ;
#21940 = CARTESIAN_POINT ( 'NONE',  ( -418.0000000000000000, 105.0000000000000142, 162.9999999999999716 ) ) ;
#21941 = ORIENTED_EDGE ( 'NONE', *, *, #29209, .T. ) ;
#21942 = LINE ( 'NONE', #19287, #3097 ) ;
#21944 = LINE ( 'NONE', #30125, #28793 ) ;
#21943 = DIRECTION ( 'NONE',  ( -0.000000000000000000, -0.000000000000000000, 1.000000000000000000 ) ) ;
#21945 = MANIFOLD_SOLID_BREP ( 'Square tube 40 X 40 X 4(1)[6]', #3714 ) ;
#21946 = ADVANCED_FACE ( 'NONE', ( #11217 ), #11930, .F. ) ;
#21947 = VECTOR ( 'NONE', #19307, 1000.000000000000000 ) ;
#21948 = EDGE_LOOP ( 'NONE', ( #23934, #29666, #12450, #3906 ) ) ;
#21949 = ADVANCED_FACE ( 'NONE', ( #11386 ), #22773, .F. ) ;
#21950 = ADVANCED_FACE ( 'NONE', ( #21279 ), #29467, .T. ) ;
#21951 = CARTESIAN_POINT ( 'NONE',  ( 25.76952721012208514, 19.87802405277947315, 68.31122994652405112 ) ) ;
#21952 = CIRCLE ( 'NONE', #4884, 4.309328216469825001 ) ;
#21953 = ORIENTED_EDGE ( 'NONE', *, *, #855, .F. ) ;
#21954 =( REPRESENTATION_RELATIONSHIP ('NONE','NONE', #23037, #28231 ) REPRESENTATION_RELATIONSHIP_WITH_TRANSFORMATION ( #15901 )SHAPE_REPRESENTATION_RELATIONSHIP( ) );
#21955 = ORIENTED_EDGE ( 'NONE', *, *, #15053, .T. ) ;
#21956 = CARTESIAN_POINT ( 'NONE',  ( -117.4999999999997442, 0.000000000000000000, -12.50000000000000000 ) ) ;
#21957 = VERTEX_POINT ( 'NONE', #9598 ) ;
#21958 = EDGE_LOOP ( 'NONE', ( #6062, #25500, #21046, #15016 ) ) ;
#21959 = LINE ( 'NONE', #30674, #15052 ) ;
#21960 = AXIS2_PLACEMENT_3D ( 'NONE', #23427, #23940, #15430 ) ;
#21961 = EDGE_CURVE ( 'NONE', #26015, #18709, #34808, .T. ) ;
#21962 = ITEM_DEFINED_TRANSFORMATION ( 'NONE', 'NONE', #8149,  #28566 ) ;
#21963 = FACE_OUTER_BOUND ( 'NONE', #34123, .T. ) ;
#21964 = CARTESIAN_POINT ( 'NONE',  ( 2.789999999999999147, -27.53147453683415335, -13.05640081644869532 ) ) ;
#21965 = ORIENTED_EDGE ( 'NONE', *, *, #2036, .F. ) ;
#21966 = ORIENTED_EDGE ( 'NONE', *, *, #7875, .T. ) ;
#21967 = CARTESIAN_POINT ( 'NONE',  ( 18.92820323027550344, -55.00000000000000711, -158.9999999999999716 ) ) ;
#21968 = CARTESIAN_POINT ( 'NONE',  ( -117.4999999999997442, 0.000000000000000000, 0.000000000000000000 ) ) ;
#21969 = ADVANCED_FACE ( 'NONE', ( #4701 ), #6735, .T. ) ;
#21970 = CARTESIAN_POINT ( 'NONE',  ( 105.3825092702455777, -5.728493955922442815, -11.11012212270734167 ) ) ;
#21971 = CYLINDRICAL_SURFACE ( 'NONE', #8013, 32.54542015209057126 ) ;
#21972 = ORIENTED_EDGE ( 'NONE', *, *, #23464, .F. ) ;
#21973 = EDGE_CURVE ( 'NONE', #15156, #6016, #32297, .T. ) ;
#21974 = CARTESIAN_POINT ( 'NONE',  ( -365.0000000000000000, 114.9999999999999574, 113.9999999999999858 ) ) ;
#21975 = EDGE_CURVE ( 'NONE', #6239, #28175, #34552, .T. ) ;
#21976 = DIRECTION ( 'NONE',  ( 1.232595164407830946E-32, 7.496237820289040735E-63, -1.000000000000000000 ) ) ;
#21977 = ORIENTED_EDGE ( 'NONE', *, *, #9384, .T. ) ;
#21978 = VECTOR ( 'NONE', #30520, 1000.000000000000000 ) ;
#21979 = LINE ( 'NONE', #2920, #14610 ) ;
#21980 = ADVANCED_FACE ( 'NONE', ( #29108 ), #34991, .T. ) ;
#21981 = CARTESIAN_POINT ( 'NONE',  ( -499.9999999999999432, -141.0000000000000000, -187.0000000000000000 ) ) ;
#21982 = CYLINDRICAL_SURFACE ( 'NONE', #7551, 7.999999999999979572 ) ;
#21983 = CARTESIAN_POINT ( 'NONE',  ( 2.765921099433442443, 7.350529080603967813, -30.20932655202929595 ) ) ;
#21984 = ORIENTED_EDGE ( 'NONE', *, *, #4431, .F. ) ;
#21985 = DIRECTION ( 'NONE',  ( 0.000000000000000000, 0.000000000000000000, 1.000000000000000000 ) ) ;
#21986 = EDGE_LOOP ( 'NONE', ( #28370, #21808, #28519, #31175, #5435, #15852, #14260, #10597 ) ) ;
#21988 = DIRECTION ( 'NONE',  ( 1.000000000000000000, 0.000000000000000000, 0.000000000000000000 ) ) ;
#21987 = CARTESIAN_POINT ( 'NONE',  ( 0.006892382735981021635, 25.89094059359475253, 16.81082004999792545 ) ) ;
#21990 = CIRCLE ( 'NONE', #18577, 30.47050528711511674 ) ;
#21989 = FACE_OUTER_BOUND ( 'NONE', #20830, .T. ) ;
#21991 = ORIENTED_EDGE ( 'NONE', *, *, #5891, .F. ) ;
#21992 = EDGE_CURVE ( 'NONE', #23843, #34921, #3967, .T. ) ;
#21993 = ADVANCED_FACE ( 'NONE', ( #2398 ), #12104, .F. ) ;
#21994 = DIRECTION ( 'NONE',  ( -1.000000000000000000, 0.000000000000000000, -0.000000000000000000 ) ) ;
#21995 = PRODUCT_DEFINITION_SHAPE ( 'NONE', 'NONE',  #25992 ) ;
#21996 = CARTESIAN_POINT ( 'NONE',  ( 0.000000000000000000, -33.69708579775584667, 49.43553178847298568 ) ) ;
#21997 = ORIENTED_EDGE ( 'NONE', *, *, #18503, .F. ) ;
#21998 = CIRCLE ( 'NONE', #35065, 7.999999999999979572 ) ;
#21999 = ORIENTED_EDGE ( 'NONE', *, *, #8928, .F. ) ;
#22000 = CARTESIAN_POINT ( 'NONE',  ( 0.000000000000000000, -3.728217946242704972, -30.24156218513559580 ) ) ;
#22001 = CARTESIAN_POINT ( 'NONE',  ( -100.4259553087715204, 2.313922778582933937, 7.141321738367093275 ) ) ;
#22002 = VERTEX_POINT ( 'NONE', #4053 ) ;
#22003 = EDGE_LOOP ( 'NONE', ( #30666, #33991, #25586, #31359 ) ) ;
#22004 = CARTESIAN_POINT ( 'NONE',  ( 11.99999999999999645, 134.9999999999999432, -162.9999999999999432 ) ) ;
#22005 = LINE ( 'NONE', #5962, #14182 ) ;
#22006 = ADVANCED_BREP_SHAPE_REPRESENTATION ( '', ( #34055, #28566 ), #32533 ) ;
#22007 = LINE ( 'NONE', #27862, #33362 ) ;
#22008 = DIRECTION ( 'NONE',  ( 0.000000000000000000, 0.7071067811865462405, -0.7071067811865489050 ) ) ;
#22009 = VERTEX_POINT ( 'NONE', #21453 ) ;
#22010 = VERTEX_POINT ( 'NONE', #7919 ) ;
#22011 = LINE ( 'NONE', #32853, #21345 ) ;
#22012 = DIRECTION ( 'NONE',  ( -1.000000000000000000, 0.000000000000000000, 0.000000000000000000 ) ) ;
#22013 = CARTESIAN_POINT ( 'NONE',  ( -365.0000000000000000, 118.9999999999999716, 113.9999999999999858 ) ) ;
#22014 = CARTESIAN_POINT ( 'NONE',  ( 117.4999999999998579, 0.000000000000000000, 0.000000000000000000 ) ) ;
#22015 = ADVANCED_FACE ( 'NONE', ( #9428 ), #20284, .T. ) ;
#22016 = ADVANCED_FACE ( 'NONE', ( #2059 ), #15955, .T. ) ;
#22017 = CARTESIAN_POINT ( 'NONE',  ( -30.91434716440808472, 10.17386417614055105, -36.68877005347593467 ) ) ;
#22018 = LINE ( 'NONE', #30376, #25418 ) ;
#22019 = LINE ( 'NONE', #127, #19276 ) ;
#22020 = EDGE_LOOP ( 'NONE', ( #18158, #14392, #13311, #25672 ) ) ;
#22021 = CARTESIAN_POINT ( 'NONE',  ( 0.000000000000000000, 0.000000000000000000, 20.00000000000000000 ) ) ;
#22022 = EDGE_CURVE ( 'NONE', #8902, #18426, #23772, .T. ) ;
#22023 = CARTESIAN_POINT ( 'NONE',  ( 1.040000000000000924, 0.000000000000000000, 0.000000000000000000 ) ) ;
#22024 = PLANE ( 'NONE',  #30264 ) ;
#22025 = ORIENTED_EDGE ( 'NONE', *, *, #10314, .F. ) ;
#22026 = AXIS2_PLACEMENT_3D ( 'NONE', #2614, #13482, #32505 ) ;
#22027 = AXIS2_PLACEMENT_3D ( 'NONE', #14989, #17501, #1275 ) ;
#22028 = ADVANCED_FACE ( 'NONE', ( #21096 ), #26785, .F. ) ;
#22029 = CARTESIAN_POINT ( 'NONE',  ( -20.02113311122488781, 8.235406450278427215, -67.50000000000000000 ) ) ;
#22030 = EDGE_LOOP ( 'NONE', ( #8607, #2576, #27155, #7036 ) ) ;
#22031 = DIRECTION ( 'NONE',  ( -1.000000000000000000, -0.000000000000000000, -0.000000000000000000 ) ) ;
#22032 = CARTESIAN_POINT ( 'NONE',  ( -104.3244124248265052, 5.081434799294422433, 11.42078282599712935 ) ) ;
#22033 = ORIENTED_EDGE ( 'NONE', *, *, #11509, .F. ) ;
#22034 = CARTESIAN_POINT ( 'NONE',  ( -418.0000000000000568, 105.0000000000000142, 104.0000000000000142 ) ) ;
#22035 = CARTESIAN_POINT ( 'NONE',  ( 10.00000000000000000, -15.58845726811992627, 0.000000000000000000 ) ) ;
#22036 = CARTESIAN_POINT ( 'NONE',  ( -32.54223829851967764, 0.4550817492056293823, -36.68877005347593467 ) ) ;
#22037 = ORIENTED_EDGE ( 'NONE', *, *, #32141, .F. ) ;
#22038 = ORIENTED_EDGE ( 'NONE', *, *, #30033, .T. ) ;
#22039 = VECTOR ( 'NONE', #18813, 1000.000000000000000 ) ;
#22040 = DIRECTION ( 'NONE',  ( 0.1063910735368947813, -0.9943243633099144718, -3.335902418024520312E-15 ) ) ;
#22041 = FACE_OUTER_BOUND ( 'NONE', #27864, .T. ) ;
#22042 = ADVANCED_FACE ( 'NONE', ( #18450 ), #15780, .F. ) ;
#22043 = EDGE_LOOP ( 'NONE', ( #11978, #32395, #6532, #3587 ) ) ;
#22044 = DIRECTION ( 'NONE',  ( -0.1081190184239421148, 0.9941379571543595972, -0.000000000000000000 ) ) ;
#22045 = CARTESIAN_POINT ( 'NONE',  ( 2.604019708820032530, -32.25918669212989442, 1.206152977787649405 ) ) ;
#22046 = CIRCLE ( 'NONE', #6693, 6.898500000000000298 ) ;
#22047 = AXIS2_PLACEMENT_3D ( 'NONE', #11389, #11039, #14249 ) ;
#22048 = CARTESIAN_POINT ( 'NONE',  ( 2.033800774695602165, 14.91862693714182875, -30.45773629169350727 ) ) ;
#22049 = CARTESIAN_POINT ( 'NONE',  ( 110.6956932917700271, -0.7984011589207654636, 7.467432841349395112 ) ) ;
#22050 = ITEM_DEFINED_TRANSFORMATION ( 'NONE', 'NONE', #14984,  #28566 ) ;
#22051 = ORIENTED_EDGE ( 'NONE', *, *, #6576, .F. ) ;
#22052 = VERTEX_POINT ( 'NONE', #268 ) ;
#22053 = ORIENTED_EDGE ( 'NONE', *, *, #3603, .F. ) ;
#22054 = DIRECTION ( 'NONE',  ( 0.5155538571770196254, 0.8568571761675904952, 1.574021097180118762E-16 ) ) ;
#22055 = EDGE_CURVE ( 'NONE', #20418, #26158, #24626, .T. ) ;
#22056 = LINE ( 'NONE', #32899, #27374 ) ;
#22057 = AXIS2_PLACEMENT_3D ( 'NONE', #12921, #24270, #24436 ) ;
#22058 = EDGE_CURVE ( 'NONE', #1154, #20834, #30335, .T. ) ;
#22059 = EDGE_CURVE ( 'NONE', #15373, #21689, #24813, .T. ) ;
#22060 = CARTESIAN_POINT ( 'NONE',  ( 2.261199749961548378, -23.80541455566248388, 23.41327456068864876 ) ) ;
#22061 = ORIENTED_EDGE ( 'NONE', *, *, #9052, .F. ) ;
#22062 = VERTEX_POINT ( 'NONE', #10946 ) ;
#22063 = DIRECTION ( 'NONE',  ( -1.000000000000000000, 0.000000000000000000, 0.000000000000000000 ) ) ;
#22064 = ORIENTED_EDGE ( 'NONE', *, *, #14015, .T. ) ;
#22065 = CARTESIAN_POINT ( 'NONE',  ( -499.9999999999998863, -109.0000000000000142, -162.9999999999999716 ) ) ;
#22066 = DIRECTION ( 'NONE',  ( 0.000000000000000000, 1.000000000000000000, 0.000000000000000000 ) ) ;
#22067 = VERTEX_POINT ( 'NONE', #13796 ) ;
#22068 = ORIENTED_EDGE ( 'NONE', *, *, #6942, .F. ) ;
#22069 = DIRECTION ( 'NONE',  ( -1.000000000000000000, 0.000000000000000000, 0.000000000000000000 ) ) ;
#22070 = AXIS2_PLACEMENT_3D ( 'NONE', #15186, #34393, #32061 ) ;
#22071 = CARTESIAN_POINT ( 'NONE',  ( 35.44043929807611448, -32.65143121711728469, 10.00000000000000000 ) ) ;
#22072 = ORIENTED_EDGE ( 'NONE', *, *, #13239, .T. ) ;
#22073 = CARTESIAN_POINT ( 'NONE',  ( -9.978866888775632660, -5.758675521474015291, -67.50000000000000000 ) ) ;
#22074 = DIRECTION ( 'NONE',  ( 0.000000000000000000, 1.836970198721029934E-16, -1.000000000000000000 ) ) ;
#22075 = CARTESIAN_POINT ( 'NONE',  ( 1.341640786499872284, 0.000000000000000000, 14.20000000000000107 ) ) ;
#22076 =( NAMED_UNIT ( * ) SI_UNIT ( $, .STERADIAN. ) SOLID_ANGLE_UNIT ( ) );
#22077 = AXIS2_PLACEMENT_3D ( 'NONE', #31659, #33992, #28996 ) ;
#22078 = CARTESIAN_POINT ( 'NONE',  ( 2.604019707142743112, -3.229344000442307738, -32.11979559073833457 ) ) ;
#22079 = CARTESIAN_POINT ( 'NONE',  ( 11.99999999999999645, -115.0000000000000142, 159.0000000000000000 ) ) ;
#22080 =( LENGTH_UNIT ( ) NAMED_UNIT ( * ) SI_UNIT ( .MILLI., .METRE. ) );
#22081 = AXIS2_PLACEMENT_3D ( 'NONE', #3878, #4046, #14596 ) ;
#22082 = ORIENTED_EDGE ( 'NONE', *, *, #33390, .F. ) ;
#22083 = DIRECTION ( 'NONE',  ( -0.9868265225415260300, 0.1617819965527647341, 0.000000000000000000 ) ) ;
#22084 = DIRECTION ( 'NONE',  ( 2.631201909438060269E-14, -5.396010391056495992E-16, 0.9999999999999998890 ) ) ;
#22085 = EDGE_LOOP ( 'NONE', ( #25671, #32158, #17863, #7355 ) ) ;
#22086 = ORIENTED_EDGE ( 'NONE', *, *, #22543, .F. ) ;
#22087 = AXIS2_PLACEMENT_3D ( 'NONE', #18877, #32906, #29549 ) ;
#22088 = VECTOR ( 'NONE', #22274, 1000.000000000000000 ) ;
#22089 = DIRECTION ( 'NONE',  ( -1.000000000000000000, -0.000000000000000000, -0.000000000000000000 ) ) ;
#22090 = APPLICATION_PROTOCOL_DEFINITION ( 'draft international standard', 'automotive_design', 1998, #4164 ) ;
#22091 = EDGE_CURVE ( 'NONE', #26985, #31534, #29391, .T. ) ;
#22092 = EDGE_LOOP ( 'NONE', ( #24195, #23183, #6078, #11095, #8946, #25180, #3642, #6616 ) ) ;
#22093 = CARTESIAN_POINT ( 'NONE',  ( 9.199999999999999289, 7.794228634059941818, 13.49999999999999645 ) ) ;
#22094 = DIRECTION ( 'NONE',  ( 0.000000000000000000, 1.000000000000000000, 1.224646799147353207E-16 ) ) ;
#22095 = ADVANCED_FACE ( 'NONE', ( #19319 ), #2749, .T. ) ;
#22096 = ITEM_DEFINED_TRANSFORMATION ( 'NONE', 'NONE', #22388,  #28566 ) ;
#22097 = VECTOR ( 'NONE', #3344, 1000.000000000000000 ) ;
#22098 = EDGE_CURVE ( 'NONE', #27476, #8689, #33178, .T. ) ;
#22100 = DIRECTION ( 'NONE',  ( -1.232595164407830946E-32, 0.000000000000000000, -1.000000000000000000 ) ) ;
#22099 = CARTESIAN_POINT ( 'NONE',  ( -365.0000000000000000, -125.0000000000000284, 168.9999999999999716 ) ) ;
#22101 = ORIENTED_EDGE ( 'NONE', *, *, #31094, .F. ) ;
#22102 = ORIENTED_EDGE ( 'NONE', *, *, #11395, .F. ) ;
#22103 = CARTESIAN_POINT ( 'NONE',  ( -349.0000000000000000, 124.9999999999999432, 168.9999999999999716 ) ) ;
#22104 = CARTESIAN_POINT ( 'NONE',  ( 19.99999999999998934, 144.9999999999999716, 187.0000000000000000 ) ) ;
#22105 = EDGE_CURVE ( 'NONE', #8775, #16257, #5414, .T. ) ;
#22106 = DIRECTION ( 'NONE',  ( 1.000000000000000000, 0.000000000000000000, 0.000000000000000000 ) ) ;
#22107 = CYLINDRICAL_SURFACE ( 'NONE', #4005, 34.41491905851385269 ) ;
#22108 = CARTESIAN_POINT ( 'NONE',  ( 0.000000000000000000, 14.59907093257217170, 26.74544485249471393 ) ) ;
#22109 = ORIENTED_EDGE ( 'NONE', *, *, #29776, .F. ) ;
#22110 = AXIS2_PLACEMENT_3D ( 'NONE', #16345, #32506, #29675 ) ;
#22111 = FACE_OUTER_BOUND ( 'NONE', #7821, .T. ) ;
#22112 = CARTESIAN_POINT ( 'NONE',  ( 2.789999999999999147, 0.000000000000000000, 0.000000000000000000 ) ) ;
#22113 = DIRECTION ( 'NONE',  ( 1.232595164407830946E-32, 0.000000000000000000, 1.000000000000000000 ) ) ;
#22114 = VERTEX_POINT ( 'NONE', #27663 ) ;
#22115 = LINE ( 'NONE', #3234, #33374 ) ;
#22116 =( LENGTH_UNIT ( ) NAMED_UNIT ( * ) SI_UNIT ( .MILLI., .METRE. ) );
#22117 = EDGE_CURVE ( 'NONE', #3175, #18752, #8799, .T. ) ;
#22118 = CARTESIAN_POINT ( 'NONE',  ( 1.749999999999999778, 0.000000000000000000, 0.000000000000000000 ) ) ;
#22120 = CARTESIAN_POINT ( 'NONE',  ( -0.7181323043387221050, -1.866624223957557893, -0.7500000000000000000 ) ) ;
#22119 = DIRECTION ( 'NONE',  ( -0.000000000000000000, 1.000000000000000000, -0.000000000000000000 ) ) ;
#22121 = VECTOR ( 'NONE', #23080, 1000.000000000000000 ) ;
#22122 = DIRECTION ( 'NONE',  ( -1.000000000000000000, -0.000000000000000000, -0.000000000000000000 ) ) ;
#22123 = ORIENTED_EDGE ( 'NONE', *, *, #4109, .F. ) ;
#22124 = CARTESIAN_POINT ( 'NONE',  ( 1.749999999999999778, 0.000000000000000000, 0.000000000000000000 ) ) ;
#22125 = DIRECTION ( 'NONE',  ( 1.000000000000000000, 0.000000000000000000, 0.000000000000000000 ) ) ;
#22126 = AXIS2_PLACEMENT_3D ( 'NONE', #7495, #5001, #33733 ) ;
#22127 = VERTEX_POINT ( 'NONE', #88 ) ;
#22128 = EDGE_LOOP ( 'NONE', ( #4487, #31606, #6770, #16277 ) ) ;
#22129 = VECTOR ( 'NONE', #20578, 1000.000000000000000 ) ;
#22130 = ORIENTED_EDGE ( 'NONE', *, *, #721, .F. ) ;
#22131 = CARTESIAN_POINT ( 'NONE',  ( -5.021133111225092982, -15.68591377522703390, -87.50000000000000000 ) ) ;
#22132 = ORIENTED_EDGE ( 'NONE', *, *, #28452, .F. ) ;
#22133 = ORIENTED_EDGE ( 'NONE', *, *, #23466, .F. ) ;
#22134 = LINE ( 'NONE', #425, #14493 ) ;
#22135 = EDGE_CURVE ( 'NONE', #24766, #2999, #616, .T. ) ;
#22136 = B_SPLINE_CURVE_WITH_KNOTS ( 'NONE', 3,
 ( #4450, #30827, #2311, #4800, #7471, #34365 ),
 .UNSPECIFIED., .F., .F.,
 ( 4, 2, 4 ),
 ( 4.404817020008189394E-07, 0.001874269619297513683, 0.003748098756893026608 ),
 .UNSPECIFIED. ) ;
#22137 = VECTOR ( 'NONE', #31884, 1000.000000000000000 ) ;
#22138 = VERTEX_POINT ( 'NONE', #16127 ) ;
#22139 = CARTESIAN_POINT ( 'NONE',  ( -34.66645501699844090, -15.21971901163153440, -36.68877005347593467 ) ) ;
#22140 = CARTESIAN_POINT ( 'NONE',  ( -442.0000000000000000, -105.0000000000000142, 100.0000000000000000 ) ) ;
#22141 = ORIENTED_EDGE ( 'NONE', *, *, #5632, .T. ) ;
#22142 = VERTEX_POINT ( 'NONE', #13978 ) ;
#22143 = CARTESIAN_POINT ( 'NONE',  ( -22.50000000000000355, 0.000000000000000000, 20.00000000000000000 ) ) ;
#22144 = CARTESIAN_POINT ( 'NONE',  ( -12.00000000000001066, 112.9999999999999574, -175.0000000000000284 ) ) ;
#22145 = EDGE_CURVE ( 'NONE', #34660, #3220, #16678, .T. ) ;
#22146 = EDGE_CURVE ( 'NONE', #32609, #17061, #18966, .T. ) ;
#22147 = LINE ( 'NONE', #11465, #6188 ) ;
#22148 = DIRECTION ( 'NONE',  ( 0.000000000000000000, 1.000000000000000000, 0.000000000000000000 ) ) ;
#22149 = EDGE_LOOP ( 'NONE', ( #31501, #11949, #33285, #3915 ) ) ;
#22150 = DIRECTION ( 'NONE',  ( 0.000000000000000000, 0.000000000000000000, -1.000000000000000000 ) ) ;
#22151 = EDGE_CURVE ( 'NONE', #13451, #7267, #7822, .T. ) ;
#22152 = EDGE_CURVE ( 'NONE', #11554, #10950, #16306, .T. ) ;
#22153 = CARTESIAN_POINT ( 'NONE',  ( 3.235562306570555532E-30, -5.758675521474011738, -87.50000000000000000 ) ) ;
#22154 = ORIENTED_EDGE ( 'NONE', *, *, #19494, .T. ) ;
#22155 = DIRECTION ( 'NONE',  ( 0.000000000000000000, 1.836970198721029441E-16, -1.000000000000000000 ) ) ;
#22156 = CARTESIAN_POINT ( 'NONE',  ( -1.341640786499875171, 0.000000000000000000, -11.80000000000000071 ) ) ;
#22157 = CARTESIAN_POINT ( 'NONE',  ( 1.749999999999999778, -33.26546734453812348, -8.820166447042147695 ) ) ;
#22158 = AXIS2_PLACEMENT_3D ( 'NONE', #22215, #8681, #19557 ) ;
#22159 = PLANE ( 'NONE',  #5804 ) ;
#22160 = ORIENTED_EDGE ( 'NONE', *, *, #32103, .T. ) ;
#22161 = DIRECTION ( 'NONE',  ( 0.000000000000000000, 1.000000000000000000, 0.000000000000000000 ) ) ;
#22162 = ORIENTED_EDGE ( 'NONE', *, *, #28168, .F. ) ;
#22163 = CARTESIAN_POINT ( 'NONE',  ( -10.00000000000000000, 0.000000000000000000, 0.000000000000000000 ) ) ;
#22164 = ADVANCED_FACE ( 'NONE', ( #24280 ), #21982, .T. ) ;
#22165 = ORIENTED_EDGE ( 'NONE', *, *, #25188, .T. ) ;
#22166 =( REPRESENTATION_RELATIONSHIP ('NONE','NONE', #23037, #15767 ) REPRESENTATION_RELATIONSHIP_WITH_TRANSFORMATION ( #32014 )SHAPE_REPRESENTATION_RELATIONSHIP( ) );
#22167 = CYLINDRICAL_SURFACE ( 'NONE', #34795, 3.999999999999976019 ) ;
#22168 = FACE_OUTER_BOUND ( 'NONE', #333, .T. ) ;
#22169 = ORIENTED_EDGE ( 'NONE', *, *, #22676, .T. ) ;
#22170 = ORIENTED_EDGE ( 'NONE', *, *, #4162, .T. ) ;
#22171 = ADVANCED_FACE ( 'NONE', ( #8616 ), #19495, .T. ) ;
#22172 = EDGE_CURVE ( 'NONE', #7199, #199, #27304, .T. ) ;
#22173 = EDGE_LOOP ( 'NONE', ( #20309, #14722, #11139, #31642 ) ) ;
#22174 = DIRECTION ( 'NONE',  ( -1.000000000000000000, -0.000000000000000000, -0.000000000000000000 ) ) ;
#22175 = FACE_OUTER_BOUND ( 'NONE', #4746, .T. ) ;
#22176 = ORIENTED_EDGE ( 'NONE', *, *, #33893, .T. ) ;
#22177 = ORIENTED_EDGE ( 'NONE', *, *, #14218, .F. ) ;
#22178 = DIRECTION ( 'NONE',  ( 1.000000000000000000, 0.000000000000000000, 0.000000000000000000 ) ) ;
#22179 = VECTOR ( 'NONE', #6046, 1000.000000000000000 ) ;
#22180 = CARTESIAN_POINT ( 'NONE',  ( -12.00000000000001066, 144.9999999999999716, 159.0000000000000000 ) ) ;
#22181 = CARTESIAN_POINT ( 'NONE',  ( 12.00000000000001066, -64.99999999999997158, -175.0000000000000000 ) ) ;
#22182 = LINE ( 'NONE', #18650, #30147 ) ;
#22183 = ORIENTED_EDGE ( 'NONE', *, *, #12361, .T. ) ;
#22184 = VERTEX_POINT ( 'NONE', #33892 ) ;
#22185 = DIRECTION ( 'NONE',  ( 0.000000000000000000, -0.08715574274765887364, -0.9961946980917455452 ) ) ;
#22186 = DIRECTION ( 'NONE',  ( -0.6051742151937647973, -0.7960930657056438653, -0.000000000000000000 ) ) ;
#22187 = FACE_OUTER_BOUND ( 'NONE', #29715, .T. ) ;
#22188 = DIRECTION ( 'NONE',  ( 0.2149704402110223789, -0.9766205557100871015, -1.794022856297801510E-16 ) ) ;
#22189 = CARTESIAN_POINT ( 'NONE',  ( 0.1859802930121887965, 14.82665350068137933, -28.67542985682306167 ) ) ;
#22190 = EDGE_CURVE ( 'NONE', #31755, #17164, #23487, .T. ) ;
#22191 = EDGE_CURVE ( 'NONE', #33679, #17311, #27839, .T. ) ;
#22192 = PLANE ( 'NONE',  #33373 ) ;
#22193 = LINE ( 'NONE', #6510, #31743 ) ;
#22194 = VERTEX_POINT ( 'NONE', #3970 ) ;
#22195 = CARTESIAN_POINT ( 'NONE',  ( 11.99999999999999645, 124.9999999999999716, 159.0000000000000000 ) ) ;
#22196 = DIRECTION ( 'NONE',  ( 0.000000000000000000, 1.000000000000000000, 1.224646799147353207E-16 ) ) ;
#22197 = DIRECTION ( 'NONE',  ( 1.000000000000000000, 3.040835319149746090E-31, 1.232595164407830946E-32 ) ) ;
#22198 = ORIENTED_EDGE ( 'NONE', *, *, #9196, .F. ) ;
#22199 = CARTESIAN_POINT ( 'NONE',  ( -442.0000000000000000, -105.0000000000000142, -77.99999999999997158 ) ) ;
#22200 = ORIENTED_EDGE ( 'NONE', *, *, #17386, .T. ) ;
#22201 = AXIS2_PLACEMENT_3D ( 'NONE', #7067, #17971, #34665 ) ;
#22202 = CARTESIAN_POINT ( 'NONE',  ( 0.000000000000000000, 11.30192140231230091, 28.29696565125076191 ) ) ;
#22203 = PLANE ( 'NONE',  #26811 ) ;
#22204 = VECTOR ( 'NONE', #31117, 1000.000000000000000 ) ;
#22205 = VERTEX_POINT ( 'NONE', #12195 ) ;
#22206 = CYLINDRICAL_SURFACE ( 'NONE', #33641, 13.50000000000000178 ) ;
#22207 = LINE ( 'NONE', #33052, #6556 ) ;
#22208 = DIRECTION ( 'NONE',  ( -0.000000000000000000, 1.000000000000000000, -0.000000000000000000 ) ) ;
#22209 = EDGE_CURVE ( 'NONE', #27507, #18790, #5288, .T. ) ;
#22210 = ORIENTED_EDGE ( 'NONE', *, *, #18415, .T. ) ;
#22211 = EDGE_CURVE ( 'NONE', #13343, #1565, #14694, .T. ) ;
#22212 = EDGE_CURVE ( 'NONE', #29973, #21178, #25341, .T. ) ;
#22213 = DIRECTION ( 'NONE',  ( 2.631201909438060585E-14, -5.396010391056496978E-16, 1.000000000000000000 ) ) ;
#22214 = VECTOR ( 'NONE', #17423, 1000.000000000000000 ) ;
#22215 = CARTESIAN_POINT ( 'NONE',  ( 0.000000000000000000, -49.99999999999999289, 0.000000000000000000 ) ) ;
#22216 = ORIENTED_EDGE ( 'NONE', *, *, #27878, .T. ) ;
#22217 = FACE_OUTER_BOUND ( 'NONE', #25159, .T. ) ;
#22218 = EDGE_CURVE ( 'NONE', #14482, #22312, #33359, .T. ) ;
#22219 = DIRECTION ( 'NONE',  ( 1.000000000000000000, 0.000000000000000000, 0.000000000000000000 ) ) ;
#22220 = ADVANCED_FACE ( 'NONE', ( #28551 ), #15034, .F. ) ;
#22221 = CARTESIAN_POINT ( 'NONE',  ( -363.0000000000000000, -125.0000000000000284, 181.0000000000000000 ) ) ;
#22222 = CARTESIAN_POINT ( 'NONE',  ( -100.1713109292253705, -1.696008709688489047, 7.307621933264760727 ) ) ;
#22223 = CONTEXT_DEPENDENT_SHAPE_REPRESENTATION ( #2150, #17731 ) ;
#22224 = ORIENTED_EDGE ( 'NONE', *, *, #15512, .F. ) ;
#22225 = ORIENTED_EDGE ( 'NONE', *, *, #34523, .F. ) ;
#22226 = ORIENTED_EDGE ( 'NONE', *, *, #33745, .T. ) ;
#22227 = VECTOR ( 'NONE', #7369, 1000.000000000000000 ) ;
#22228 = SURFACE_STYLE_USAGE ( .BOTH. , #25589 ) ;
#22230 = AXIS2_PLACEMENT_3D ( 'NONE', #1351, #12223, #25369 ) ;
#22229 = LINE ( 'NONE', #8694, #27941 ) ;
#22231 = DIRECTION ( 'NONE',  ( 0.000000000000000000, 0.000000000000000000, 1.000000000000000000 ) ) ;
#22232 = EDGE_CURVE ( 'NONE', #32595, #16498, #33147, .T. ) ;
#22233 = ORIENTED_EDGE ( 'NONE', *, *, #559, .F. ) ;
#22234 = ORIENTED_EDGE ( 'NONE', *, *, #24689, .F. ) ;
#22235 = CYLINDRICAL_SURFACE ( 'NONE', #32785, 16.19999999999999574 ) ;
#22236 = ORIENTED_EDGE ( 'NONE', *, *, #20066, .T. ) ;
#22237 = FACE_OUTER_BOUND ( 'NONE', #15860, .T. ) ;
#22238 = DIRECTION ( 'NONE',  ( 0.000000000000000000, 0.000000000000000000, -1.000000000000000000 ) ) ;
#22239 = EDGE_LOOP ( 'NONE', ( #18786, #15270, #15722 ) ) ;
#22240 = ORIENTED_EDGE ( 'NONE', *, *, #10700, .T. ) ;
#22241 = PLANE ( 'NONE',  #8372 ) ;
#22242 = VECTOR ( 'NONE', #4790, 1000.000000000000000 ) ;
#22243 = VECTOR ( 'NONE', #32226, 1000.000000000000000 ) ;
#22245 = CARTESIAN_POINT ( 'NONE',  ( 2.765921099433441110, 11.80989368511462523, 28.76039115933989976 ) ) ;
#22244 = AXIS2_PLACEMENT_3D ( 'NONE', #22163, #6122, #20031 ) ;
#22246 = ORIENTED_EDGE ( 'NONE', *, *, #121, .T. ) ;
#22247 = AXIS2_PLACEMENT_3D ( 'NONE', #3763, #17668, #31177 ) ;
#22248 = DIRECTION ( 'NONE',  ( 0.000000000000000000, 0.000000000000000000, 1.000000000000000000 ) ) ;
#22249 = CARTESIAN_POINT ( 'NONE',  ( -499.9999999999999432, -137.0000000000000000, -190.9999999999999716 ) ) ;
#22250 = FACE_BOUND ( 'NONE', #33364, .T. ) ;
#22251 = CYLINDRICAL_SURFACE ( 'NONE', #33878, 3.999999999999976019 ) ;
#22252 = CARTESIAN_POINT ( 'NONE',  ( -445.9999999999999432, -112.9999999999999858, -174.9999999999999716 ) ) ;
#22253 = CARTESIAN_POINT ( 'NONE',  ( -20.00000000000007461, 144.9999999999999716, 187.0000000000000000 ) ) ;
#22254 = AXIS2_PLACEMENT_3D ( 'NONE', #26203, #4137, #25866 ) ;
#22255 = CARTESIAN_POINT ( 'NONE',  ( 21.24400529595485310, -24.65555945140048522, 68.31122994652405112 ) ) ;
#22256 = CIRCLE ( 'NONE', #663, 32.54542015209054284 ) ;
#22257 = EDGE_CURVE ( 'NONE', #29402, #28782, #30695, .T. ) ;
#22258 = EDGE_CURVE ( 'NONE', #20922, #3555, #12366, .T. ) ;
#22259 = VERTEX_POINT ( 'NONE', #20203 ) ;
#22260 = DIRECTION ( 'NONE',  ( 0.1063910735368947813, -0.9943243633099144718, -3.335902418024520312E-15 ) ) ;
#22261 = ORIENTED_EDGE ( 'NONE', *, *, #16948, .T. ) ;
#22262 = EDGE_LOOP ( 'NONE', ( #16395, #29188, #17613, #28904 ) ) ;
#22263 = CARTESIAN_POINT ( 'NONE',  ( -361.0000000000000000, -135.0000000000000000, 113.9999999999999858 ) ) ;
#22264 = CIRCLE ( 'NONE', #3502, 34.41491905851385269 ) ;
#22265 = CARTESIAN_POINT ( 'NONE',  ( 99.30232950514738377, 0.7843626702862538380, 7.468944954497490407 ) ) ;
#22266 = AXIS2_PLACEMENT_3D ( 'NONE', #9208, #33583, #11717 ) ;
#22267 = ORIENTED_EDGE ( 'NONE', *, *, #9714, .T. ) ;
#22268 = VECTOR ( 'NONE', #29827, 1000.000000000000000 ) ;
#22269 = AXIS2_PLACEMENT_3D ( 'NONE', #5989, #19545, #33043 ) ;
#22270 = LINE ( 'NONE', #2691, #10522 ) ;
#22271 = CARTESIAN_POINT ( 'NONE',  ( -106.6601487443931262, -4.849606089681288701, -11.52174238786261107 ) ) ;
#22272 = CONTEXT_DEPENDENT_SHAPE_REPRESENTATION ( #25585, #26644 ) ;
#22274 = DIRECTION ( 'NONE',  ( 0.000000000000000000, 2.465190328815661892E-32, 1.000000000000000000 ) ) ;
#22273 = CYLINDRICAL_SURFACE ( 'NONE', #3645, 1.154999999999999805 ) ;
#22275 = ORIENTED_EDGE ( 'NONE', *, *, #13131, .T. ) ;
#22276 = ORIENTED_EDGE ( 'NONE', *, *, #18078, .T. ) ;
#22277 = CARTESIAN_POINT ( 'NONE',  ( -500.0000000000000000, -137.0000000000000000, 155.0000000000000000 ) ) ;
#22278 = LINE ( 'NONE', #19623, #32343 ) ;
#22279 = CARTESIAN_POINT ( 'NONE',  ( 19.99999999999998934, 144.9999999999999716, 187.0000000000000000 ) ) ;
#22280 = DIRECTION ( 'NONE',  ( 0.000000000000000000, 0.000000000000000000, -1.000000000000000000 ) ) ;
#22281 = ORIENTED_EDGE ( 'NONE', *, *, #29644, .F. ) ;
#22282 = AXIS2_PLACEMENT_3D ( 'NONE', #14009, #8123, #10809 ) ;
#22283 = LINE ( 'NONE', #33314, #16967 ) ;
#22284 = DIRECTION ( 'NONE',  ( 0.000000000000000000, 0.000000000000000000, 1.000000000000000000 ) ) ;
#22285 = CARTESIAN_POINT ( 'NONE',  ( 19.99999999999998934, 75.55999999999990280, 177.7400000000000091 ) ) ;
#22286 = PRODUCT ( 'shaft', 'shaft', '', ( #8201 ) ) ;
#22287 = ORIENTED_EDGE ( 'NONE', *, *, #16945, .F. ) ;
#22288 = CARTESIAN_POINT ( 'NONE',  ( -418.0000000000000000, -105.0000000000000142, 135.9999999999999716 ) ) ;
#22289 = PLANE ( 'NONE',  #22247 ) ;
#22290 = LINE ( 'NONE', #19635, #749 ) ;
#22293 = FACE_OUTER_BOUND ( 'NONE', #10718, .T. ) ;
#22292 = DIRECTION ( 'NONE',  ( 0.000000000000000000, 0.000000000000000000, -1.000000000000000000 ) ) ;
#22291 = VECTOR ( 'NONE', #4579, 1000.000000000000000 ) ;
#22294 = CIRCLE ( 'NONE', #1281, 30.47050528711511674 ) ;
#22295 = AXIS2_PLACEMENT_3D ( 'NONE', #29480, #13290, #16317 ) ;
#22296 = CARTESIAN_POINT ( 'NONE',  ( -418.0000000000000000, 109.0000000000000142, -155.0000000000000000 ) ) ;
#22297 = ORIENTED_EDGE ( 'NONE', *, *, #9526, .F. ) ;
#22299 = AXIS2_PLACEMENT_3D ( 'NONE', #2929, #22821, #25654 ) ;
#22298 = FACE_OUTER_BOUND ( 'NONE', #28180, .T. ) ;
#22300 = DIRECTION ( 'NONE',  ( 0.000000000000000000, 0.000000000000000000, -1.000000000000000000 ) ) ;
#22301 = EDGE_CURVE ( 'NONE', #32774, #7713, #14340, .T. ) ;
#22302 = ADVANCED_FACE ( 'NONE', ( #25162 ), #17372, .T. ) ;
#22303 = ORIENTED_EDGE ( 'NONE', *, *, #34717, .T. ) ;
#22304 = EDGE_CURVE ( 'NONE', #33409, #7560, #791, .T. ) ;
#22305 = ORIENTED_EDGE ( 'NONE', *, *, #16461, .F. ) ;
#22306 = ORIENTED_EDGE ( 'NONE', *, *, #13583, .F. ) ;
#22307 = CARTESIAN_POINT ( 'NONE',  ( -20.63749999999999929, 0.000000000000000000, -11.22499999999999787 ) ) ;
#22308 = ORIENTED_EDGE ( 'NONE', *, *, #14194, .T. ) ;
#22309 = VERTEX_POINT ( 'NONE', #9147 ) ;
#22310 = CARTESIAN_POINT ( 'NONE',  ( -3.250000000000000000, 5.404196845913421754, 0.000000000000000000 ) ) ;
#22311 = CONTEXT_DEPENDENT_SHAPE_REPRESENTATION ( #5556, #14598 ) ;
#22312 = VERTEX_POINT ( 'NONE', #22864 ) ;
#22313 = CARTESIAN_POINT ( 'NONE',  ( 12.00000000000001066, -134.9999999999999716, 162.9999999999999716 ) ) ;
#22314 = AXIS2_PLACEMENT_3D ( 'NONE', #2666, #13535, #24374 ) ;
#22315 = DIRECTION ( 'NONE',  ( 3.697785493223492838E-32, 1.934419779023891545E-16, -1.000000000000000000 ) ) ;
#22316 = ORIENTED_EDGE ( 'NONE', *, *, #4467, .F. ) ;
#22317 = AXIS2_PLACEMENT_3D ( 'NONE', #13416, #13590, #8057 ) ;
#22318 = ORIENTED_EDGE ( 'NONE', *, *, #19936, .T. ) ;
#22319 = LINE ( 'NONE', #960, #29905 ) ;
#22320 = CARTESIAN_POINT ( 'NONE',  ( 2.265105757022230382, -1.320925567293070424, -33.35364885818402314 ) ) ;
#22321 = CARTESIAN_POINT ( 'NONE',  ( 10.17231796313407344, -5.651112684911598016, -77.50000000000000000 ) ) ;
#22322 = CARTESIAN_POINT ( 'NONE',  ( 2.765921099433441999, 4.286445725888479608, -30.79383171238939809 ) ) ;
#22323 = DIRECTION ( 'NONE',  ( 0.000000000000000000, 0.000000000000000000, 1.000000000000000000 ) ) ;
#22324 = ORIENTED_EDGE ( 'NONE', *, *, #7281, .T. ) ;
#22325 = CARTESIAN_POINT ( 'NONE',  ( 1.155000000000000027, 1.414467053015192657E-16, 4.679999999999999716 ) ) ;
#22326 = CARTESIAN_POINT ( 'NONE',  ( 0.7561992252148435067, -2.658747979797246419, -33.81079988514331802 ) ) ;
#22327 = ORIENTED_EDGE ( 'NONE', *, *, #14607, .T. ) ;
#22328 = PLANE ( 'NONE',  #32761 ) ;
#22329 = DIRECTION ( 'NONE',  ( 1.000000000000000000, 0.000000000000000000, 0.000000000000000000 ) ) ;
#22330 = DIRECTION ( 'NONE',  ( 0.000000000000000000, 0.000000000000000000, -1.000000000000000000 ) ) ;
#22331 = CARTESIAN_POINT ( 'NONE',  ( 0.5248942129897558040, 21.86923048072691600, 25.21799932878544581 ) ) ;
#22332 = FACE_OUTER_BOUND ( 'NONE', #25323, .T. ) ;
#22333 = ORIENTED_EDGE ( 'NONE', *, *, #3028, .T. ) ;
#22335 = DIRECTION ( 'NONE',  ( 0.000000000000000000, -1.000000000000000000, 3.421138828918010427E-49 ) ) ;
#22334 = CARTESIAN_POINT ( 'NONE',  ( 2.765921099433441999, 26.03801215795542134, -16.98986790278583570 ) ) ;
#22336 = ADVANCED_FACE ( 'NONE', ( #8980 ), #6286, .T. ) ;
#22337 = AXIS2_PLACEMENT_3D ( 'NONE', #7846, #29568, #2499 ) ;
#22339 = VERTEX_POINT ( 'NONE', #28198 ) ;
#22338 = AXIS2_PLACEMENT_3D ( 'NONE', #18630, #23602, #20933 ) ;
#22340 = CIRCLE ( 'NONE', #17179, 4.000000000000003553 ) ;
#22341 = AXIS2_PLACEMENT_3D ( 'NONE', #11620, #20155, #27975 ) ;
#22342 = CARTESIAN_POINT ( 'NONE',  ( -6.500000000000000000, 0.000000000000000000, 3.930000000000000160 ) ) ;
#22343 = DIRECTION ( 'NONE',  ( -0.6876994588534230957, -0.7259954919231310644, 0.000000000000000000 ) ) ;
#22344 = ADVANCED_FACE ( 'NONE', ( #33709 ), #6469, .T. ) ;
#22345 = ADVANCED_FACE ( 'NONE', ( #22695 ), #6646, .F. ) ;
#22346 = EDGE_LOOP ( 'NONE', ( #15389, #11312, #22198, #22705 ) ) ;
#22347 = EDGE_LOOP ( 'NONE', ( #22442, #14397, #16859, #228 ) ) ;
#22348 = EDGE_CURVE ( 'NONE', #12803, #23775, #17278, .T. ) ;
#22349 = EDGE_CURVE ( 'NONE', #20441, #34661, #9847, .T. ) ;
#22350 = VERTEX_POINT ( 'NONE', #7163 ) ;
#22351 = CARTESIAN_POINT ( 'NONE',  ( 11.99999999999999645, -145.0000000000000000, 159.0000000000000000 ) ) ;
#22352 = CARTESIAN_POINT ( 'NONE',  ( -418.0000000000000000, -105.0000000000000142, -174.9999999999999716 ) ) ;
#22353 = EDGE_LOOP ( 'NONE', ( #27254, #32526, #4636, #28688 ) ) ;
#22354 = ORIENTED_EDGE ( 'NONE', *, *, #25348, .T. ) ;
#22355 = CARTESIAN_POINT ( 'NONE',  ( 8.927936315454028104, -31.29690601358700519, 49.43553178847298568 ) ) ;
#22356 = EDGE_CURVE ( 'NONE', #16360, #25686, #22919, .T. ) ;
#22357 = CARTESIAN_POINT ( 'NONE',  ( 2.789999999999999147, 27.98916443103621177, -15.38717335695007904 ) ) ;
#22358 = CARTESIAN_POINT ( 'NONE',  ( -11.99999999999998224, -134.9999999999999716, 194.9999999999999716 ) ) ;
#22359 = PLANE ( 'NONE',  #22771 ) ;
#22360 = ORIENTED_EDGE ( 'NONE', *, *, #6425, .T. ) ;
#22361 = ORIENTED_EDGE ( 'NONE', *, *, #16645, .T. ) ;
#22362 = LINE ( 'NONE', #30552, #17961 ) ;
#22363 = DIRECTION ( 'NONE',  ( 1.000000000000000000, -0.000000000000000000, 0.000000000000000000 ) ) ;
#22364 = CARTESIAN_POINT ( 'NONE',  ( -442.0000000000000000, 141.0000000000000000, -155.0000000000000000 ) ) ;
#22365 = DIRECTION ( 'NONE',  ( 1.000000000000000000, 0.000000000000000000, 0.000000000000000000 ) ) ;
#22366 = DIRECTION ( 'NONE',  ( -0.000000000000000000, -0.000000000000000000, -1.000000000000000000 ) ) ;
#22367 = AXIS2_PLACEMENT_3D ( 'NONE', #29878, #2639, #15664 ) ;
#22368 = DIRECTION ( 'NONE',  ( -0.000000000000000000, 0.5000000000000012212, 0.8660254037844380415 ) ) ;
#22369 = AXIS2_PLACEMENT_3D ( 'NONE', #18021, #23334, #12323 ) ;
#22370 = CARTESIAN_POINT ( 'NONE',  ( 2.789999999999999147, 7.412728658109134727, -29.75205777216480740 ) ) ;
#22371 = VERTEX_POINT ( 'NONE', #28889 ) ;
#22372 = FACE_OUTER_BOUND ( 'NONE', #25191, .T. ) ;
#22373 = DIRECTION ( 'NONE',  ( -1.000000000000000000, 0.000000000000000000, 0.000000000000000000 ) ) ;
#22374 = CARTESIAN_POINT ( 'NONE',  ( -442.0000000000000000, -105.0000000000000142, 107.9999999999999858 ) ) ;
#22375 = ORIENTED_EDGE ( 'NONE', *, *, #553, .T. ) ;
#22376 = APPLICATION_CONTEXT ( 'automotive_design' ) ;
#22377 = CARTESIAN_POINT ( 'NONE',  ( -143.0000000000000568, 85.49999999999998579, 65.00000000000000000 ) ) ;
#22378 = ORIENTED_EDGE ( 'NONE', *, *, #7733, .F. ) ;
#22379 = DIRECTION ( 'NONE',  ( -1.000000000000000000, -0.000000000000000000, -0.000000000000000000 ) ) ;
#22380 = LINE ( 'NONE', #22564, #29609 ) ;
#22381 = VECTOR ( 'NONE', #16718, 1000.000000000000000 ) ;
#22382 = ORIENTED_EDGE ( 'NONE', *, *, #6661, .F. ) ;
#22383 = LINE ( 'NONE', #31105, #13177 ) ;
#22384 = DIRECTION ( 'NONE',  ( 1.000000000000000000, 0.000000000000000000, 0.000000000000000000 ) ) ;
#22385 = DIRECTION ( 'NONE',  ( 1.000000000000000000, 0.000000000000000000, 0.000000000000000000 ) ) ;
#22386 = ADVANCED_FACE ( 'NONE', ( #18229 ), #10025, .F. ) ;
#22387 = ORIENTED_EDGE ( 'NONE', *, *, #13064, .T. ) ;
#22388 = AXIS2_PLACEMENT_3D ( 'NONE', #23524, #26720, #29574 ) ;
#22389 = AXIS2_PLACEMENT_3D ( 'NONE', #27493, #32471, #29993 ) ;
#22390 = EDGE_CURVE ( 'NONE', #32869, #15141, #2014, .T. ) ;
#22391 = EDGE_CURVE ( 'NONE', #30770, #23261, #4489, .T. ) ;
#22392 = CARTESIAN_POINT ( 'NONE',  ( 829.8297214518297551, 1229.023940416447203, 1753.598338701302964 ) ) ;
#22393 = VECTOR ( 'NONE', #12537, 1000.000000000000000 ) ;
#22394 = FACE_BOUND ( 'NONE', #12910, .T. ) ;
#22395 = ORIENTED_EDGE ( 'NONE', *, *, #31333, .F. ) ;
#22396 = CARTESIAN_POINT ( 'NONE',  ( 0.02407890056655868569, -8.112136323388726922, -30.01377904834218668 ) ) ;
#22397 = CARTESIAN_POINT ( 'NONE',  ( 2.789999999999999591, 12.80000000000000071, 0.000000000000000000 ) ) ;
#22398 = CARTESIAN_POINT ( 'NONE',  ( -499.9999999999999432, 136.9999999999999432, 187.0000000000000000 ) ) ;
#22399 = CARTESIAN_POINT ( 'NONE',  ( 2.789999999999999147, 4.286445725888479608, -30.79383171238939809 ) ) ;
#22400 = ORIENTED_EDGE ( 'NONE', *, *, #10323, .T. ) ;
#22401 = ORIENTED_EDGE ( 'NONE', *, *, #8282, .F. ) ;
#22402 = ORIENTED_EDGE ( 'NONE', *, *, #6784, .T. ) ;
#22403 = DIRECTION ( 'NONE',  ( 0.000000000000000000, 1.836970198721029441E-16, -1.000000000000000000 ) ) ;
#22404 = EDGE_CURVE ( 'NONE', #8601, #28875, #1891, .T. ) ;
#22405 = CARTESIAN_POINT ( 'NONE',  ( 2.765921099433440222, -27.96208973699893008, -13.59246946040217630 ) ) ;
#22406 = AXIS2_PLACEMENT_3D ( 'NONE', #24469, #111, #7576 ) ;
#22407 = DIRECTION ( 'NONE',  ( -0.000000000000000000, -0.000000000000000000, -1.000000000000000000 ) ) ;
#22408 = DIRECTION ( 'NONE',  ( -0.3193015301359803382, -0.9476531711828023452, 0.000000000000000000 ) ) ;
#22409 = VERTEX_POINT ( 'NONE', #18065 ) ;
#22410 = VERTEX_POINT ( 'NONE', #26211 ) ;
#22411 = CARTESIAN_POINT ( 'NONE',  ( -10.00000000000000000, 0.000000000000000000, 0.000000000000000000 ) ) ;
#22412 = ORIENTED_EDGE ( 'NONE', *, *, #4135, .F. ) ;
#22413 = EDGE_CURVE ( 'NONE', #11793, #20827, #7335, .T. ) ;
#22414 = LINE ( 'NONE', #30603, #29992 ) ;
#22415 = PLANE ( 'NONE',  #18291 ) ;
#22416 = ORIENTED_EDGE ( 'NONE', *, *, #27963, .T. ) ;
#22417 = CARTESIAN_POINT ( 'NONE',  ( -12.00000000000001066, 124.9999999999999716, 194.9999999999999716 ) ) ;
#22419 = EDGE_CURVE ( 'NONE', #20279, #25692, #16121, .T. ) ;
#22418 = ORIENTED_EDGE ( 'NONE', *, *, #11913, .F. ) ;
#22420 = DIRECTION ( 'NONE',  ( 0.000000000000000000, 0.000000000000000000, 1.000000000000000000 ) ) ;
#22421 = VECTOR ( 'NONE', #580, 1000.000000000000000 ) ;
#22422 = VECTOR ( 'NONE', #14659, 1000.000000000000000 ) ;
#22423 = DIRECTION ( 'NONE',  ( -0.000000000000000000, -1.000000000000000000, -0.000000000000000000 ) ) ;
#22424 = ORIENTED_EDGE ( 'NONE', *, *, #26085, .T. ) ;
#22425 = CARTESIAN_POINT ( 'NONE',  ( 19.99999999999998934, -137.0000000000000000, -155.0000000000000284 ) ) ;
#22427 = CIRCLE ( 'NONE', #15595, 1.999999999999999556 ) ;
#22426 = CARTESIAN_POINT ( 'NONE',  ( -442.0000000000000000, -112.9999999999999858, -155.0000000000000000 ) ) ;
#22428 = EDGE_CURVE ( 'NONE', #8431, #13630, #1834, .T. ) ;
#22429 = LINE ( 'NONE', #19937, #30907 ) ;
#22430 =( LENGTH_UNIT ( ) NAMED_UNIT ( * ) SI_UNIT ( .MILLI., .METRE. ) );
#22431 = CARTESIAN_POINT ( 'NONE',  ( 1.039999999999999369, -1.891117961020236216, 34.36292081097831641 ) ) ;
#22432 = LINE ( 'NONE', #22253, #21877 ) ;
#22433 = LINE ( 'NONE', #6037, #16101 ) ;
#22434 = VERTEX_POINT ( 'NONE', #15549 ) ;
#22435 = AXIS2_PLACEMENT_3D ( 'NONE', #12553, #11865, #33732 ) ;
#22436 = ORIENTED_EDGE ( 'NONE', *, *, #17400, .F. ) ;
#22437 = EDGE_CURVE ( 'NONE', #32336, #2950, #27459, .T. ) ;
#22438 = DIRECTION ( 'NONE',  ( 0.1063910735368947813, -0.9943243633099144718, -3.335902418024520312E-15 ) ) ;
#22439 = EDGE_LOOP ( 'NONE', ( #19826, #32800, #27753, #18336 ) ) ;
#22440 = VECTOR ( 'NONE', #12093, 1000.000000000000000 ) ;
#22441 = VERTEX_POINT ( 'NONE', #12890 ) ;
#22442 = ORIENTED_EDGE ( 'NONE', *, *, #15476, .F. ) ;
#22443 = CARTESIAN_POINT ( 'NONE',  ( 1.749999999999999778, 14.40815186467775888, 31.25366880301323746 ) ) ;
#22444 = AXIS2_PLACEMENT_3D ( 'NONE', #5023, #15920, #5191 ) ;
#22445 = CARTESIAN_POINT ( 'NONE',  ( 99.58837370945708756, 1.917593826231215770, 7.253178031220425481 ) ) ;
#22446 = APPLICATION_PROTOCOL_DEFINITION ( 'draft international standard', 'automotive_design', 1998, #27351 ) ;
#22447 = VECTOR ( 'NONE', #25792, 1000.000000000000000 ) ;
#22448 = ORIENTED_EDGE ( 'NONE', *, *, #11309, .F. ) ;
#22449 = DIRECTION ( 'NONE',  ( 0.000000000000000000, -1.000000000000000000, 1.131431318426415506E-52 ) ) ;
#22450 = ITEM_DEFINED_TRANSFORMATION ( 'NONE', 'NONE', #2483,  #28566 ) ;
#22452 = DIRECTION ( 'NONE',  ( 0.000000000000000000, 0.000000000000000000, -1.000000000000000000 ) ) ;
#22451 = DIRECTION ( 'NONE',  ( 0.000000000000000000, 0.000000000000000000, 1.000000000000000000 ) ) ;
#22453 = VERTEX_POINT ( 'NONE', #23729 ) ;
#22454 = ORIENTED_EDGE ( 'NONE', *, *, #24124, .F. ) ;
#22455 = DIRECTION ( 'NONE',  ( -0.000000000000000000, -0.000000000000000000, -1.000000000000000000 ) ) ;
#22456 = DIRECTION ( 'NONE',  ( 0.000000000000000000, 0.000000000000000000, 1.000000000000000000 ) ) ;
#22457 = DIRECTION ( 'NONE',  ( 0.000000000000000000, 0.000000000000000000, 1.000000000000000000 ) ) ;
#22458 = CARTESIAN_POINT ( 'NONE',  ( -5.210000000000000853, 0.000000000000000000, 0.000000000000000000 ) ) ;
#22459 = ORIENTED_EDGE ( 'NONE', *, *, #16696, .F. ) ;
#22460 = ADVANCED_FACE ( 'NONE', ( #6994 ), #34587, .F. ) ;
#22461 = CARTESIAN_POINT ( 'NONE',  ( -12.00000000000003908, -134.9999999999999716, -154.9999999999999716 ) ) ;
#22462 = CARTESIAN_POINT ( 'NONE',  ( -355.0000000000000000, -119.0000000000000000, 128.0000000000000000 ) ) ;
#22463 = ADVANCED_FACE ( 'NONE', ( #10201 ), #2353, .F. ) ;
#22464 = AXIS2_PLACEMENT_3D ( 'NONE', #8384, #24395, #27777 ) ;
#22465 = DIRECTION ( 'NONE',  ( 0.000000000000000000, 1.000000000000000000, 1.836970198721029688E-16 ) ) ;
#22466 = EDGE_LOOP ( 'NONE', ( #21484, #13592, #25296, #17755 ) ) ;
#22467 = CIRCLE ( 'NONE', #19631, 2.000000000000001776 ) ;
#22468 = DIRECTION ( 'NONE',  ( 0.000000000000000000, 1.000000000000000000, 2.465190328815662439E-32 ) ) ;
#22469 = PLANE ( 'NONE',  #6879 ) ;
#22470 = FACE_OUTER_BOUND ( 'NONE', #31923, .T. ) ;
#22471 = CYLINDRICAL_SURFACE ( 'NONE', #33750, 2.525000000000000799 ) ;
#22473 = CARTESIAN_POINT ( 'NONE',  ( 0.8418677244547475569, 6.533629441836217744, 13.49999999999999645 ) ) ;
#22472 = CARTESIAN_POINT ( 'NONE',  ( 2.630124765083918348, -1.866624223957557893, -0.7500000000000000000 ) ) ;
#22474 = TOROIDAL_SURFACE ( 'NONE', #19081, 30.47050528711512030, 8.000000000000000000 ) ;
#22475 = UNCERTAINTY_MEASURE_WITH_UNIT (LENGTH_MEASURE( 1.000000000000000082E-05 ), #21468, 'distance_accuracy_value', 'NONE');
#22477 = ADVANCED_FACE ( 'NONE', ( #34946 ), #21231, .T. ) ;
#22476 = CYLINDRICAL_SURFACE ( 'NONE', #24656, 3.999999999999976019 ) ;
#22478 = ORIENTED_EDGE ( 'NONE', *, *, #32337, .T. ) ;
#22479 = DIRECTION ( 'NONE',  ( 1.000000000000000000, 3.469446951953834515E-18, 0.000000000000000000 ) ) ;
#22480 = CARTESIAN_POINT ( 'NONE',  ( 0.000000000000000000, -20.92506858792774338, 22.14933852381670221 ) ) ;
#22481 = MANIFOLD_SOLID_BREP ( 'Cut-Extrude1', #11099 ) ;
#22482 = CLOSED_SHELL ( 'NONE', ( #5129, #14540, #21607, #9372, #13104, #21336, #31692, #21949, #6615, #17672, #14323, #27357, #12110, #10223, #25579, #4543, #22667, #31696 ) ) ;
#22483 = VERTEX_POINT ( 'NONE', #10906 ) ;
#22484 = ORIENTED_EDGE ( 'NONE', *, *, #11004, .T. ) ;
#22485 = VECTOR ( 'NONE', #13476, 1000.000000000000000 ) ;
#22486 = ORIENTED_EDGE ( 'NONE', *, *, #2636, .T. ) ;
#22487 = DIRECTION ( 'NONE',  ( 1.000000000000000000, 0.000000000000000000, 0.000000000000000000 ) ) ;
#22488 = ORIENTED_EDGE ( 'NONE', *, *, #26308, .T. ) ;
#22489 = ORIENTED_EDGE ( 'NONE', *, *, #34180, .F. ) ;
#22490 = EDGE_CURVE ( 'NONE', #27476, #19038, #20536, .T. ) ;
#22491 = LINE ( 'NONE', #8773, #25266 ) ;
#22492 = VECTOR ( 'NONE', #10558, 1000.000000000000000 ) ;
#22493 = EDGE_LOOP ( 'NONE', ( #2657, #3174, #25129, #4969 ) ) ;
#22494 = LINE ( 'NONE', #33871, #34556 ) ;
#22495 = CARTESIAN_POINT ( 'NONE',  ( 15.99999999999998579, -137.0000000000000000, 155.0000000000000000 ) ) ;
#22496 = ORIENTED_EDGE ( 'NONE', *, *, #7135, .F. ) ;
#22497 = VERTEX_POINT ( 'NONE', #26916 ) ;
#22498 = LINE ( 'NONE', #30319, #21947 ) ;
#22499 = DIRECTION ( 'NONE',  ( 0.000000000000000000, -2.748076793626624385E-15, -1.000000000000000000 ) ) ;
#22500 = VECTOR ( 'NONE', #25478, 1000.000000000000000 ) ;
#22501 = EDGE_CURVE ( 'NONE', #6306, #16209, #18926, .T. ) ;
#22502 = CARTESIAN_POINT ( 'NONE',  ( -20.00000000000007461, 136.9999999999999432, -162.9999999999999716 ) ) ;
#22503 = CARTESIAN_POINT ( 'NONE',  ( 24.90835164106607635, -28.52396285516520891, 49.43553178847298568 ) ) ;
#22504 = FACE_BOUND ( 'NONE', #19046, .T. ) ;
#22505 = ORIENTED_EDGE ( 'NONE', *, *, #17193, .F. ) ;
#22506 = EDGE_CURVE ( 'NONE', #23786, #33325, #19109, .T. ) ;
#22507 = CYLINDRICAL_SURFACE ( 'NONE', #4857, 2.524999999999999467 ) ;
#22508 = EDGE_CURVE ( 'NONE', #33799, #8677, #21752, .T. ) ;
#22509 = CARTESIAN_POINT ( 'NONE',  ( -355.0000000000000000, 118.9999999999999716, 130.0000000000000000 ) ) ;
#22510 = ORIENTED_EDGE ( 'NONE', *, *, #28807, .F. ) ;
#22511 = B_SPLINE_CURVE_WITH_KNOTS ( 'NONE', 3,
 ( #11665, #22515, #31220, #617 ),
 .UNSPECIFIED., .F., .F.,
 ( 4, 4 ),
 ( 0.005298352064454709028, 0.005985220659832061682 ),
 .UNSPECIFIED. ) ;
#22512 = LINE ( 'NONE', #27661, #31085 ) ;
#22513 = DIRECTION ( 'NONE',  ( 0.000000000000000000, 0.000000000000000000, 1.000000000000000000 ) ) ;
#22514 = DIRECTION ( 'NONE',  ( -0.1081190184239417262, -0.9941379571543595972, 0.000000000000000000 ) ) ;
#22515 = CARTESIAN_POINT ( 'NONE',  ( -5.475207829904333729E-16, -23.48484457444932261, -19.71282888652513066 ) ) ;
#22516 = DIRECTION ( 'NONE',  ( 0.4684084406997896521, 0.8835120444460232703, 1.622985295858434769E-16 ) ) ;
#22517 = AXIS2_PLACEMENT_3D ( 'NONE', #25505, #28876, #15190 ) ;
#22518 = CYLINDRICAL_SURFACE ( 'NONE', #17285, 16.19999999999999574 ) ;
#22519 = ORIENTED_EDGE ( 'NONE', *, *, #5338, .F. ) ;
#22520 = B_SPLINE_CURVE_WITH_KNOTS ( 'NONE', 3,
 ( #20539, #9850, #18405, #4661, #31898, #4148, #20885, #7516, #1837, #20717, #2017, #31563, #15553, #34765, #26396, #15039, #23554, #31393, #12717, #28723, #12893, #6997, #4322, #15209, #26052, #2712, #5717, #24776, #16619, #29428, #3061, #7881, #5544, #24416, #32784, #24245 ),
 .UNSPECIFIED., .F., .F.,
 ( 4, 2, 2, 2, 2, 2, 2, 2, 2, 2, 2, 2, 2, 2, 2, 2, 2, 4 ),
 ( 3.708067775211463633E-19, 0.001035696236907465012, 0.002071392473814929591, 0.003107088710722395036, 0.004142784947629859181, 0.005178481184537325061, 0.006214177421444790073, 0.007249873658352254217, 0.007767721776805967641, 0.008285569895259680198, 0.009321266132167145210, 0.01035696236907461369, 0.01087481048752832885, 0.01139265860598204401, 0.01242835484288950555, 0.01449974731670440609, 0.01553544355361185722, 0.01657113979051930489 ),
 .UNSPECIFIED. ) ;
#22521 = CARTESIAN_POINT ( 'NONE',  ( -410.0000000000000568, 113.0000000000000000, 154.9999999999999716 ) ) ;
#22523 = CARTESIAN_POINT ( 'NONE',  ( 22.50000000000000355, 2.755455298081545172E-15, 0.000000000000000000 ) ) ;
#22522 = CARTESIAN_POINT ( 'NONE',  ( -15.99999999999998579, 4.559999999999909015, -168.2400000000000091 ) ) ;
#22524 = AXIS2_PLACEMENT_3D ( 'NONE', #1097, #20969, #17318 ) ;
#22525 = ORIENTED_EDGE ( 'NONE', *, *, #20927, .F. ) ;
#22526 = DIRECTION ( 'NONE',  ( 0.000000000000000000, 0.000000000000000000, 1.000000000000000000 ) ) ;
#22527 = DIRECTION ( 'NONE',  ( 0.000000000000000000, -0.000000000000000000, -1.000000000000000000 ) ) ;
#22528 = VECTOR ( 'NONE', #13025, 1000.000000000000000 ) ;
#22529 = ORIENTED_EDGE ( 'NONE', *, *, #29437, .F. ) ;
#22530 = AXIS2_PLACEMENT_3D ( 'NONE', #7359, #18606, #5045 ) ;
#22531 = EDGE_LOOP ( 'NONE', ( #3700, #2736, #11388, #17389 ) ) ;
#22532 = LINE ( 'NONE', #28572, #17388 ) ;
#22533 = ORIENTED_EDGE ( 'NONE', *, *, #25455, .F. ) ;
#22534 = ORIENTED_EDGE ( 'NONE', *, *, #26350, .T. ) ;
#22535 = MANIFOLD_SOLID_BREP ( 'Boss-Extrude6[1]', #33827 ) ;
#22536 = CARTESIAN_POINT ( 'NONE',  ( 32.40067729534749219, 3.066020821660475626, 49.43553178847298568 ) ) ;
#22537 = PRODUCT_DEFINITION_SHAPE ( 'NONE', 'NONE',  #35166 ) ;
#22538 = DIRECTION ( 'NONE',  ( -0.000000000000000000, 1.000000000000000000, -0.000000000000000000 ) ) ;
#22539 = CARTESIAN_POINT ( 'NONE',  ( -449.9999999999999432, -112.9999999999999858, -155.0000000000000000 ) ) ;
#22540 = LINE ( 'NONE', #11689, #14826 ) ;
#22541 = ORIENTED_EDGE ( 'NONE', *, *, #28121, .F. ) ;
#22542 = ORIENTED_EDGE ( 'NONE', *, *, #4331, .F. ) ;
#22543 = EDGE_CURVE ( 'NONE', #26161, #18440, #30321, .T. ) ;
#22544 = CARTESIAN_POINT ( 'NONE',  ( 0.07094833146048340478, -31.01658195443398824, 6.517894193012690351 ) ) ;
#22545 = CARTESIAN_POINT ( 'NONE',  ( -499.9999999999999432, -113.0000000000000000, -194.9999999999999716 ) ) ;
#22546 = DIRECTION ( 'NONE',  ( 0.8835120444460229372, 0.4684084406997900407, 0.000000000000000000 ) ) ;
#22547 = CIRCLE ( 'NONE', #28235, 4.000000000000003553 ) ;
#22548 = EDGE_CURVE ( 'NONE', #1095, #28119, #13931, .T. ) ;
#22549 = DIRECTION ( 'NONE',  ( -1.000000000000000000, 0.000000000000000000, 1.232595164407831220E-32 ) ) ;
#22550 = FACE_OUTER_BOUND ( 'NONE', #6408, .T. ) ;
#22551 = DIRECTION ( 'NONE',  ( -1.000000000000000000, 0.000000000000000000, 0.000000000000000000 ) ) ;
#22552 = ADVANCED_FACE ( 'NONE', ( #3236 ), #14110, .T. ) ;
#22553 = DIRECTION ( 'NONE',  ( 0.000000000000000000, 0.000000000000000000, 1.000000000000000000 ) ) ;
#22554 = ORIENTED_EDGE ( 'NONE', *, *, #29865, .F. ) ;
#22555 = ADVANCED_FACE ( 'NONE', ( #32259 ), #7877, .F. ) ;
#22556 = VECTOR ( 'NONE', #21240, 1000.000000000000000 ) ;
#22557 = PLANE ( 'NONE',  #2607 ) ;
#22558 = CARTESIAN_POINT ( 'NONE',  ( 0.02407890056655738464, 28.29688452313417812, -12.88099432405573630 ) ) ;
#22559 = CARTESIAN_POINT ( 'NONE',  ( 11.99999999999999645, 144.9999999999999716, -162.9999999999999432 ) ) ;
#22560 = ORIENTED_EDGE ( 'NONE', *, *, #8059, .T. ) ;
#22561 = CARTESIAN_POINT ( 'NONE',  ( -500.0000000000000000, -104.9999999999999858, -194.9999999999999716 ) ) ;
#22562 = VERTEX_POINT ( 'NONE', #1276 ) ;
#22563 = SURFACE_STYLE_FILL_AREA ( #11710 ) ;
#22564 = CARTESIAN_POINT ( 'NONE',  ( 19.99999999999998934, 144.9999999999999716, -186.9999999999999432 ) ) ;
#22565 = CIRCLE ( 'NONE', #26534, 4.000000000000003553 ) ;
#22566 = EDGE_CURVE ( 'NONE', #21537, #30882, #6322, .T. ) ;
#22567 = EDGE_CURVE ( 'NONE', #13666, #6283, #26222, .T. ) ;
#22568 = AXIS2_PLACEMENT_3D ( 'NONE', #28282, #12276, #27920 ) ;
#22569 = ORIENTED_EDGE ( 'NONE', *, *, #6299, .T. ) ;
#22570 = LINE ( 'NONE', #8673, #23950 ) ;
#22571 = CARTESIAN_POINT ( 'NONE',  ( -31.87924797510909869, -6.551177101682105430, -36.68877005347593467 ) ) ;
#22572 = DIRECTION ( 'NONE',  ( 0.000000000000000000, -1.000000000000000000, -1.224646799147353207E-16 ) ) ;
#22573 = EDGE_LOOP ( 'NONE', ( #27315, #18050, #24329, #32987 ) ) ;
#22574 = DIRECTION ( 'NONE',  ( 0.1063910735369155841, -0.9943243633099125844, -3.335902418025060287E-15 ) ) ;
#22575 = DIRECTION ( 'NONE',  ( -0.000000000000000000, 1.836970198721029934E-16, -1.000000000000000000 ) ) ;
#22576 = VERTEX_POINT ( 'NONE', #27795 ) ;
#22577 = DIRECTION ( 'NONE',  ( -2.891205793294675368E-16, 0.000000000000000000, -1.000000000000000000 ) ) ;
#22578 = DIRECTION ( 'NONE',  ( -1.000000000000000000, -0.000000000000000000, -0.000000000000000000 ) ) ;
#22579 = DIRECTION ( 'NONE',  ( 0.000000000000000000, 0.000000000000000000, -1.000000000000000000 ) ) ;
#22580 = CARTESIAN_POINT ( 'NONE',  ( -35.00000000000000000, 3.432458613951602011, 68.31122994652405112 ) ) ;
#22581 = VERTEX_POINT ( 'NONE', #14990 ) ;
#22582 = ORIENTED_EDGE ( 'NONE', *, *, #19546, .F. ) ;
#22583 = ORIENTED_EDGE ( 'NONE', *, *, #14193, .F. ) ;
#22584 = LINE ( 'NONE', #24883, #29472 ) ;
#22585 =( GEOMETRIC_REPRESENTATION_CONTEXT ( 3 ) GLOBAL_UNCERTAINTY_ASSIGNED_CONTEXT ( ( #8940 ) ) GLOBAL_UNIT_ASSIGNED_CONTEXT ( ( #8886, #709, #19931 ) ) REPRESENTATION_CONTEXT ( 'NONE', 'WORKASPACE' ) );
#22586 = CARTESIAN_POINT ( 'NONE',  ( 1.749999999999999778, 34.10861917999622506, -4.581348211831717698 ) ) ;
#22587 = AXIS2_PLACEMENT_3D ( 'NONE', #1316, #26206, #20875 ) ;
#22588 = CIRCLE ( 'NONE', #7218, 7.999999999999979572 ) ;
#22589 = DIRECTION ( 'NONE',  ( 0.000000000000000000, -0.000000000000000000, 1.000000000000000000 ) ) ;
#22590 = DIRECTION ( 'NONE',  ( 0.000000000000000000, 1.310824597558155437E-49, 1.000000000000000000 ) ) ;
#22591 = ORIENTED_EDGE ( 'NONE', *, *, #5243, .T. ) ;
#22592 = ORIENTED_EDGE ( 'NONE', *, *, #31930, .T. ) ;
#22593 = DIRECTION ( 'NONE',  ( 0.000000000000000000, -1.000000000000000000, -2.465190328815662439E-32 ) ) ;
#22594 = VERTEX_POINT ( 'NONE', #22991 ) ;
#22595 = EDGE_CURVE ( 'NONE', #6108, #10763, #4095, .T. ) ;
#22596 = DIRECTION ( 'NONE',  ( 0.000000000000000000, -1.000000000000000000, 6.123233995736766036E-17 ) ) ;
#22597 = EDGE_CURVE ( 'NONE', #23843, #10663, #25300, .T. ) ;
#22598 = CARTESIAN_POINT ( 'NONE',  ( 0.7564103381736747567, 31.72524275137206828, -11.99054900124176193 ) ) ;
#22599 = VERTEX_POINT ( 'NONE', #17322 ) ;
#22600 = CIRCLE ( 'NONE', #18067, 30.47050528711512030 ) ;
#22601 = EDGE_LOOP ( 'NONE', ( #5445, #22037 ) ) ;
#22602 = DIRECTION ( 'NONE',  ( -0.000000000000000000, -0.000000000000000000, -1.000000000000000000 ) ) ;
#22603 = ADVANCED_FACE ( 'NONE', ( #33847 ), #6424, .T. ) ;
#22604 = ADVANCED_FACE ( 'NONE', ( #3407 ), #22289, .T. ) ;
#22605 = LINE ( 'NONE', #5670, #21193 ) ;
#22606 = ORIENTED_EDGE ( 'NONE', *, *, #12230, .F. ) ;
#22607 = DIRECTION ( 'NONE',  ( -0.000000000000000000, -0.000000000000000000, -1.000000000000000000 ) ) ;
#22608 = FACE_OUTER_BOUND ( 'NONE', #23366, .T. ) ;
#22609 = LINE ( 'NONE', #25257, #18973 ) ;
#22610 = LINE ( 'NONE', #9722, #3761 ) ;
#22611 = CIRCLE ( 'NONE', #14071, 4.000000000000003553 ) ;
#22612 = CARTESIAN_POINT ( 'NONE',  ( -109.5827309310070916, -2.278159677709880704, 12.29156386665007084 ) ) ;
#22613 = PLANE ( 'NONE',  #6527 ) ;
#22614 = FACE_BOUND ( 'NONE', #32458, .T. ) ;
#22616 = ADVANCED_FACE ( 'NONE', ( #6777 ), #19807, .T. ) ;
#22615 = VERTEX_POINT ( 'NONE', #33135 ) ;
#22617 = VECTOR ( 'NONE', #13927, 1000.000000000000000 ) ;
#22618 = VECTOR ( 'NONE', #1237, 1000.000000000000000 ) ;
#22619 = ORIENTED_EDGE ( 'NONE', *, *, #382, .T. ) ;
#22620 = DIRECTION ( 'NONE',  ( 0.08782252338093358979, -0.9961361374767030430, -3.823500829060100389E-15 ) ) ;
#22621 = VERTEX_POINT ( 'NONE', #19633 ) ;
#22622 = VERTEX_POINT ( 'NONE', #9469 ) ;
#22623 = CIRCLE ( 'NONE', #24885, 2.525000000000000799 ) ;
#22624 = DIRECTION ( 'NONE',  ( -1.000000000000000000, -0.000000000000000000, -0.000000000000000000 ) ) ;
#22625 = EDGE_CURVE ( 'NONE', #9821, #1704, #6602, .T. ) ;
#22626 = EDGE_CURVE ( 'NONE', #7363, #22339, #20325, .T. ) ;
#22627 = CYLINDRICAL_SURFACE ( 'NONE', #9675, 16.19999999999999929 ) ;
#22628 = EDGE_LOOP ( 'NONE', ( #16192, #16188, #18731, #29928 ) ) ;
#22629 = DIRECTION ( 'NONE',  ( -1.000000000000000000, 0.000000000000000000, 0.000000000000000000 ) ) ;
#22630 = CARTESIAN_POINT ( 'NONE',  ( -102.7235731336728719, -4.592708079286355272, -11.62653478258734907 ) ) ;
#22632 = CARTESIAN_POINT ( 'NONE',  ( 17.27856612038527118, 33.69708579775584667, 49.43553178847298568 ) ) ;
#22631 = DIRECTION ( 'NONE',  ( -0.000000000000000000, 1.000000000000000000, -0.000000000000000000 ) ) ;
#22633 = VECTOR ( 'NONE', #16998, 1000.000000000000000 ) ;
#22634 = ORIENTED_EDGE ( 'NONE', *, *, #14142, .F. ) ;
#22635 = ORIENTED_EDGE ( 'NONE', *, *, #12162, .F. ) ;
#22636 = LINE ( 'NONE', #19962, #4323 ) ;
#22637 = LINE ( 'NONE', #1440, #14717 ) ;
#22638 = CARTESIAN_POINT ( 'NONE',  ( -12.00000000000001066, -56.99999999999997868, -154.9999999999999716 ) ) ;
#22639 = DIRECTION ( 'NONE',  ( 1.000000000000000000, 0.000000000000000000, 0.000000000000000000 ) ) ;
#22640 = ORIENTED_EDGE ( 'NONE', *, *, #16096, .F. ) ;
#22641 = VECTOR ( 'NONE', #1444, 1000.000000000000114 ) ;
#22643 = CARTESIAN_POINT ( 'NONE',  ( 2.789999999999999147, 13.51972826729850041, -27.27250221666277596 ) ) ;
#22642 = CIRCLE ( 'NONE', #26613, 3.999999999999976019 ) ;
#22644 = DIRECTION ( 'NONE',  ( -0.000000000000000000, -1.000000000000000000, -0.000000000000000000 ) ) ;
#22645 = ADVANCED_FACE ( 'NONE', ( #17142 ), #31001, .T. ) ;
#22646 = EDGE_CURVE ( 'NONE', #33401, #3348, #31332, .T. ) ;
#22647 =( REPRESENTATION_RELATIONSHIP ('NONE','NONE', #23037, #28231 ) REPRESENTATION_RELATIONSHIP_WITH_TRANSFORMATION ( #13732 )SHAPE_REPRESENTATION_RELATIONSHIP( ) );
#22648 = VERTEX_POINT ( 'NONE', #19974 ) ;
#22649 = LINE ( 'NONE', #28153, #19195 ) ;
#22650 = CARTESIAN_POINT ( 'NONE',  ( 0.000000000000000000, -33.69708579775584667, 49.43553178847298568 ) ) ;
#22651 = ADVANCED_FACE ( 'NONE', ( #6069 ), #14291, .F. ) ;
#22652 = PLANE ( 'NONE',  #16132 ) ;
#22653 = AXIS2_PLACEMENT_3D ( 'NONE', #29584, #32416, #8036 ) ;
#22655 = CARTESIAN_POINT ( 'NONE',  ( 32.30227131129396412, -3.970848902647437395, 68.31122994652405112 ) ) ;
#22654 = DIRECTION ( 'NONE',  ( 0.000000000000000000, 0.000000000000000000, 1.000000000000000000 ) ) ;
#22656 = DIRECTION ( 'NONE',  ( -1.000000000000000000, 0.000000000000000000, 0.000000000000000000 ) ) ;
#22657 = CYLINDRICAL_SURFACE ( 'NONE', #21066, 2.525000000000001243 ) ;
#22658 = ORIENTED_EDGE ( 'NONE', *, *, #19424, .F. ) ;
#22659 = CARTESIAN_POINT ( 'NONE',  ( 9.199999999999999289, -15.58845726811992449, 0.000000000000000000 ) ) ;
#22660 = CARTESIAN_POINT ( 'NONE',  ( 0.02407890056655695096, 11.80989368511462523, 28.76039115933989976 ) ) ;
#22661 = AXIS2_PLACEMENT_3D ( 'NONE', #19400, #21705, #21881 ) ;
#22662 = ORIENTED_EDGE ( 'NONE', *, *, #21530, .F. ) ;
#22663 = SHAPE_REPRESENTATION_RELATIONSHIP ( 'NONE' , 'NONE' ,  #19821, #33925 ) ;
#22664 = ORIENTED_EDGE ( 'NONE', *, *, #20612, .F. ) ;
#22665 = ADVANCED_FACE ( 'NONE', ( #11619, #30825 ), #22469, .F. ) ;
#22666 = CIRCLE ( 'NONE', #28351, 2.525000000000001243 ) ;
#22667 = ADVANCED_FACE ( 'NONE', ( #17502, #3927 ), #4977, .T. ) ;
#22668 = ORIENTED_EDGE ( 'NONE', *, *, #11761, .F. ) ;
#22669 = CARTESIAN_POINT ( 'NONE',  ( 11.99999999999999645, -105.0000000000000142, 174.9999999999999432 ) ) ;
#22670 = EDGE_LOOP ( 'NONE', ( #18807, #20504, #34811, #33675 ) ) ;
#22671 = VERTEX_POINT ( 'NONE', #26525 ) ;
#22672 = CARTESIAN_POINT ( 'NONE',  ( -430.0000000000000000, 134.9999999999999716, 113.9999999999999858 ) ) ;
#22673 = EDGE_CURVE ( 'NONE', #10814, #24787, #34774, .T. ) ;
#22674 = AXIS2_PLACEMENT_3D ( 'NONE', #12056, #19887, #1181 ) ;
#22675 = ITEM_DEFINED_TRANSFORMATION ( 'NONE', 'NONE', #28053,  #28566 ) ;
#22676 = EDGE_CURVE ( 'NONE', #18132, #22985, #15164, .T. ) ;
#22677 = VERTEX_POINT ( 'NONE', #15506 ) ;
#22678 = FACE_OUTER_BOUND ( 'NONE', #6309, .T. ) ;
#22679 = CARTESIAN_POINT ( 'NONE',  ( -32.37866696771086339, 3.290334066652079947, 68.31122994652405112 ) ) ;
#22680 = ORIENTED_EDGE ( 'NONE', *, *, #31750, .F. ) ;
#22681 = VERTEX_POINT ( 'NONE', #25824 ) ;
#22682 = CARTESIAN_POINT ( 'NONE',  ( 5.021133111224679091, 28.08988295778447508, -67.50000000000000000 ) ) ;
#22683 = ADVANCED_FACE ( 'NONE', ( #23685 ), #28846, .T. ) ;
#22684 = LINE ( 'NONE', #19484, #21500 ) ;
#22685 = DIRECTION ( 'NONE',  ( 1.000000000000000000, 0.000000000000000000, 0.000000000000000000 ) ) ;
#22686 = LINE ( 'NONE', #5453, #10834 ) ;
#22687 = CARTESIAN_POINT ( 'NONE',  ( 2.783128806874977990, 29.25797949657086860, 9.843693408253784582 ) ) ;
#22688 = ORIENTED_EDGE ( 'NONE', *, *, #34026, .F. ) ;
#22689 = DIRECTION ( 'NONE',  ( 0.000000000000000000, -1.000000000000000000, -3.083952846180992253E-16 ) ) ;
#22690 = VECTOR ( 'NONE', #30726, 1000.000000000000000 ) ;
#22691 = PLANE ( 'NONE',  #32356 ) ;
#22692 = ORIENTED_EDGE ( 'NONE', *, *, #21057, .T. ) ;
#22693 = CARTESIAN_POINT ( 'NONE',  ( 0.000000000000000000, 3.909681563762119172, -30.21863799912381054 ) ) ;
#22694 = CARTESIAN_POINT ( 'NONE',  ( -5.469264258321805627, 1.713938105891546382, 3.930000000000000160 ) ) ;
#22695 = FACE_OUTER_BOUND ( 'NONE', #16420, .T. ) ;
#22696 = DIRECTION ( 'NONE',  ( 0.000000000000000000, 0.000000000000000000, 1.000000000000000000 ) ) ;
#22697 = DIRECTION ( 'NONE',  ( -1.000000000000000000, -0.000000000000000000, -0.000000000000000000 ) ) ;
#22698 = VECTOR ( 'NONE', #20398, 1000.000000000000000 ) ;
#22699 = DIRECTION ( 'NONE',  ( -1.000000000000000000, 0.000000000000000000, 0.000000000000000000 ) ) ;
#22700 = ORIENTED_EDGE ( 'NONE', *, *, #22349, .F. ) ;
#22701 = CARTESIAN_POINT ( 'NONE',  ( -143.0000000000000568, -89.01471862576147487, 43.40376782973931569 ) ) ;
#22703 = DIRECTION ( 'NONE',  ( 0.000000000000000000, 0.000000000000000000, -1.000000000000000000 ) ) ;
#22702 = CARTESIAN_POINT ( 'NONE',  ( 2.789999999999999147, -0.09145294252654824485, -30.47036804522408460 ) ) ;
#22704 = VECTOR ( 'NONE', #1535, 1000.000000000000000 ) ;
#22705 = ORIENTED_EDGE ( 'NONE', *, *, #29800, .T. ) ;
#22706 = FACE_OUTER_BOUND ( 'NONE', #8903, .T. ) ;
#22707 = EDGE_CURVE ( 'NONE', #28991, #20852, #3483, .T. ) ;
#22708 = VERTEX_POINT ( 'NONE', #13021 ) ;
#22709 = VERTEX_POINT ( 'NONE', #29016 ) ;
#22710 = ADVANCED_FACE ( 'NONE', ( #7294 ), #18361, .F. ) ;
#22711 = EDGE_CURVE ( 'NONE', #24869, #20130, #33025, .T. ) ;
#22712 = CIRCLE ( 'NONE', #10760, 3.999999999999976019 ) ;
#22713 = EDGE_LOOP ( 'NONE', ( #25291, #10921, #16848, #17658, #343, #2829 ) ) ;
#22714 = DIRECTION ( 'NONE',  ( 0.000000000000000000, -1.224646799147353207E-16, 1.000000000000000000 ) ) ;
#22715 = ORIENTED_EDGE ( 'NONE', *, *, #11091, .F. ) ;
#22716 = ORIENTED_EDGE ( 'NONE', *, *, #29545, .F. ) ;
#22717 = MANIFOLD_SOLID_BREP ( 'Square tube 40 X 40 X 4(1)[11]', #2012 ) ;
#22718 = LINE ( 'NONE', #33554, #17603 ) ;
#22719 = PRESENTATION_LAYER_ASSIGNMENT (  '', '', ( #28951 ) ) ;
#22720 = DIRECTION ( 'NONE',  ( -1.000000000000000000, 0.000000000000000000, 1.232595164407831220E-32 ) ) ;
#22721 = CARTESIAN_POINT ( 'NONE',  ( -499.9999999999999432, -137.0000000000000000, -194.9999999999999716 ) ) ;
#22722 = EDGE_LOOP ( 'NONE', ( #22560, #5276, #13874, #29498 ) ) ;
#22723 = ORIENTED_EDGE ( 'NONE', *, *, #29160, .F. ) ;
#22724 = DIRECTION ( 'NONE',  ( -0.000000000000000000, -0.000000000000000000, -1.000000000000000000 ) ) ;
#22725 = CYLINDRICAL_SURFACE ( 'NONE', #2141, 34.41491905851385269 ) ;
#22726 = CARTESIAN_POINT ( 'NONE',  ( -365.0000000000000000, 124.9999999999999432, 181.0000000000000000 ) ) ;
#22727 = CARTESIAN_POINT ( 'NONE',  ( 129.3530333899765594, -6.000000000000000000, -62.49999999999999289 ) ) ;
#22728 = CARTESIAN_POINT ( 'NONE',  ( -6.500000000000000000, 0.000000000000000000, -0.7500000000000000000 ) ) ;
#22729 = CIRCLE ( 'NONE', #21597, 5.115020388170798959 ) ;
#22730 = FACE_OUTER_BOUND ( 'NONE', #21397, .T. ) ;
#22731 = CARTESIAN_POINT ( 'NONE',  ( 2.783107588261252374, 7.365885187734460438, -29.97812926094515973 ) ) ;
#22732 = ORIENTED_EDGE ( 'NONE', *, *, #1689, .F. ) ;
#22733 = CARTESIAN_POINT ( 'NONE',  ( 0.000000000000000000, -17.83604598421647935, -24.70480026434186982 ) ) ;
#22734 = LINE ( 'NONE', #33570, #14331 ) ;
#22735 = CARTESIAN_POINT ( 'NONE',  ( -130.6469666100234406, 6.000000000000000000, 62.49999999999999289 ) ) ;
#22736 = EDGE_LOOP ( 'NONE', ( #9868, #27467 ) ) ;
#22737 = CARTESIAN_POINT ( 'NONE',  ( -345.0000000000000000, -125.0000000000000284, 181.0000000000000000 ) ) ;
#22738 = EDGE_LOOP ( 'NONE', ( #33536, #10174, #15496, #15282 ) ) ;
#22739 = CARTESIAN_POINT ( 'NONE',  ( -103.8279344131445470, 4.981785521925213622, 11.46442881298733241 ) ) ;
#22740 = ORIENTED_EDGE ( 'NONE', *, *, #15107, .F. ) ;
#22741 = CARTESIAN_POINT ( 'NONE',  ( -442.0000000000000000, 105.0000000000000000, 139.9999999999999716 ) ) ;
#22742 = LINE ( 'NONE', #3335, #2008 ) ;
#22743 = CARTESIAN_POINT ( 'NONE',  ( 3.235562306570555532E-30, 18.16264470403145026, -67.50000000000000000 ) ) ;
#22744 = PRODUCT_DEFINITION_SHAPE ( 'NONE', 'NONE',  #35195 ) ;
#22745 = EDGE_CURVE ( 'NONE', #8531, #25754, #34014, .T. ) ;
#22746 = VERTEX_POINT ( 'NONE', #9635 ) ;
#22747 = VECTOR ( 'NONE', #23998, 1000.000000000000000 ) ;
#22748 = EDGE_CURVE ( 'NONE', #17861, #34482, #31341, .T. ) ;
#22749 = DIRECTION ( 'NONE',  ( 2.631201909438060585E-14, -5.396010391056496978E-16, 1.000000000000000000 ) ) ;
#22750 = FACE_OUTER_BOUND ( 'NONE', #20987, .T. ) ;
#22751 = EDGE_CURVE ( 'NONE', #27517, #13700, #8026, .T. ) ;
#22752 = VERTEX_POINT ( 'NONE', #34186 ) ;
#22753 = CARTESIAN_POINT ( 'NONE',  ( -5.021133111224989953, -5.758675521474015291, -67.50000000000000000 ) ) ;
#22754 =( NAMED_UNIT ( * ) PLANE_ANGLE_UNIT ( ) SI_UNIT ( $, .RADIAN. ) );
#22755 = CARTESIAN_POINT ( 'NONE',  ( -430.0000000000000000, 132.9999999999999716, 126.0000000000000000 ) ) ;
#22756 = DIRECTION ( 'NONE',  ( 0.000000000000000000, 0.000000000000000000, 1.000000000000000000 ) ) ;
#22757 = ORIENTED_EDGE ( 'NONE', *, *, #7099, .T. ) ;
#22758 = ORIENTED_EDGE ( 'NONE', *, *, #23338, .F. ) ;
#22759 = EDGE_LOOP ( 'NONE', ( #27310, #16822, #21567, #22200 ) ) ;
#22760 = EDGE_CURVE ( 'NONE', #22002, #17949, #31515, .T. ) ;
#22761 = DIRECTION ( 'NONE',  ( -1.000000000000000000, 0.000000000000000000, -5.546364386991661285E-52 ) ) ;
#22762 = CARTESIAN_POINT ( 'NONE',  ( -10.00000000000000000, 0.000000000000000000, 0.000000000000000000 ) ) ;
#22763 = DIRECTION ( 'NONE',  ( 1.000000000000000000, 3.040835319149746528E-31, 1.232595164407830946E-32 ) ) ;
#22764 = ORIENTED_EDGE ( 'NONE', *, *, #634, .T. ) ;
#22765 = DIRECTION ( 'NONE',  ( 0.000000000000000000, 1.131431318426415506E-52, 1.000000000000000000 ) ) ;
#22766 = CARTESIAN_POINT ( 'NONE',  ( 37.09133285470120711, -7.633836879289870758, 49.43553178847298568 ) ) ;
#22767 = ORIENTED_EDGE ( 'NONE', *, *, #23425, .F. ) ;
#22768 = CARTESIAN_POINT ( 'NONE',  ( 3.235562306570555532E-30, 4.168562732279007754, -87.50000000000000000 ) ) ;
#22769 = CARTESIAN_POINT ( 'NONE',  ( 106.8660777065885412, 5.429478283318180054, 11.25942253076638089 ) ) ;
#22770 = ORIENTED_EDGE ( 'NONE', *, *, #27125, .F. ) ;
#22771 = AXIS2_PLACEMENT_3D ( 'NONE', #31077, #17399, #27688 ) ;
#22772 = EDGE_LOOP ( 'NONE', ( #4913, #7279, #22375, #21320 ) ) ;
#22773 = CYLINDRICAL_SURFACE ( 'NONE', #7216, 2.000000000000001776 ) ;
#22774 = FACE_OUTER_BOUND ( 'NONE', #29218, .T. ) ;
#22775 = ORIENTED_EDGE ( 'NONE', *, *, #34767, .F. ) ;
#22776 = DIRECTION ( 'NONE',  ( -0.000000000000000000, -0.000000000000000000, -1.000000000000000000 ) ) ;
#22777 = DIRECTION ( 'NONE',  ( -3.469446951953832974E-18, -1.000000000000000000, -7.888609052210116302E-31 ) ) ;
#22778 = DIRECTION ( 'NONE',  ( 0.000000000000000000, 1.836970198721029441E-16, -1.000000000000000000 ) ) ;
#22779 = VECTOR ( 'NONE', #19080, 1000.000000000000000 ) ;
#22780 = CARTESIAN_POINT ( 'NONE',  ( -109.9476998985492173, -1.340877102867428894, 12.43231962408541769 ) ) ;
#22781 = CARTESIAN_POINT ( 'NONE',  ( -442.0000000000000000, -105.0000000000000142, -109.9999999999999574 ) ) ;
#22782 = ADVANCED_FACE ( 'NONE', ( #20670 ), #13708, .F. ) ;
#22783 = ORIENTED_EDGE ( 'NONE', *, *, #22798, .F. ) ;
#22784 = VERTEX_POINT ( 'NONE', #26877 ) ;
#22785 = CARTESIAN_POINT ( 'NONE',  ( 790.5782620794143440, 1023.063726873133305, 1753.598338701303419 ) ) ;
#22786 = AXIS2_PLACEMENT_3D ( 'NONE', #25912, #29282, #29459 ) ;
#22787 = ADVANCED_FACE ( 'NONE', ( #35080 ), #8007, .F. ) ;
#22788 = VERTEX_POINT ( 'NONE', #183 ) ;
#22789 = EDGE_CURVE ( 'NONE', #9953, #11863, #16594, .T. ) ;
#22790 = VECTOR ( 'NONE', #15942, 1000.000000000000000 ) ;
#22791 = LINE ( 'NONE', #33820, #10721 ) ;
#22792 = EDGE_CURVE ( 'NONE', #30850, #10045, #21120, .T. ) ;
#22793 = CARTESIAN_POINT ( 'NONE',  ( 0.000000000000000000, -30.41598411195408502, -1.821977758773957179 ) ) ;
#22794 = EDGE_CURVE ( 'NONE', #18049, #30159, #2333, .T. ) ;
#22795 = ORIENTED_EDGE ( 'NONE', *, *, #2520, .T. ) ;
#22796 = CARTESIAN_POINT ( 'NONE',  ( -23.46927268871044348, -22.54767421130285143, 68.31122994652405112 ) ) ;
#22797 = CARTESIAN_POINT ( 'NONE',  ( -100.1505957388136494, -1.661087400543260761, -12.39310421627767944 ) ) ;
#22798 = EDGE_CURVE ( 'NONE', #11163, #32869, #34176, .T. ) ;
#22800 = CARTESIAN_POINT ( 'NONE',  ( 50.00050000000000239, 12.80000000000000071, 3.000000000000000000 ) ) ;
#22799 = DIRECTION ( 'NONE',  ( 0.000000000000000000, 0.000000000000000000, 1.000000000000000000 ) ) ;
#22802 = ORIENTED_EDGE ( 'NONE', *, *, #33228, .T. ) ;
#22801 = AXIS2_PLACEMENT_3D ( 'NONE', #19842, #30684, #6275 ) ;
#22803 = ORIENTED_EDGE ( 'NONE', *, *, #10687, .F. ) ;
#22804 = LINE ( 'NONE', #4599, #17459 ) ;
#22805 = AXIS2_PLACEMENT_3D ( 'NONE', #3586, #4105, #25831 ) ;
#22806 = AXIS2_PLACEMENT_3D ( 'NONE', #1156, #8804, #14346 ) ;
#22807 = CARTESIAN_POINT ( 'NONE',  ( -15.99999999999998579, -145.0000000000000000, 187.0000000000000000 ) ) ;
#22808 = CARTESIAN_POINT ( 'NONE',  ( 2.261199741344610104, 33.02096244749633769, -4.949265406681700341 ) ) ;
#22809 = VERTEX_POINT ( 'NONE', #4 ) ;
#22810 = DIRECTION ( 'NONE',  ( 0.000000000000000000, 1.224646799147353207E-16, -1.000000000000000000 ) ) ;
#22811 = LINE ( 'NONE', #28331, #30510 ) ;
#22812 = ORIENTED_EDGE ( 'NONE', *, *, #34790, .F. ) ;
#22813 = AXIS2_PLACEMENT_3D ( 'NONE', #8972, #1314, #27830 ) ;
#22814 = DIRECTION ( 'NONE',  ( -1.000000000000000000, 0.000000000000000000, 0.000000000000000000 ) ) ;
#22815 = DIRECTION ( 'NONE',  ( -0.000000000000000000, 0.000000000000000000, -1.000000000000000000 ) ) ;
#22816 = AXIS2_PLACEMENT_3D ( 'NONE', #12557, #18093, #26593 ) ;
#22817 = CARTESIAN_POINT ( 'NONE',  ( -12.00000000000001066, -124.9999999999999432, -154.9999999999999716 ) ) ;
#22819 = LINE ( 'NONE', #6073, #24744 ) ;
#22818 = PLANE ( 'NONE',  #21874 ) ;
#22820 = DIRECTION ( 'NONE',  ( 0.000000000000000000, 0.000000000000000000, 1.000000000000000000 ) ) ;
#22821 = DIRECTION ( 'NONE',  ( -1.000000000000000000, -0.000000000000000000, -0.000000000000000000 ) ) ;
#22822 = ORIENTED_EDGE ( 'NONE', *, *, #27633, .T. ) ;
#22823 = CARTESIAN_POINT ( 'NONE',  ( -15.99999999999998579, 4.559999999999908127, 168.2400000000000091 ) ) ;
#22824 =( LENGTH_UNIT ( ) NAMED_UNIT ( * ) SI_UNIT ( .MILLI., .METRE. ) );
#22825 = PRODUCT_DEFINITION_SHAPE ( 'NONE', 'NONE',  #35163 ) ;
#22826 = ORIENTED_EDGE ( 'NONE', *, *, #24897, .F. ) ;
#22827 = CIRCLE ( 'NONE', #644, 30.47050528711512030 ) ;
#22828 = SHAPE_REPRESENTATION_RELATIONSHIP ( 'NONE' , 'NONE' ,  #18474, #22006 ) ;
#22829 = VECTOR ( 'NONE', #19595, 1000.000000000000000 ) ;
#22830 = AXIS2_PLACEMENT_3D ( 'NONE', #35005, #18984, #5595 ) ;
#22831 = AXIS2_PLACEMENT_3D ( 'NONE', #4275, #4611, #12491 ) ;
#22832 = EDGE_LOOP ( 'NONE', ( #63, #28843, #34293, #25905 ) ) ;
#22833 = EDGE_CURVE ( 'NONE', #16547, #14949, #19464, .T. ) ;
#22834 = EDGE_CURVE ( 'NONE', #15568, #16675, #21549, .T. ) ;
#22835 = ORIENTED_EDGE ( 'NONE', *, *, #8334, .F. ) ;
#22836 = LINE ( 'NONE', #22307, #24665 ) ;
#22837 = EDGE_LOOP ( 'NONE', ( #17777, #29699, #26457, #8354 ) ) ;
#22838 = ORIENTED_EDGE ( 'NONE', *, *, #6889, .T. ) ;
#22839 = DIRECTION ( 'NONE',  ( 0.000000000000000000, 0.000000000000000000, 1.000000000000000000 ) ) ;
#22840 = AXIS2_PLACEMENT_3D ( 'NONE', #25325, #14677, #25502 ) ;
#22841 = VERTEX_POINT ( 'NONE', #32387 ) ;
#22842 = CARTESIAN_POINT ( 'NONE',  ( 1.999999999999999556, 0.000000000000000000, -0.7500000000000000000 ) ) ;
#22843 = DIRECTION ( 'NONE',  ( 0.000000000000000000, 1.000000000000000000, 1.131431318426415506E-52 ) ) ;
#22844 = ORIENTED_EDGE ( 'NONE', *, *, #26324, .F. ) ;
#22845 = EDGE_LOOP ( 'NONE', ( #19971, #26481, #26792, #26616 ) ) ;
#22846 =( REPRESENTATION_RELATIONSHIP ('NONE','NONE', #23037, #15767 ) REPRESENTATION_RELATIONSHIP_WITH_TRANSFORMATION ( #20648 )SHAPE_REPRESENTATION_RELATIONSHIP( ) );
#22847 = CARTESIAN_POINT ( 'NONE',  ( -442.0000000000000000, 105.0000000000000142, 162.9999999999999716 ) ) ;
#22848 = CARTESIAN_POINT ( 'NONE',  ( 2.789999999999999147, 18.92047747027354987, 23.84508255125859222 ) ) ;
#22849 = LINE ( 'NONE', #1311, #6782 ) ;
#22851 = EDGE_CURVE ( 'NONE', #1613, #8699, #29911, .T. ) ;
#22850 = DIRECTION ( 'NONE',  ( -0.000000000000000000, 6.123233995736766036E-17, 1.000000000000000000 ) ) ;
#22852 = CARTESIAN_POINT ( 'NONE',  ( -365.0000000000000000, -125.0000000000000284, 181.0000000000000000 ) ) ;
#22853 = EDGE_LOOP ( 'NONE', ( #20689, #34571, #10150, #2172 ) ) ;
#22854 = AXIS2_PLACEMENT_3D ( 'NONE', #24166, #7794, #35047 ) ;
#22855 = FACE_OUTER_BOUND ( 'NONE', #28703, .T. ) ;
#22856 = DIRECTION ( 'NONE',  ( 0.000000000000000000, -0.5288966977476834419, -0.8486862100397269959 ) ) ;
#22857 = DIRECTION ( 'NONE',  ( 0.000000000000000000, -2.465190328815661892E-32, -1.000000000000000000 ) ) ;
#22858 = ORIENTED_EDGE ( 'NONE', *, *, #25915, .T. ) ;
#22859 = CIRCLE ( 'NONE', #8611, 34.41491905851385269 ) ;
#22860 = VECTOR ( 'NONE', #25255, 1000.000000000000114 ) ;
#22861 = CARTESIAN_POINT ( 'NONE',  ( 5.021133111224369117, -1.691831803474591833, -67.50000000000000000 ) ) ;
#22863 = ADVANCED_FACE ( 'NONE', ( #2841 ), #27056, .T. ) ;
#22862 = CARTESIAN_POINT ( 'NONE',  ( 0.000000000000000000, 0.000000000000000000, 0.000000000000000000 ) ) ;
#22864 = CARTESIAN_POINT ( 'NONE',  ( -5.469264258321805627, 1.713938105891546382, 4.679999999999999716 ) ) ;
#22865 = EDGE_CURVE ( 'NONE', #8883, #9321, #2670, .T. ) ;
#22866 = CARTESIAN_POINT ( 'NONE',  ( 0.07098930928321604827, 21.26205330531119841, 23.50467731722566356 ) ) ;
#22868 = SURFACE_STYLE_USAGE ( .BOTH. , #30524 ) ;
#22867 = CARTESIAN_POINT ( 'NONE',  ( -21.17270648470164218, -7.613573412837966181, 0.000000000000000000 ) ) ;
#22869 = EDGE_CURVE ( 'NONE', #12655, #2863, #24377, .T. ) ;
#22870 = DIRECTION ( 'NONE',  ( 0.000000000000000000, 0.000000000000000000, -1.000000000000000000 ) ) ;
#22871 = VERTEX_POINT ( 'NONE', #8181 ) ;
#22872 = FACE_OUTER_BOUND ( 'NONE', #8918, .T. ) ;
#22874 = DIRECTION ( 'NONE',  ( 0.000000000000000000, 0.000000000000000000, -1.000000000000000000 ) ) ;
#22873 = CARTESIAN_POINT ( 'NONE',  ( -410.0000000000000568, -104.9999999999999716, -162.9999999999999716 ) ) ;
#22875 = ADVANCED_FACE ( 'NONE', ( #11040 ), #1805, .T. ) ;
#22876 = ORIENTED_EDGE ( 'NONE', *, *, #1438, .T. ) ;
#22877 = PRODUCT ( 'motor', 'motor', '', ( #552 ) ) ;
#22878 = DIRECTION ( 'NONE',  ( 0.000000000000000000, 1.224646799147359124E-16, 1.000000000000000000 ) ) ;
#22879 = VERTEX_POINT ( 'NONE', #30250 ) ;
#22880 = VECTOR ( 'NONE', #26699, 1000.000000000000114 ) ;
#22881 = EDGE_CURVE ( 'NONE', #6216, #23009, #19240, .T. ) ;
#22882=STYLED_ITEM('',(#35254),#24685);
#22883 = ORIENTED_EDGE ( 'NONE', *, *, #28209, .F. ) ;
#22884 = CARTESIAN_POINT ( 'NONE',  ( 107.8989562062458560, -4.964839546134684589, -5.627339305134570147 ) ) ;
#22885 = EDGE_LOOP ( 'NONE', ( #12746, #18113, #8344, #1660, #62, #27691, #6631, #18899, #17183, #25850, #3420, #3851, #25677, #2664, #25896, #1270, #19837, #7962, #25796, #22327, #27111, #27184, #10393, #18918, #23531, #24556, #31268, #3203, #2892, #19363, #6042, #2516, #1987, #13806, #9097, #12762, #15835, #21275, #10805, #15300, #28993, #1343, #6670, #33567, #17573, #834, #15938, #869, #16993, #23135, #14710, #14884, #7223, #21226, #6302, #19085, #8383, #6374, #7795, #298, #33971, #9105 ) ) ;
#22886 = EDGE_LOOP ( 'NONE', ( #26676, #15861, #32580, #18485 ) ) ;
#22887 = DIRECTION ( 'NONE',  ( 0.000000000000000000, 1.000000000000000000, 5.053935297177146739E-49 ) ) ;
#22888 = PLANE ( 'NONE',  #22126 ) ;
#22889 = LINE ( 'NONE', #20051, #14591 ) ;
#22890 = DIRECTION ( 'NONE',  ( 0.05413890858541786644, -0.9985334138511238189, 0.000000000000000000 ) ) ;
#22891 = VERTEX_POINT ( 'NONE', #16574 ) ;
#22892 = VERTEX_POINT ( 'NONE', #27404 ) ;
#22893 = DIRECTION ( 'NONE',  ( -0.000000000000000000, 1.000000000000000000, -0.000000000000000000 ) ) ;
#22894 = CARTESIAN_POINT ( 'NONE',  ( 0.000000000000000000, 2.281310696040539424E-14, -36.68877005347592757 ) ) ;
#22895 = FACE_OUTER_BOUND ( 'NONE', #14360, .T. ) ;
#22896 = DIRECTION ( 'NONE',  ( 1.000000000000000000, 3.469446951953834515E-18, 0.000000000000000000 ) ) ;
#22897 = DIRECTION ( 'NONE',  ( 1.000000000000000000, 0.000000000000000000, 0.000000000000000000 ) ) ;
#22898 = DIRECTION ( 'NONE',  ( -1.000000000000000000, 0.000000000000000000, 0.000000000000000000 ) ) ;
#22899 = CARTESIAN_POINT ( 'NONE',  ( 0.000000000000000000, 0.000000000000000000, 0.000000000000000000 ) ) ;
#22900 = ORIENTED_EDGE ( 'NONE', *, *, #32929, .F. ) ;
#22901 = EDGE_CURVE ( 'NONE', #28106, #24475, #3014, .T. ) ;
#22902 = CARTESIAN_POINT ( 'NONE',  ( 2.765921099433440666, -11.07880054387200985, -29.04985141099774637 ) ) ;
#22903 = FACE_OUTER_BOUND ( 'NONE', #10512, .T. ) ;
#22904 = EDGE_CURVE ( 'NONE', #19641, #27262, #32220, .T. ) ;
#22905 = DIRECTION ( 'NONE',  ( -1.848892746611746419E-32, -6.842277657836020854E-49, 1.000000000000000000 ) ) ;
#22906 = ORIENTED_EDGE ( 'NONE', *, *, #1684, .T. ) ;
#22907 = EDGE_CURVE ( 'NONE', #9255, #24623, #29557, .T. ) ;
#22908 = AXIS2_PLACEMENT_3D ( 'NONE', #3011, #27226, #33089 ) ;
#22909 = AXIS2_PLACEMENT_3D ( 'NONE', #26611, #10420, #4529 ) ;
#22910 = DIRECTION ( 'NONE',  ( 0.4684084406997904848, -0.8835120444460226041, 0.000000000000000000 ) ) ;
#22911 = VERTEX_POINT ( 'NONE', #33274 ) ;
#22912 = LINE ( 'NONE', #33763, #14507 ) ;
#22913 = CARTESIAN_POINT ( 'NONE',  ( -449.9999999999999432, 105.0000000000000142, 107.9999999999999858 ) ) ;
#22914 = VERTEX_POINT ( 'NONE', #22954 ) ;
#22915 = DIRECTION ( 'NONE',  ( -1.000000000000000000, 0.000000000000000000, 0.000000000000000000 ) ) ;
#22916 = FACE_OUTER_BOUND ( 'NONE', #24290, .T. ) ;
#22917 = CARTESIAN_POINT ( 'NONE',  ( -1.030735741678193262, 1.713938105891546382, 3.930000000000000160 ) ) ;
#22918 = EDGE_LOOP ( 'NONE', ( #34396, #22929, #20934, #25668 ) ) ;
#22919 = CIRCLE ( 'NONE', #9268, 10.00000000000000000 ) ;
#22920 = DIRECTION ( 'NONE',  ( 0.1063910735369155841, -0.9943243633099125844, -3.335902418025060287E-15 ) ) ;
#22921 = CYLINDRICAL_SURFACE ( 'NONE', #9093, 2.033421858999711951 ) ;
#22922 = VERTEX_POINT ( 'NONE', #16748 ) ;
#22923 = DIRECTION ( 'NONE',  ( 0.000000000000000000, -6.123233995736766036E-17, -1.000000000000000000 ) ) ;
#22924 = AXIS2_PLACEMENT_3D ( 'NONE', #10835, #8152, #26674 ) ;
#22925 = CARTESIAN_POINT ( 'NONE',  ( 19.99999999999996092, -145.0000000000000000, 162.9999999999999716 ) ) ;
#22926 = AXIS2_PLACEMENT_3D ( 'NONE', #27183, #13842, #11354 ) ;
#22927 = CARTESIAN_POINT ( 'NONE',  ( -365.0000000000000000, 134.9999999999999716, 113.9999999999999858 ) ) ;
#22928 = DIRECTION ( 'NONE',  ( 3.697785493223492838E-32, 1.934419779023891545E-16, -1.000000000000000000 ) ) ;
#22929 = ORIENTED_EDGE ( 'NONE', *, *, #30669, .T. ) ;
#22930 = EDGE_LOOP ( 'NONE', ( #15973, #22591, #23590, #28257 ) ) ;
#22931 = VECTOR ( 'NONE', #33663, 1000.000000000000000 ) ;
#22932 = ORIENTED_EDGE ( 'NONE', *, *, #415, .F. ) ;
#22933 = CARTESIAN_POINT ( 'NONE',  ( -20.02113311122509032, -13.65249191622732816, -67.50000000000000000 ) ) ;
#22934 = CARTESIAN_POINT ( 'NONE',  ( -9.144464960067645976, -31.23432620483747968, 68.31122994652405112 ) ) ;
#22935 = CARTESIAN_POINT ( 'NONE',  ( 2.719051664247837508, 31.58891575048174971, 2.579090161526253144 ) ) ;
#22936 = DIRECTION ( 'NONE',  ( -1.000000000000000000, -0.000000000000000000, -0.000000000000000000 ) ) ;
#22937 = DIRECTION ( 'NONE',  ( 0.000000000000000000, 1.000000000000000000, 1.224646799147353207E-16 ) ) ;
#22938 = CARTESIAN_POINT ( 'NONE',  ( -37.12776225901827587, -7.411627343331139706, -36.68877005347593467 ) ) ;
#22939 = ORIENTED_EDGE ( 'NONE', *, *, #31983, .T. ) ;
#22940 = MANIFOLD_SOLID_BREP ( 'Boss-Extrude4[1]', #13220 ) ;
#22941 = B_SPLINE_CURVE_WITH_KNOTS ( 'NONE', 3,
 ( #18298, #29661, #29129, #21302 ),
 .UNSPECIFIED., .F., .F.,
 ( 4, 4 ),
 ( 0.005298346101779219386, 0.005985214792934989356 ),
 .UNSPECIFIED. ) ;
#22942 = EDGE_CURVE ( 'NONE', #33679, #9083, #12077, .T. ) ;
#22943 = DIRECTION ( 'NONE',  ( -1.000000000000000000, 0.000000000000000000, 0.000000000000000000 ) ) ;
#22944 = CARTESIAN_POINT ( 'NONE',  ( 107.8850264453569707, 4.974089543361914778, 11.46991629550682212 ) ) ;
#22945 = EDGE_CURVE ( 'NONE', #34809, #1848, #678, .T. ) ;
#22946 = ORIENTED_EDGE ( 'NONE', *, *, #15825, .F. ) ;
#22947 = DIRECTION ( 'NONE',  ( -0.000000000000000000, -0.000000000000000000, -1.000000000000000000 ) ) ;
#22948 = EDGE_CURVE ( 'NONE', #20300, #1296, #20289, .T. ) ;
#22949 = AXIS2_PLACEMENT_3D ( 'NONE', #17252, #27372, #11196 ) ;
#22950 = CARTESIAN_POINT ( 'NONE',  ( 1.749999999999999778, -10.37741591188871482, -32.81304455236878681 ) ) ;
#22951 = ORIENTED_EDGE ( 'NONE', *, *, #26103, .T. ) ;
#22952 = PRODUCT_DEFINITION ( 'UNKNOWN', '', #18993, #8565 ) ;
#22953 = CARTESIAN_POINT ( 'NONE',  ( -1.625000000000000000, -1.866624223957557671, 4.679999999999999716 ) ) ;
#22954 = CARTESIAN_POINT ( 'NONE',  ( -418.0000000000000568, 141.0000000000000000, 154.9999999999999716 ) ) ;
#22955 = CARTESIAN_POINT ( 'NONE',  ( 2.790000000000000924, 9.539392014169456147, -3.000000000000000000 ) ) ;
#22956 = AXIS2_PLACEMENT_3D ( 'NONE', #4207, #31443, #28260 ) ;
#22957 = VECTOR ( 'NONE', #14699, 1000.000000000000000 ) ;
#22958 = VECTOR ( 'NONE', #17669, 1000.000000000000000 ) ;
#22959 = LINE ( 'NONE', #33808, #22829 ) ;
#22960 = LINE ( 'NONE', #22781, #9942 ) ;
#22961 = CARTESIAN_POINT ( 'NONE',  ( -12.00000000000001066, -64.99999999999997158, 154.9999999999999716 ) ) ;
#22962 = VERTEX_POINT ( 'NONE', #11758 ) ;
#22963 = ORIENTED_EDGE ( 'NONE', *, *, #29365, .F. ) ;
#22964 = CARTESIAN_POINT ( 'NONE',  ( 845.2233085191031705, 966.7087021365013015, 1753.598338701303874 ) ) ;
#22965 = ORIENTED_EDGE ( 'NONE', *, *, #26385, .T. ) ;
#22966 = DIRECTION ( 'NONE',  ( 0.000000000000000000, 0.000000000000000000, -1.000000000000000000 ) ) ;
#22967 = CIRCLE ( 'NONE', #7602, 7.999999999999979572 ) ;
#22968 = LINE ( 'NONE', #6926, #30717 ) ;
#22969 = VERTEX_POINT ( 'NONE', #539 ) ;
#22970 = FACE_OUTER_BOUND ( 'NONE', #16817, .T. ) ;
#22971 = CARTESIAN_POINT ( 'NONE',  ( -109.8499392758812121, -1.660053020383221112, -12.39330379916376756 ) ) ;
#22972 = DIRECTION ( 'NONE',  ( 0.000000000000000000, -1.000000000000000000, -2.465190328815662439E-32 ) ) ;
#22974 = LINE ( 'NONE', #25100, #32291 ) ;
#22973 = LINE ( 'NONE', #28486, #15614 ) ;
#22975 = VECTOR ( 'NONE', #22997, 1000.000000000000000 ) ;
#22976 = ORIENTED_EDGE ( 'NONE', *, *, #9196, .T. ) ;
#22977 = ORIENTED_EDGE ( 'NONE', *, *, #25463, .F. ) ;
#22978 = AXIS2_PLACEMENT_3D ( 'NONE', #29520, #16358, #32704 ) ;
#22979 = CARTESIAN_POINT ( 'NONE',  ( -499.9999999999999432, -137.0000000000000000, -162.9999999999999716 ) ) ;
#22980 = EDGE_CURVE ( 'NONE', #20852, #28991, #29660, .T. ) ;
#22981 = VECTOR ( 'NONE', #19042, 1000.000000000000000 ) ;
#22982 = EDGE_CURVE ( 'NONE', #27216, #18999, #3723, .T. ) ;
#22983 = CARTESIAN_POINT ( 'NONE',  ( -15.99999999999998579, 4.559999999999909015, 177.7400000000000091 ) ) ;
#22984 = LINE ( 'NONE', #1783, #23926 ) ;
#22985 = VERTEX_POINT ( 'NONE', #25434 ) ;
#22986 = DIRECTION ( 'NONE',  ( 0.000000000000000000, 0.000000000000000000, 1.000000000000000000 ) ) ;
#22987 = LINE ( 'NONE', #10112, #18897 ) ;
#22988 = EDGE_LOOP ( 'NONE', ( #31788, #15504, #10625, #20575 ) ) ;
#22989 = EDGE_CURVE ( 'NONE', #2726, #17921, #5199, .T. ) ;
#22990 = DIRECTION ( 'NONE',  ( 1.000000000000000000, 3.469446951953834515E-18, 0.000000000000000000 ) ) ;
#22991 = CARTESIAN_POINT ( 'NONE',  ( -9.978866888775632660, -1.691831803474591833, -67.50000000000000000 ) ) ;
#22992 = LINE ( 'NONE', #17323, #33152 ) ;
#22994 = DIRECTION ( 'NONE',  ( -0.6876994588534237618, -0.7259954919231303982, 0.000000000000000000 ) ) ;
#22993 = DIRECTION ( 'NONE',  ( 0.000000000000000000, 0.000000000000000000, -1.000000000000000000 ) ) ;
#22995 = VECTOR ( 'NONE', #7534, 1000.000000000000000 ) ;
#22996 = EDGE_CURVE ( 'NONE', #21875, #33864, #11575, .T. ) ;
#22997 = DIRECTION ( 'NONE',  ( 0.000000000000000000, 1.131431318426415506E-52, 1.000000000000000000 ) ) ;
#22998 = CARTESIAN_POINT ( 'NONE',  ( 12.00000000000001066, -64.99999999999997158, -154.9999999999999716 ) ) ;
#22999 = ORIENTED_EDGE ( 'NONE', *, *, #17256, .T. ) ;
#23000 = CARTESIAN_POINT ( 'NONE',  ( 0.000000000000000000, 0.000000000000000000, 0.000000000000000000 ) ) ;
#23001 = CARTESIAN_POINT ( 'NONE',  ( 0.1149164202474821789, -13.01099471650158712, 4.464296094009060134 ) ) ;
#23002 = CIRCLE ( 'NONE', #20711, 3.999999999999982681 ) ;
#23003 = EDGE_CURVE ( 'NONE', #1486, #34521, #1068, .T. ) ;
#23004 = ADVANCED_FACE ( 'NONE', ( #22608 ), #9071, .F. ) ;
#23005 = SURFACE_SIDE_STYLE ('',( #5571 ) ) ;
#23007 = VERTEX_POINT ( 'NONE', #6567 ) ;
#23006 = AXIS2_PLACEMENT_3D ( 'NONE', #29596, #23732, #23891 ) ;
#23008 = AXIS2_PLACEMENT_3D ( 'NONE', #26926, #32433, #27538 ) ;
#23009 = VERTEX_POINT ( 'NONE', #17465 ) ;
#23010 = AXIS2_PLACEMENT_3D ( 'NONE', #19735, #33423, #24878 ) ;
#23011 = ORIENTED_EDGE ( 'NONE', *, *, #4252, .F. ) ;
#23012 = B_SPLINE_CURVE_WITH_KNOTS ( 'NONE', 3,
 ( #16431, #32249, #15911, #24765 ),
 .UNSPECIFIED., .F., .F.,
 ( 4, 4 ),
 ( 0.005298366463358164004, 0.005985234859393915273 ),
 .UNSPECIFIED. ) ;
#23013 = CARTESIAN_POINT ( 'NONE',  ( 2.789999999999999147, 24.20451283648829133, 19.51346322004938827 ) ) ;
#23014 = EDGE_LOOP ( 'NONE', ( #19922, #27503, #23838, #2944 ) ) ;
#23015 = ORIENTED_EDGE ( 'NONE', *, *, #17654, .T. ) ;
#23016 = VERTEX_POINT ( 'NONE', #1238 ) ;
#23017 = DIRECTION ( 'NONE',  ( 0.000000000000000000, -1.836970198721029688E-16, 1.000000000000000000 ) ) ;
#23018 = ITEM_DEFINED_TRANSFORMATION ( 'NONE', 'NONE', #792,  #28566 ) ;
#23019 = VECTOR ( 'NONE', #10542, 1000.000000000000000 ) ;
#23020 = ORIENTED_EDGE ( 'NONE', *, *, #25305, .T. ) ;
#23021 = CARTESIAN_POINT ( 'NONE',  ( -12.00000000000001066, 124.9999999999999716, 159.0000000000000000 ) ) ;
#23022 = CARTESIAN_POINT ( 'NONE',  ( 5.021133111224162171, -25.61315202898006049, -67.50000000000000000 ) ) ;
#23023 = VERTEX_POINT ( 'NONE', #12109 ) ;
#23024 = VERTEX_POINT ( 'NONE', #27582 ) ;
#23025 = CARTESIAN_POINT ( 'NONE',  ( -19.99999999999998934, 75.55999999999990280, 172.9900000000000091 ) ) ;
#23026 = DIRECTION ( 'NONE',  ( 0.000000000000000000, 0.000000000000000000, 1.000000000000000000 ) ) ;
#23027 = AXIS2_PLACEMENT_3D ( 'NONE', #32503, #8125, #7951 ) ;
#23028 = FACE_OUTER_BOUND ( 'NONE', #6007, .T. ) ;
#23029 = DIRECTION ( 'NONE',  ( 0.000000000000000000, 1.836970198721029934E-16, -1.000000000000000000 ) ) ;
#23030 = FACE_BOUND ( 'NONE', #9308, .T. ) ;
#23031 = ORIENTED_EDGE ( 'NONE', *, *, #494, .T. ) ;
#23032 = CARTESIAN_POINT ( 'NONE',  ( -12.00000000000003908, -145.0000000000000000, -154.9999999999999716 ) ) ;
#23033 = CARTESIAN_POINT ( 'NONE',  ( 12.00000000000001066, -28.99999999999999645, -175.0000000000000000 ) ) ;
#23034 = VECTOR ( 'NONE', #11974, 1000.000000000000000 ) ;
#23035 = TOROIDAL_SURFACE ( 'NONE', #850, 30.47050528711511674, 8.000000000000000000 ) ;
#23036 = FACE_OUTER_BOUND ( 'NONE', #32021, .T. ) ;
#23037 = SHAPE_REPRESENTATION ( 'MAT-054', ( #28635, #19505, #18363, #4674, #26316, #32560, #151, #13804, #22337, #20638, #12119, #17254, #2431, #10979, #10389, #28591, #11545, #1874, #15509, #2986, #16099, #31978, #13249, #4122, #30875, #20068, #17809, #24021, #24578, #29729, #6973, #33686, #16663, #743, #1300, #21189, #5823, #34848, #5268, #25170, #9825, #14405, #25760, #14984, #13277, #1335, #30904, #29751, #1897, #21214, #11578, #20662, #14431, #5294, #24600, #26342, #9279, #2455, #29171, #22367, #3016, #15562, #21795, #6437, #17834, #7004, #4703, #24044, #28612, #33719, #22924, #33150, #18386, #12723, #11003, #30304, #26898, #5853, #201, #31450, #3594, #7558, #16129, #34873, #766, #23498, #25197, #13831, #15529, #9857, #34297, #32583, #18968, #27463, #10419, #12140, #4156, #8149, #28053, #32003, #17284, #185, #20088, #19530, #16689, #8715, #13852, #33746, #21241, #22956, #32028, #792, #29777, #4183, #3624, #18414, #13302, #14451, #20116, #23521, #20135, #24073, #7577, #21818, #1359, #8172, #5321, #24627, #15003, #17857, #6471, #20684, #16714, #28077, #10445, #27488, #7027, #2483, #5874, #4757, #34327, #9303, #12747, #17305, #22388, #12166, #32613, #29195, #1924, #3039, #11600, #31478, #4728, #25787 ), #26929 ) ;
#23038 = VERTEX_POINT ( 'NONE', #3195 ) ;
#23039 = CIRCLE ( 'NONE', #20768, 2.000000000000001776 ) ;
#23040 = CARTESIAN_POINT ( 'NONE',  ( -15.99999999999998579, -32.99999999999997158, -175.0000000000000000 ) ) ;
#23041 = CARTESIAN_POINT ( 'NONE',  ( -19.99999999999998934, -137.0000000000000000, 162.9999999999999716 ) ) ;
#23042 = DIRECTION ( 'NONE',  ( -0.000000000000000000, 1.836970198721029688E-16, -1.000000000000000000 ) ) ;
#23043 = ADVANCED_FACE ( 'NONE', ( #14067 ), #24902, .F. ) ;
#23044 = DIRECTION ( 'NONE',  ( -0.000000000000000000, 1.000000000000000000, -0.000000000000000000 ) ) ;
#23045 = CARTESIAN_POINT ( 'NONE',  ( 145.0000000000000568, -97.49999999999998579, 51.88904920397793319 ) ) ;
#23046 = EDGE_CURVE ( 'NONE', #21039, #26588, #10916, .T. ) ;
#23047 = EDGE_CURVE ( 'NONE', #21471, #22985, #20631, .T. ) ;
#23048 = LINE ( 'NONE', #6825, #15004 ) ;
#23049 = ORIENTED_EDGE ( 'NONE', *, *, #14840, .F. ) ;
#23050 = CARTESIAN_POINT ( 'NONE',  ( 0.006871072277270173605, 20.89672672272023135, -22.72123193261218432 ) ) ;
#23052 = CARTESIAN_POINT ( 'NONE',  ( 1.040000000000001146, -2.430610048906252985, 34.32897884578299852 ) ) ;
#23051 = FACE_OUTER_BOUND ( 'NONE', #20622, .T. ) ;
#23053 = VECTOR ( 'NONE', #2509, 1000.000000000000000 ) ;
#23054 = ORIENTED_EDGE ( 'NONE', *, *, #18772, .T. ) ;
#23055 = VECTOR ( 'NONE', #27485, 1000.000000000000000 ) ;
#23056 = PLANE ( 'NONE',  #33051 ) ;
#23057 = AXIS2_PLACEMENT_3D ( 'NONE', #16163, #35027, #31979 ) ;
#23058 = VERTEX_POINT ( 'NONE', #17982 ) ;
#23059 = ADVANCED_FACE ( 'NONE', ( #4409 ), #31476, .T. ) ;
#23060 = AXIS2_PLACEMENT_3D ( 'NONE', #19726, #16891, #6170 ) ;
#23061 = APPLICATION_CONTEXT ( 'automotive_design' ) ;
#23062 = EDGE_LOOP ( 'NONE', ( #12858, #11488, #2331, #24512 ) ) ;
#23063 = CARTESIAN_POINT ( 'NONE',  ( 3.235562306570555532E-30, 1.325223266901699007E-14, -67.50000000000000000 ) ) ;
#23064 = VERTEX_POINT ( 'NONE', #20458 ) ;
#23065 = ORIENTED_EDGE ( 'NONE', *, *, #30169, .F. ) ;
#23066 = DIRECTION ( 'NONE',  ( -0.000000000000000000, 1.836970198721029688E-16, -1.000000000000000000 ) ) ;
#23067 = VECTOR ( 'NONE', #21551, 1000.000000000000000 ) ;
#23068 = ADVANCED_FACE ( 'NONE', ( #28984 ), #15126, .F. ) ;
#23069 = CARTESIAN_POINT ( 'NONE',  ( -5.021133111225092982, -13.65249191622732816, -67.50000000000000000 ) ) ;
#23070 = EDGE_CURVE ( 'NONE', #22194, #31417, #1921, .T. ) ;
#23072 = EDGE_CURVE ( 'NONE', #1486, #11417, #25784, .T. ) ;
#23071 = DIRECTION ( 'NONE',  ( -1.000000000000000000, 0.000000000000000000, 0.000000000000000000 ) ) ;
#23073 = DIRECTION ( 'NONE',  ( -1.000000000000000000, 0.000000000000000000, 0.000000000000000000 ) ) ;
#23074 = ORIENTED_EDGE ( 'NONE', *, *, #12857, .F. ) ;
#23075 = ORIENTED_EDGE ( 'NONE', *, *, #12545, .T. ) ;
#23076 = DIRECTION ( 'NONE',  ( -1.000000000000000000, 6.792721752314501023E-48, -3.697785493223492838E-32 ) ) ;
#23077 = FACE_OUTER_BOUND ( 'NONE', #13129, .T. ) ;
#23078 = LINE ( 'NONE', #28750, #7843 ) ;
#23079 = EDGE_CURVE ( 'NONE', #18985, #10479, #34680, .T. ) ;
#23080 = DIRECTION ( 'NONE',  ( 0.000000000000000000, 1.836970198721029441E-16, -1.000000000000000000 ) ) ;
#23081 = DIRECTION ( 'NONE',  ( 0.000000000000000000, 0.000000000000000000, -1.000000000000000000 ) ) ;
#23082 = CIRCLE ( 'NONE', #7708, 1.649999999999999467 ) ;
#23083 = CARTESIAN_POINT ( 'NONE',  ( 0.000000000000000000, 0.000000000000000000, 0.000000000000000000 ) ) ;
#23084 = CARTESIAN_POINT ( 'NONE',  ( -365.0000000000000000, 118.9999999999999858, 128.0000000000000000 ) ) ;
#23085 = ORIENTED_EDGE ( 'NONE', *, *, #30535, .F. ) ;
#23086 = AXIS2_PLACEMENT_3D ( 'NONE', #34229, #31890, #7873 ) ;
#23087 = CARTESIAN_POINT ( 'NONE',  ( 31.73435513276359643, 7.220462394039750542, 68.31122994652405112 ) ) ;
#23088 = LINE ( 'NONE', #27879, #18322 ) ;
#23089 = CARTESIAN_POINT ( 'NONE',  ( -442.0000000000000000, -105.0000000000000142, -174.9999999999999432 ) ) ;
#23090 = ORIENTED_EDGE ( 'NONE', *, *, #9982, .F. ) ;
#23091 = ADVANCED_FACE ( 'NONE', ( #4061 ), #26134, .F. ) ;
#23092 = ADVANCED_FACE ( 'NONE', ( #12629 ), #23463, .F. ) ;
#23093 = PLANE ( 'NONE',  #13280 ) ;
#23094 = EDGE_LOOP ( 'NONE', ( #2602, #33995, #24310, #20070 ) ) ;
#23095 = CYLINDRICAL_SURFACE ( 'NONE', #20510, 4.000000000000003553 ) ;
#23097=STYLED_ITEM('',(#35289),#827);
#23096 = CARTESIAN_POINT ( 'NONE',  ( -8.386830662123268555E-14, 23.76564585742992719, 19.37518496788528211 ) ) ;
#23098 = AXIS2_PLACEMENT_3D ( 'NONE', #28227, #20399, #31242 ) ;
#23099 = VERTEX_POINT ( 'NONE', #1415 ) ;
#23100 = DIRECTION ( 'NONE',  ( 0.000000000000000000, -0.000000000000000000, -1.000000000000000000 ) ) ;
#23101 = CARTESIAN_POINT ( 'NONE',  ( -35.00000000000000000, -4.184937238521367675, -15.81122994652403513 ) ) ;
#23102 = VERTEX_POINT ( 'NONE', #20801 ) ;
#23103 = AXIS2_PLACEMENT_3D ( 'NONE', #2383, #29623, #34979 ) ;
#23104 = DIRECTION ( 'NONE',  ( -7.893605728314051750E-14, 1.618803117314786530E-15, 1.000000000000000000 ) ) ;
#23105 = CARTESIAN_POINT ( 'NONE',  ( 110.7380848894537024, -0.3844778738587160682, 12.50000000000000178 ) ) ;
#23106 = ORIENTED_EDGE ( 'NONE', *, *, #26224, .T. ) ;
#23107 = AXIS2_PLACEMENT_3D ( 'NONE', #2440, #13321, #21833 ) ;
#23108 = FACE_OUTER_BOUND ( 'NONE', #15049, .T. ) ;
#23109 = EDGE_CURVE ( 'NONE', #13030, #640, #29159, .T. ) ;
#23110 = FACE_BOUND ( 'NONE', #2107, .T. ) ;
#23111 = ADVANCED_FACE ( 'NONE', ( #15475 ), #30806, .T. ) ;
#23112 = LINE ( 'NONE', #26115, #11069 ) ;
#23113 = CARTESIAN_POINT ( 'NONE',  ( -442.0000000000000000, -105.0000000000000142, 194.9999999999999716 ) ) ;
#23114 = ITEM_DEFINED_TRANSFORMATION ( 'NONE', 'NONE', #22924,  #28566 ) ;
#23115 = EDGE_LOOP ( 'NONE', ( #8696, #10442, #2020, #15923, #2124, #34793, #10451, #5065, #5138, #31810 ) ) ;
#23117 = ORIENTED_EDGE ( 'NONE', *, *, #31549, .T. ) ;
#23116 =( REPRESENTATION_RELATIONSHIP ('NONE','NONE', #23037, #28231 ) REPRESENTATION_RELATIONSHIP_WITH_TRANSFORMATION ( #13777 )SHAPE_REPRESENTATION_RELATIONSHIP( ) );
#23118 = VERTEX_POINT ( 'NONE', #23136 ) ;
#23119 = CARTESIAN_POINT ( 'NONE',  ( 9.199999999999999289, -7.794228634059966687, -13.49999999999999822 ) ) ;
#23120 = AXIS2_PLACEMENT_3D ( 'NONE', #28388, #3979, #3811 ) ;
#23121 = EDGE_CURVE ( 'NONE', #4232, #26941, #4755, .T. ) ;
#23122 = CARTESIAN_POINT ( 'NONE',  ( 35.44043929807611448, -32.65143121711728469, 14.30932821646982411 ) ) ;
#23123 = CYLINDRICAL_SURFACE ( 'NONE', #28126, 7.999999999999979572 ) ;
#23124 = PLANE ( 'NONE',  #19939 ) ;
#23125 = CARTESIAN_POINT ( 'NONE',  ( -410.0000000000000568, 113.0000000000000000, -155.0000000000000000 ) ) ;
#23126 = PRESENTATION_STYLE_ASSIGNMENT (( #7072 ) ) ;
#23127 = ORIENTED_EDGE ( 'NONE', *, *, #10572, .T. ) ;
#23128 = EDGE_CURVE ( 'NONE', #9083, #21605, #152, .T. ) ;
#23129 = PRODUCT_DEFINITION_SHAPE ( 'NONE', 'NONE',  #35167 ) ;
#23130 = CARTESIAN_POINT ( 'NONE',  ( 110.5504696841441046, 1.503590720865120911, 12.41481623251361555 ) ) ;
#23131 = ORIENTED_EDGE ( 'NONE', *, *, #23860, .F. ) ;
#23132 = CIRCLE ( 'NONE', #24219, 2.000000000000001776 ) ;
#23133 = CARTESIAN_POINT ( 'NONE',  ( 11.99999999999999645, 136.9999999999999716, -175.0000000000000284 ) ) ;
#23134 = CARTESIAN_POINT ( 'NONE',  ( -414.0000000000000568, -125.0000000000000000, 187.0000000000000000 ) ) ;
#23135 = ORIENTED_EDGE ( 'NONE', *, *, #29781, .F. ) ;
#23136 = CARTESIAN_POINT ( 'NONE',  ( -35.00000000000000000, 16.36947364650383818, 36.69637551990492597 ) ) ;
#23137 = DIRECTION ( 'NONE',  ( 0.000000000000000000, -3.374343856708137958E-53, 1.000000000000000000 ) ) ;
#23138 = PLANE ( 'NONE',  #21673 ) ;
#23139 = UNCERTAINTY_MEASURE_WITH_UNIT (LENGTH_MEASURE( 1.000000000000000082E-05 ), #25664, 'distance_accuracy_value', 'NONE');
#23140 = DIRECTION ( 'NONE',  ( 0.8568571761675890519, -0.5155538571770220679, -9.470570714698675251E-17 ) ) ;
#23141 = EDGE_CURVE ( 'NONE', #33356, #34959, #12975, .T. ) ;
#23142 = CARTESIAN_POINT ( 'NONE',  ( 11.99999999999999645, 144.9999999999999716, 162.9999999999999716 ) ) ;
#23143 = ORIENTED_EDGE ( 'NONE', *, *, #5807, .F. ) ;
#23144 = EDGE_LOOP ( 'NONE', ( #29606, #21698, #29089, #28064, #16199, #25127, #7020, #31409 ) ) ;
#23145 = CARTESIAN_POINT ( 'NONE',  ( 786.4290124711920953, 1061.842355923035484, 1753.598338701303192 ) ) ;
#23146 = EDGE_LOOP ( 'NONE', ( #23462, #27353, #2940, #2916 ) ) ;
#23147 = VECTOR ( 'NONE', #33617, 1000.000000000000000 ) ;
#23148 = EDGE_CURVE ( 'NONE', #10220, #9458, #17995, .T. ) ;
#23149 = EDGE_CURVE ( 'NONE', #30081, #23628, #18841, .T. ) ;
#23150 = CARTESIAN_POINT ( 'NONE',  ( -500.0000000000000000, -113.0000000000000000, 187.0000000000000000 ) ) ;
#23151 = CIRCLE ( 'NONE', #18604, 7.999999999999952038 ) ;
#23152 = AXIS2_PLACEMENT_3D ( 'NONE', #12303, #29363, #7104 ) ;
#23153 = EDGE_CURVE ( 'NONE', #10340, #34596, #27737, .T. ) ;
#23154 = CARTESIAN_POINT ( 'NONE',  ( -1.341640786499875171, 0.000000000000000000, 0.000000000000000000 ) ) ;
#23155 = ORIENTED_EDGE ( 'NONE', *, *, #6154, .F. ) ;
#23156 = LINE ( 'NONE', #19784, #34391 ) ;
#23157 = DIRECTION ( 'NONE',  ( 0.000000000000000000, 0.000000000000000000, 1.000000000000000000 ) ) ;
#23159 = DIRECTION ( 'NONE',  ( 1.000000000000000000, 0.000000000000000000, 0.000000000000000000 ) ) ;
#23158 = CARTESIAN_POINT ( 'NONE',  ( -430.0000000000000000, -131.0000000000000000, 113.9999999999999858 ) ) ;
#23160 = ORIENTED_EDGE ( 'NONE', *, *, #34265, .T. ) ;
#23161 = VERTEX_POINT ( 'NONE', #10993 ) ;
#23162 = LINE ( 'NONE', #33478, #27657 ) ;
#23163 = CARTESIAN_POINT ( 'NONE',  ( -365.0000000000000000, 130.9999999999999716, 113.9999999999999858 ) ) ;
#23164 = LINE ( 'NONE', #6413, #19988 ) ;
#23165 = VERTEX_POINT ( 'NONE', #8321 ) ;
#23166 = DIRECTION ( 'NONE',  ( -1.300283923313630633E-47, 0.000000000000000000, -1.000000000000000000 ) ) ;
#23167 = AXIS2_PLACEMENT_3D ( 'NONE', #14176, #22174, #3299 ) ;
#23168 = VERTEX_POINT ( 'NONE', #32516 ) ;
#23169 = DIRECTION ( 'NONE',  ( 1.000000000000000000, 0.000000000000000000, 0.000000000000000000 ) ) ;
#23170 = DIRECTION ( 'NONE',  ( -0.8835120444460224931, -0.4684084406997908179, 0.000000000000000000 ) ) ;
#23172 = PLANE ( 'NONE',  #8850 ) ;
#23171 = DIRECTION ( 'NONE',  ( -3.040835319149746528E-31, -1.000000000000000000, 0.000000000000000000 ) ) ;
#23173 = AXIS2_PLACEMENT_3D ( 'NONE', #18753, #2525, #36 ) ;
#23174 = VECTOR ( 'NONE', #26566, 1000.000000000000000 ) ;
#23175 = CARTESIAN_POINT ( 'NONE',  ( -499.9999999999999432, -105.0000000000000142, -162.9999999999999716 ) ) ;
#23176 = PLANE ( 'NONE',  #34714 ) ;
#23177 = ORIENTED_EDGE ( 'NONE', *, *, #25868, .T. ) ;
#23178 = DIRECTION ( 'NONE',  ( 1.000000000000000000, 3.469446951953834515E-18, 0.000000000000000000 ) ) ;
#23179 = CARTESIAN_POINT ( 'NONE',  ( 9.199999999999999289, 7.794228634059932048, -13.49999999999999822 ) ) ;
#23180 = VERTEX_POINT ( 'NONE', #16177 ) ;
#23181 = EDGE_CURVE ( 'NONE', #6717, #24229, #26662, .T. ) ;
#23182 = ORIENTED_EDGE ( 'NONE', *, *, #2205, .F. ) ;
#23183 = ORIENTED_EDGE ( 'NONE', *, *, #6327, .T. ) ;
#23184 = ADVANCED_FACE ( 'NONE', ( #2627 ), #13150, .T. ) ;
#23185 = EDGE_CURVE ( 'NONE', #15934, #19179, #10475, .T. ) ;
#23186 = AXIS2_PLACEMENT_3D ( 'NONE', #12176, #9313, #25324 ) ;
#23187 = PLANE ( 'NONE',  #27840 ) ;
#23188 = ORIENTED_EDGE ( 'NONE', *, *, #1881, .F. ) ;
#23189 = ORIENTED_EDGE ( 'NONE', *, *, #13235, .T. ) ;
#23190 = VERTEX_POINT ( 'NONE', #34865 ) ;
#23191 = EDGE_CURVE ( 'NONE', #30714, #27733, #27185, .T. ) ;
#23192 = CARTESIAN_POINT ( 'NONE',  ( 12.00000000000001066, -134.9999999999999716, 194.9999999999999716 ) ) ;
#23193 = AXIS2_PLACEMENT_3D ( 'NONE', #32257, #8044, #5538 ) ;
#23194 = CIRCLE ( 'NONE', #22047, 34.41491905851385269 ) ;
#23195 = EDGE_LOOP ( 'NONE', ( #28393, #4084, #5210, #6484 ) ) ;
#23196 = CARTESIAN_POINT ( 'NONE',  ( -347.0000000000000000, -125.0000000000000284, 168.9999999999999716 ) ) ;
#23197 = DIRECTION ( 'NONE',  ( -0.000000000000000000, -1.000000000000000000, -0.000000000000000000 ) ) ;
#23198 = ORIENTED_EDGE ( 'NONE', *, *, #10444, .F. ) ;
#23199 = ORIENTED_EDGE ( 'NONE', *, *, #15687, .F. ) ;
#23200 = CARTESIAN_POINT ( 'NONE',  ( 0.8394537150690343230, -6.525267068024321659, 13.49999999999999822 ) ) ;
#23201 = CARTESIAN_POINT ( 'NONE',  ( 0.000000000000000000, 2.296212748401288367E-15, 87.50000000000000000 ) ) ;
#23202 = EDGE_CURVE ( 'NONE', #11184, #12833, #23982, .T. ) ;
#23203 = CARTESIAN_POINT ( 'NONE',  ( 1.749999999999999778, -30.28730148581173864, 16.34215476954022606 ) ) ;
#23204 = DIRECTION ( 'NONE',  ( -0.000000000000000000, 1.836970198721029934E-16, -1.000000000000000000 ) ) ;
#23205 = CARTESIAN_POINT ( 'NONE',  ( 0.000000000000000000, 0.000000000000000000, -57.49999999999999289 ) ) ;
#23206 = EDGE_LOOP ( 'NONE', ( #23251, #8778, #2883, #33006 ) ) ;
#23207 = AXIS2_PLACEMENT_3D ( 'NONE', #27478, #3267, #14500 ) ;
#23208 = CYLINDRICAL_SURFACE ( 'NONE', #27708, 14.77500000000000036 ) ;
#23209 = LINE ( 'NONE', #12008, #33867 ) ;
#23210 = DIRECTION ( 'NONE',  ( 0.000000000000000000, 1.000000000000000000, 0.000000000000000000 ) ) ;
#23211 = ORIENTED_EDGE ( 'NONE', *, *, #17089, .T. ) ;
#23212 = DIRECTION ( 'NONE',  ( -1.000000000000000000, 0.000000000000000000, 0.000000000000000000 ) ) ;
#23213 = PLANE ( 'NONE',  #33077 ) ;
#23214 = CARTESIAN_POINT ( 'NONE',  ( -361.0000000000000000, 124.9999999999999432, 168.9999999999999716 ) ) ;
#23215 = LINE ( 'NONE', #20715, #32564 ) ;
#23217 = DIRECTION ( 'NONE',  ( 0.000000000000000000, 0.000000000000000000, 1.000000000000000000 ) ) ;
#23216 = DIRECTION ( 'NONE',  ( -1.000000000000000000, -0.000000000000000000, -0.000000000000000000 ) ) ;
#23218 = VECTOR ( 'NONE', #33650, 1000.000000000000000 ) ;
#23219 = CARTESIAN_POINT ( 'NONE',  ( 2.604019711028809692, -0.8217981779194966085, 32.27126551972443025 ) ) ;
#23220 = VERTEX_POINT ( 'NONE', #8670 ) ;
#23221 = DIRECTION ( 'NONE',  ( 1.000000000000000000, 0.000000000000000000, 0.000000000000000000 ) ) ;
#23223 = PLANE ( 'NONE',  #27084 ) ;
#23222 = FACE_OUTER_BOUND ( 'NONE', #23014, .T. ) ;
#23224 = AXIS2_PLACEMENT_3D ( 'NONE', #32499, #8121, #5447 ) ;
#23225 = EDGE_LOOP ( 'NONE', ( #9260, #30276, #20810, #31046 ) ) ;
#23226 = COLOUR_RGB ( '',0.7921568627450980005, 0.8196078431372548767, 0.9333333333333333481 ) ;
#23227 = DIRECTION ( 'NONE',  ( -0.000000000000000000, 1.000000000000000000, 3.017235169886638201E-16 ) ) ;
#23228 = ORIENTED_EDGE ( 'NONE', *, *, #18618, .F. ) ;
#23229 = ADVANCED_FACE ( 'NONE', ( #11357 ), #33231, .F. ) ;
#23230 = AXIS2_PLACEMENT_3D ( 'NONE', #12519, #20869, #33876 ) ;
#23231 = ORIENTED_EDGE ( 'NONE', *, *, #23714, .T. ) ;
#23232 = CARTESIAN_POINT ( 'NONE',  ( 100.4809210094639980, -3.554721378204152682, -6.612463615769124559 ) ) ;
#23233 = ORIENTED_EDGE ( 'NONE', *, *, #23821, .F. ) ;
#23234 = EDGE_LOOP ( 'NONE', ( #737, #11231, #26410, #3424 ) ) ;
#23235 = EDGE_CURVE ( 'NONE', #10833, #6717, #33577, .T. ) ;
#23236 = CARTESIAN_POINT ( 'NONE',  ( 0.1859802892437388833, -18.30372525367501524, 26.59104308589815702 ) ) ;
#23237 = EDGE_CURVE ( 'NONE', #21957, #12207, #17744, .T. ) ;
#23238 = VECTOR ( 'NONE', #14772, 1000.000000000000000 ) ;
#23239 = AXIS2_PLACEMENT_3D ( 'NONE', #19884, #5971, #2294 ) ;
#23240 = FACE_OUTER_BOUND ( 'NONE', #25765, .T. ) ;
#23241 = CARTESIAN_POINT ( 'NONE',  ( 129.3530333899765594, 6.000000000000000000, -62.49999999999999289 ) ) ;
#23242 = ADVANCED_FACE ( 'NONE', ( #30572 ), #22203, .T. ) ;
#23243 = VERTEX_POINT ( 'NONE', #25031 ) ;
#23244 = EDGE_CURVE ( 'NONE', #3078, #12010, #6163, .T. ) ;
#23245 = ORIENTED_EDGE ( 'NONE', *, *, #7812, .F. ) ;
#23246 = FACE_OUTER_BOUND ( 'NONE', #4506, .T. ) ;
#23247 = PLANE ( 'NONE',  #28299 ) ;
#23248 = DIRECTION ( 'NONE',  ( -1.000000000000000000, -0.000000000000000000, -0.000000000000000000 ) ) ;
#23249 = CARTESIAN_POINT ( 'NONE',  ( 2.789999999999999147, -21.56796757982826307, 22.39322359481599278 ) ) ;
#23250 = DIRECTION ( 'NONE',  ( -1.000000000000000000, 0.000000000000000000, 0.000000000000000000 ) ) ;
#23251 = ORIENTED_EDGE ( 'NONE', *, *, #14391, .F. ) ;
#23252 = AXIS2_PLACEMENT_3D ( 'NONE', #33249, #30933, #17438 ) ;
#23253 = CYLINDRICAL_SURFACE ( 'NONE', #9957, 7.999999999999952038 ) ;
#23254 = CARTESIAN_POINT ( 'NONE',  ( 0.2204769333330994785, -10.04478976116411459, 9.601913782316108481 ) ) ;
#23255 = ORIENTED_EDGE ( 'NONE', *, *, #29181, .T. ) ;
#23256 = DIRECTION ( 'NONE',  ( 1.000000000000000000, 0.000000000000000000, 0.000000000000000000 ) ) ;
#23257 = CARTESIAN_POINT ( 'NONE',  ( 0.000000000000000000, 144.9999999999999716, -154.9999999999999716 ) ) ;
#23258 = EDGE_CURVE ( 'NONE', #10055, #32960, #27713, .T. ) ;
#23259 = PRESENTATION_LAYER_ASSIGNMENT (  '', '', ( #17028 ) ) ;
#23260 = FACE_OUTER_BOUND ( 'NONE', #13040, .T. ) ;
#23261 = VERTEX_POINT ( 'NONE', #11532 ) ;
#23262 = CARTESIAN_POINT ( 'NONE',  ( 34.14795412574902400, 16.36947364650384529, 49.43553178847298568 ) ) ;
#23263 = VERTEX_POINT ( 'NONE', #30918 ) ;
#23265 = DIRECTION ( 'NONE',  ( 0.000000000000000000, 1.310824597558155437E-49, 1.000000000000000000 ) ) ;
#23264 =( LENGTH_UNIT ( ) NAMED_UNIT ( * ) SI_UNIT ( .MILLI., .METRE. ) );
#23266 = DIRECTION ( 'NONE',  ( 1.000000000000000000, 0.000000000000000000, 0.000000000000000000 ) ) ;
#23267 = CIRCLE ( 'NONE', #9055, 34.41491905851385269 ) ;
#23268 = ADVANCED_FACE ( 'NONE', ( #24863 ), #3331, .T. ) ;
#23269 = ORIENTED_EDGE ( 'NONE', *, *, #29689, .F. ) ;
#23270 = LINE ( 'NONE', #31615, #21115 ) ;
#23271 = CARTESIAN_POINT ( 'NONE',  ( -499.9999999999999432, 136.9999999999999432, 155.0000000000000000 ) ) ;
#23272 = ORIENTED_EDGE ( 'NONE', *, *, #5419, .F. ) ;
#23273 = VECTOR ( 'NONE', #3304, 1000.000000000000000 ) ;
#23274 = ADVANCED_BREP_SHAPE_REPRESENTATION ( '', ( #22481, #28566 ), #8124 ) ;
#23275 = DIRECTION ( 'NONE',  ( -0.1063910735369225230, 0.9943243633099118073, -1.000770725407345128E-14 ) ) ;
#23276 = VERTEX_POINT ( 'NONE', #17243 ) ;
#23277 = CARTESIAN_POINT ( 'NONE',  ( 110.6987342991635188, -0.7699128213881768490, 12.48180554319666768 ) ) ;
#23278 = ORIENTED_EDGE ( 'NONE', *, *, #20298, .F. ) ;
#23279 = LINE ( 'NONE', #26111, #15609 ) ;
#23280 = CARTESIAN_POINT ( 'NONE',  ( -500.0000000000000000, -115.0000000000000000, 155.0000000000000000 ) ) ;
#23281 = PLANE ( 'NONE',  #24254 ) ;
#23282 = DIRECTION ( 'NONE',  ( 1.000000000000000000, 0.000000000000000000, -0.000000000000000000 ) ) ;
#23283 = EDGE_CURVE ( 'NONE', #11639, #11066, #22380, .T. ) ;
#23284 = ORIENTED_EDGE ( 'NONE', *, *, #27849, .T. ) ;
#23285 = EDGE_CURVE ( 'NONE', #7553, #23884, #6522, .T. ) ;
#23286 = ORIENTED_EDGE ( 'NONE', *, *, #24126, .F. ) ;
#23287 = VERTEX_POINT ( 'NONE', #19898 ) ;
#23288 = FACE_OUTER_BOUND ( 'NONE', #22439, .T. ) ;
#23289 = DIRECTION ( 'NONE',  ( 0.000000000000000000, 1.374038396813311798E-15, -1.000000000000000000 ) ) ;
#23290 = LINE ( 'NONE', #23451, #17915 ) ;
#23291 = CIRCLE ( 'NONE', #5072, 30.47050528711512030 ) ;
#23292 = DIRECTION ( 'NONE',  ( -0.5611870653623824978, 0.8276889981568904542, 1.520440023423473517E-16 ) ) ;
#23293 = CARTESIAN_POINT ( 'NONE',  ( 2.033800783032481796, -32.97757984916182039, 7.919492155587937177 ) ) ;
#23294 = SURFACE_STYLE_FILL_AREA ( #20966 ) ;
#23295 = ORIENTED_EDGE ( 'NONE', *, *, #21577, .T. ) ;
#23296 = CARTESIAN_POINT ( 'NONE',  ( -442.0000000000000000, 141.0000000000000000, 154.9999999999999716 ) ) ;
#23297 = EDGE_CURVE ( 'NONE', #8267, #6040, #20938, .T. ) ;
#23298 = EDGE_LOOP ( 'NONE', ( #23871, #10849, #8454, #13873, #28521, #19960, #15502, #30291 ) ) ;
#23299 = LINE ( 'NONE', #23134, #8102 ) ;
#23300 = ORIENTED_EDGE ( 'NONE', *, *, #29206, .T. ) ;
#23301 = DIRECTION ( 'NONE',  ( -0.000000000000000000, 0.8486862100397269959, 0.5288966977476834419 ) ) ;
#23302 = EDGE_CURVE ( 'NONE', #29908, #23325, #12879, .T. ) ;
#23303 = PLANE ( 'NONE',  #15041 ) ;
#23304 = VECTOR ( 'NONE', #24300, 1000.000000000000114 ) ;
#23305 = EDGE_CURVE ( 'NONE', #28417, #15781, #14911, .T. ) ;
#23306 = EDGE_CURVE ( 'NONE', #5849, #20728, #620, .T. ) ;
#23307 = CARTESIAN_POINT ( 'NONE',  ( -442.0000000000000000, -125.0000000000000000, -101.9999999999999858 ) ) ;
#23308 = CYLINDRICAL_SURFACE ( 'NONE', #2539, 7.999999999999979572 ) ;
#23309 = ADVANCED_FACE ( 'NONE', ( #9723 ), #1545, .T. ) ;
#23310 = ORIENTED_EDGE ( 'NONE', *, *, #442, .F. ) ;
#23311 = EDGE_LOOP ( 'NONE', ( #19573, #19202, #13993, #11864 ) ) ;
#23312 = DIRECTION ( 'NONE',  ( -0.1063910735369017202, 0.9943243633099136947, -1.000770725407181676E-14 ) ) ;
#23313 =( REPRESENTATION_RELATIONSHIP ('NONE','NONE', #23037, #15767 ) REPRESENTATION_RELATIONSHIP_WITH_TRANSFORMATION ( #19385 )SHAPE_REPRESENTATION_RELATIONSHIP( ) );
#23314 = ORIENTED_EDGE ( 'NONE', *, *, #9845, .F. ) ;
#23315 = DIRECTION ( 'NONE',  ( 1.000000000000000000, 0.000000000000000000, 0.000000000000000000 ) ) ;
#23316 = EDGE_CURVE ( 'NONE', #30469, #4119, #30750, .T. ) ;
#23317 = CARTESIAN_POINT ( 'NONE',  ( -442.0000000000000000, 113.0000000000000000, -175.0000000000000000 ) ) ;
#23318 = VERTEX_POINT ( 'NONE', #22913 ) ;
#23319 = DIRECTION ( 'NONE',  ( -1.232595164407830946E-32, -3.421138828918010427E-49, 1.000000000000000000 ) ) ;
#23320 = CARTESIAN_POINT ( 'NONE',  ( -110.1150203881707910, -7.176976838982289656E-16, -12.50000000000000000 ) ) ;
#23321 = AXIS2_PLACEMENT_3D ( 'NONE', #21729, #29925, #5519 ) ;
#23323 = DIRECTION ( 'NONE',  ( -1.000000000000000000, 0.000000000000000000, 0.000000000000000000 ) ) ;
#23322 = LINE ( 'NONE', #34168, #29242 ) ;
#23324 = ORIENTED_EDGE ( 'NONE', *, *, #25915, .F. ) ;
#23325 = VERTEX_POINT ( 'NONE', #25930 ) ;
#23326 = CARTESIAN_POINT ( 'NONE',  ( -410.0000000000000568, 105.0000000000000000, -77.99999999999997158 ) ) ;
#23327 = CARTESIAN_POINT ( 'NONE',  ( 2.033589661659781722, 21.20732892273832704, -26.46721543659820242 ) ) ;
#23328 = CARTESIAN_POINT ( 'NONE',  ( 22.89764159710613001, 6.310691531022070144, -77.50000000000000000 ) ) ;
#23329 = ORIENTED_EDGE ( 'NONE', *, *, #27568, .T. ) ;
#23330 = CARTESIAN_POINT ( 'NONE',  ( 3.235562306570555532E-30, 24.02303923978505296, -87.50000000000000000 ) ) ;
#23331 = EDGE_LOOP ( 'NONE', ( #4460, #22068, #33313, #8024 ) ) ;
#23332 = CARTESIAN_POINT ( 'NONE',  ( 1.749999999999999778, -25.27164158951550732, -23.36088151536945645 ) ) ;
#23333 = CARTESIAN_POINT ( 'NONE',  ( -11.83261234297099662, -30.31820670846267873, 68.31122994652405112 ) ) ;
#23334 = DIRECTION ( 'NONE',  ( -0.3701381553399144542, 0.9289767198167914186, 1.706502549609061988E-16 ) ) ;
#23335 = ADVANCED_FACE ( 'NONE', ( #33764 ), #19378, .T. ) ;
#23337 = CARTESIAN_POINT ( 'NONE',  ( 2.781508616055402339, -26.25561000592817607, -16.27441264773137419 ) ) ;
#23336 = PLANE ( 'NONE',  #6525 ) ;
#23338 = EDGE_CURVE ( 'NONE', #20533, #32765, #20763, .T. ) ;
#23339 = LINE ( 'NONE', #26171, #7051 ) ;
#23340 = DIRECTION ( 'NONE',  ( 0.000000000000000000, 1.000000000000000000, 0.000000000000000000 ) ) ;
#23341 = CARTESIAN_POINT ( 'NONE',  ( -20.02113311122509032, -15.68591377522703745, -67.50000000000000000 ) ) ;
#23342 = AXIS2_PLACEMENT_3D ( 'NONE', #24846, #24481, #8481 ) ;
#23343 = CIRCLE ( 'NONE', #6278, 3.999999999999976019 ) ;
#23344 = ORIENTED_EDGE ( 'NONE', *, *, #11983, .F. ) ;
#23345 = VERTEX_POINT ( 'NONE', #28770 ) ;
#23346 = EDGE_LOOP ( 'NONE', ( #29259, #19564, #9794, #12682, #31800, #34816, #17276, #30791, #24563, #8803, #177, #2284 ) ) ;
#23347 = CIRCLE ( 'NONE', #20506, 7.999999999999979572 ) ;
#23348 = LINE ( 'NONE', #467, #1119 ) ;
#23349 = EDGE_LOOP ( 'NONE', ( #28362, #26890, #27399, #20007 ) ) ;
#23350 = VECTOR ( 'NONE', #16311, 1000.000000000000000 ) ;
#23351 = ORIENTED_EDGE ( 'NONE', *, *, #2723, .F. ) ;
#23352 = ORIENTED_EDGE ( 'NONE', *, *, #16948, .F. ) ;
#23353 = LINE ( 'NONE', #1298, #8241 ) ;
#23354 = CONTEXT_DEPENDENT_SHAPE_REPRESENTATION ( #24906, #24078 ) ;
#23355 = ORIENTED_EDGE ( 'NONE', *, *, #3557, .F. ) ;
#23356 = PLANE ( 'NONE',  #29462 ) ;
#23357 = FACE_BOUND ( 'NONE', #29842, .T. ) ;
#23358 = ORIENTED_EDGE ( 'NONE', *, *, #16566, .F. ) ;
#23359 = EDGE_LOOP ( 'NONE', ( #22424, #15971, #17036, #32008 ) ) ;
#23360 = CARTESIAN_POINT ( 'NONE',  ( 0.000000000000000000, 0.000000000000000000, 0.000000000000000000 ) ) ;
#23362 = CARTESIAN_POINT ( 'NONE',  ( 2.789999999999999147, 26.03801215795542134, -16.98986790278583570 ) ) ;
#23361 = AXIS2_PLACEMENT_3D ( 'NONE', #12399, #28926, #15584 ) ;
#23363 = CARTESIAN_POINT ( 'NONE',  ( 1.040000000000001590, 32.09669216789235691, 12.41728656686385968 ) ) ;
#23364 = DIRECTION ( 'NONE',  ( -0.000000000000000000, 1.000000000000000000, -0.000000000000000000 ) ) ;
#23365 = DIRECTION ( 'NONE',  ( 1.000000000000000000, 0.000000000000000000, 0.000000000000000000 ) ) ;
#23366 = EDGE_LOOP ( 'NONE', ( #22757, #17903, #8242, #1291 ) ) ;
#23367 = AXIS2_PLACEMENT_3D ( 'NONE', #19303, #2902, #2380 ) ;
#23368 = CARTESIAN_POINT ( 'NONE',  ( -500.0000000000000000, -145.0000000000000000, 162.9999999999999716 ) ) ;
#23369 = CARTESIAN_POINT ( 'NONE',  ( -445.9999999999999432, -105.0000000000000142, 132.0000000000000000 ) ) ;
#23370 = CARTESIAN_POINT ( 'NONE',  ( -9.978866888775632660, -3.725253662474300231, -87.50000000000000000 ) ) ;
#23371 = ORIENTED_EDGE ( 'NONE', *, *, #17337, .T. ) ;
#23372 = CARTESIAN_POINT ( 'NONE',  ( -2.791255079241054649, -37.75727539589166071, 68.31122994652405112 ) ) ;
#23373 = EDGE_CURVE ( 'NONE', #12065, #14482, #15420, .T. ) ;
#23374 = DIRECTION ( 'NONE',  ( 1.000000000000000000, 0.000000000000000000, 0.000000000000000000 ) ) ;
#23375 = CARTESIAN_POINT ( 'NONE',  ( 110.1953605866412715, 2.443267496989373733, -7.093208238637026319 ) ) ;
#23377 = DIRECTION ( 'NONE',  ( 0.000000000000000000, -1.000000000000000000, 0.000000000000000000 ) ) ;
#23376 = LINE ( 'NONE', #18068, #25250 ) ;
#23378 = ADVANCED_FACE ( 'NONE', ( #23607 ), #7041, .F. ) ;
#23379 = AXIS2_PLACEMENT_3D ( 'NONE', #17133, #30109, #27438 ) ;
#23380 = AXIS2_PLACEMENT_3D ( 'NONE', #16578, #27410, #18721 ) ;
#23381 = CARTESIAN_POINT ( 'NONE',  ( -20.00000000000007461, 140.9999999999999432, 187.0000000000000000 ) ) ;
#23383 = ORIENTED_EDGE ( 'NONE', *, *, #15999, .T. ) ;
#23382 = VECTOR ( 'NONE', #8628, 1000.000000000000000 ) ;
#23385 = MECHANICAL_DESIGN_GEOMETRIC_PRESENTATION_REPRESENTATION (  '', ( #651 ), #29068 ) ;
#23384 = CARTESIAN_POINT ( 'NONE',  ( 109.3193400707606031, 3.795444455902927228, -11.91305592319909223 ) ) ;
#23387 = CARTESIAN_POINT ( 'NONE',  ( 1.205771365940040196, 7.794228634059932048, -13.49999999999999822 ) ) ;
#23386 = CARTESIAN_POINT ( 'NONE',  ( -414.0000000000000568, 104.9999999999999858, -187.0000000000000000 ) ) ;
#23388 = ORIENTED_EDGE ( 'NONE', *, *, #14348, .F. ) ;
#23389 = PLANE ( 'NONE',  #32464 ) ;
#23390 = EDGE_LOOP ( 'NONE', ( #30711, #379 ) ) ;
#23391 = AXIS2_PLACEMENT_3D ( 'NONE', #7676, #13044, #18572 ) ;
#23392 = ORIENTED_EDGE ( 'NONE', *, *, #30950, .T. ) ;
#23393 = CARTESIAN_POINT ( 'NONE',  ( 1.040000000000000924, 0.000000000000000000, 0.000000000000000000 ) ) ;
#23394 = ORIENTED_EDGE ( 'NONE', *, *, #18916, .F. ) ;
#23395 = ORIENTED_EDGE ( 'NONE', *, *, #25479, .T. ) ;
#23396 = CARTESIAN_POINT ( 'NONE',  ( -499.9999999999999432, -137.0000000000000000, -194.9999999999999716 ) ) ;
#23397 = PRODUCT_DEFINITION_SHAPE ( 'NONE', 'NONE',  #35170 ) ;
#23398=STYLED_ITEM('',(#35254),#34343);
#23399 = CARTESIAN_POINT ( 'NONE',  ( -20.00000000000001776, -113.0000000000000000, 194.9999999999999716 ) ) ;
#23400 = AXIS2_PLACEMENT_3D ( 'NONE', #8134, #16349, #16880 ) ;
#23401 = LINE ( 'NONE', #13084, #5158 ) ;
#23402 = B_SPLINE_CURVE_WITH_KNOTS ( 'NONE', 3,
 ( #32426, #2013, #15547, #32258, #7876, #31892 ),
 .UNSPECIFIED., .F., .F.,
 ( 4, 2, 4 ),
 ( 2.333473478908367993E-07, 0.001873431678079542006, 0.003746630008811193454 ),
 .UNSPECIFIED. ) ;
#23403 = ORIENTED_EDGE ( 'NONE', *, *, #12501, .F. ) ;
#23404 = VERTEX_POINT ( 'NONE', #4535 ) ;
#23405 = AXIS2_PLACEMENT_3D ( 'NONE', #12252, #26449, #23100 ) ;
#23406 = LINE ( 'NONE', #31419, #8833 ) ;
#23407 = CARTESIAN_POINT ( 'NONE',  ( -25.07182831876307105, -28.36910952062232738, -36.68877005347593467 ) ) ;
#23408 =( GEOMETRIC_REPRESENTATION_CONTEXT ( 3 ) GLOBAL_UNCERTAINTY_ASSIGNED_CONTEXT ( ( #11808 ) ) GLOBAL_UNIT_ASSIGNED_CONTEXT ( ( #9432, #28113, #3371 ) ) REPRESENTATION_CONTEXT ( 'NONE', 'WORKASPACE' ) );
#23409 = CARTESIAN_POINT ( 'NONE',  ( 1.040000000000001368, -33.26546734453825138, 8.820166447041648539 ) ) ;
#23410 = DIRECTION ( 'NONE',  ( 0.000000000000000000, -1.000000000000000000, -5.145227585319922065E-49 ) ) ;
#23411 = DIRECTION ( 'NONE',  ( -0.8276889981568904542, 0.5611870653623824978, 0.000000000000000000 ) ) ;
#23412 = ORIENTED_EDGE ( 'NONE', *, *, #6208, .T. ) ;
#23413 = VERTEX_POINT ( 'NONE', #15431 ) ;
#23414 = CARTESIAN_POINT ( 'NONE',  ( -414.0000000000000568, -105.0000000000000142, 107.9999999999999858 ) ) ;
#23415 = DIRECTION ( 'NONE',  ( 0.000000000000000000, 1.836970198721029688E-16, -1.000000000000000000 ) ) ;
#23416 = VERTEX_POINT ( 'NONE', #26266 ) ;
#23417 = DIRECTION ( 'NONE',  ( -0.000000000000000000, -0.000000000000000000, -1.000000000000000000 ) ) ;
#23418 = CARTESIAN_POINT ( 'NONE',  ( -499.9999999999999432, 136.9999999999999432, -194.9999999999999716 ) ) ;
#23419 = ADVANCED_FACE ( 'NONE', ( #1884, #4017 ), #12248, .T. ) ;
#23420 = AXIS2_PLACEMENT_3D ( 'NONE', #19352, #19529, #5790 ) ;
#23421 = DIRECTION ( 'NONE',  ( -0.000000000000000000, 1.000000000000000000, -0.000000000000000000 ) ) ;
#23422 = ORIENTED_EDGE ( 'NONE', *, *, #32394, .T. ) ;
#23423 = LINE ( 'NONE', #10073, #27491 ) ;
#23424 = ORIENTED_EDGE ( 'NONE', *, *, #25270, .T. ) ;
#23425 = EDGE_CURVE ( 'NONE', #8710, #14706, #9389, .T. ) ;
#23427 = CARTESIAN_POINT ( 'NONE',  ( 2.789999999999999147, 9.869977788040968036, 30.37666815053940539 ) ) ;
#23426 = LINE ( 'NONE', #31264, #13704 ) ;
#23428 = CARTESIAN_POINT ( 'NONE',  ( -107.5740197209480726, 4.432569708812558851, 11.68934771181378451 ) ) ;
#23429 = PRESENTATION_LAYER_ASSIGNMENT (  '', '', ( #4071 ) ) ;
#23431 = ORIENTED_EDGE ( 'NONE', *, *, #32339, .T. ) ;
#23430 = VECTOR ( 'NONE', #2748, 1000.000000000000000 ) ;
#23432 = EDGE_CURVE ( 'NONE', #1235, #22809, #6698, .T. ) ;
#23433 = LINE ( 'NONE', #4375, #5749 ) ;
#23434 = CARTESIAN_POINT ( 'NONE',  ( -35.00000000000000000, -46.95407462254104303, 36.69637551990492597 ) ) ;
#23435 = EDGE_CURVE ( 'NONE', #14210, #22879, #24114, .T. ) ;
#23436 = ORIENTED_EDGE ( 'NONE', *, *, #34320, .F. ) ;
#23437 = CARTESIAN_POINT ( 'NONE',  ( 791.2698036807846620, 1016.600622031483113, 1753.598338701303419 ) ) ;
#23438 = ORIENTED_EDGE ( 'NONE', *, *, #33193, .T. ) ;
#23439 = CARTESIAN_POINT ( 'NONE',  ( 104.6174907297543939, -5.728493955922441927, 11.11012212270733990 ) ) ;
#23440 = ORIENTED_EDGE ( 'NONE', *, *, #31894, .F. ) ;
#23441 = LINE ( 'NONE', #34296, #19020 ) ;
#23442 = CARTESIAN_POINT ( 'NONE',  ( -19.99999999999998934, 75.55999999999990280, 172.9900000000000091 ) ) ;
#23443 = CARTESIAN_POINT ( 'NONE',  ( 19.99999999999998934, -145.0000000000000000, -186.9999999999999716 ) ) ;
#23444 = CARTESIAN_POINT ( 'NONE',  ( -29.34345171400087793, 14.07715221144534823, 68.31122994652405112 ) ) ;
#23445 = ORIENTED_EDGE ( 'NONE', *, *, #11998, .T. ) ;
#23446 = VERTEX_POINT ( 'NONE', #35002 ) ;
#23447 = ORIENTED_EDGE ( 'NONE', *, *, #9673, .F. ) ;
#23448 = PRODUCT_DEFINITION_SHAPE ( 'NONE', 'NONE',  #35116 ) ;
#23449 = CARTESIAN_POINT ( 'NONE',  ( 24.11848021413634768, 29.19488569250030352, 49.43553178847298568 ) ) ;
#23450 = DIRECTION ( 'NONE',  ( 0.000000000000000000, 0.000000000000000000, 1.000000000000000000 ) ) ;
#23451 = CARTESIAN_POINT ( 'NONE',  ( 11.99999999999999645, -124.9999999999999432, -158.9999999999999716 ) ) ;
#23452 = DIRECTION ( 'NONE',  ( 0.000000000000000000, 1.836970198721029688E-16, -1.000000000000000000 ) ) ;
#23453 = AXIS2_PLACEMENT_3D ( 'NONE', #7172, #1504, #31057 ) ;
#23454 = PLANE ( 'NONE',  #4372 ) ;
#23455 = AXIS2_PLACEMENT_3D ( 'NONE', #22374, #8662, #21835 ) ;
#23456 = DIRECTION ( 'NONE',  ( 0.000000000000000000, -1.000000000000000000, -2.465190328815662439E-32 ) ) ;
#23457 = ORIENTED_EDGE ( 'NONE', *, *, #26797, .F. ) ;
#23458 = LINE ( 'NONE', #25469, #2056 ) ;
#23459 = LINE ( 'NONE', #21141, #12623 ) ;
#23460 = EDGE_LOOP ( 'NONE', ( #30743, #19045, #23198, #7766 ) ) ;
#23461 = CARTESIAN_POINT ( 'NONE',  ( 24.90835164106607280, -28.52396285516520891, 68.31122994652405112 ) ) ;
#23462 = ORIENTED_EDGE ( 'NONE', *, *, #34727, .F. ) ;
#23463 = PLANE ( 'NONE',  #34798 ) ;
#23464 = EDGE_CURVE ( 'NONE', #14949, #4850, #24457, .T. ) ;
#23465 = FACE_OUTER_BOUND ( 'NONE', #24192, .T. ) ;
#23466 = EDGE_CURVE ( 'NONE', #27067, #18455, #26620, .T. ) ;
#23467 = ADVANCED_FACE ( 'NONE', ( #29302 ), #5591, .F. ) ;
#23468 = DIRECTION ( 'NONE',  ( 0.000000000000000000, -1.000000000000000000, -2.132064625830773463E-16 ) ) ;
#23469 = DIRECTION ( 'NONE',  ( 0.000000000000000000, 1.000000000000000000, 0.000000000000000000 ) ) ;
#23470 = B_SPLINE_CURVE_WITH_KNOTS ( 'NONE', 3,
 ( #20005, #30849, #9314, #10188 ),
 .UNSPECIFIED., .F., .F.,
 ( 4, 4 ),
 ( 3.346525879906762451E-07, 0.0006880714927763405177 ),
 .UNSPECIFIED. ) ;
#23471 = ORIENTED_EDGE ( 'NONE', *, *, #26865, .T. ) ;
#23472 = ORIENTED_EDGE ( 'NONE', *, *, #7099, .F. ) ;
#23473 = AXIS2_PLACEMENT_3D ( 'NONE', #28065, #6695, #22910 ) ;
#23474 = VECTOR ( 'NONE', #19247, 1000.000000000000000 ) ;
#23475 = DIRECTION ( 'NONE',  ( -7.893605728314050488E-14, 1.618803117314786135E-15, 0.9999999999999998890 ) ) ;
#23476 = AXIS2_PLACEMENT_3D ( 'NONE', #27305, #30336, #18969 ) ;
#23477 = ORIENTED_EDGE ( 'NONE', *, *, #24691, .F. ) ;
#23478 = EDGE_CURVE ( 'NONE', #21604, #16288, #8098, .T. ) ;
#23479 = CARTESIAN_POINT ( 'NONE',  ( 11.99999999999995559, -134.9999999999999716, -194.9999999999999432 ) ) ;
#23480 = DIRECTION ( 'NONE',  ( -1.000000000000000000, 0.000000000000000000, 0.000000000000000000 ) ) ;
#23481 = CARTESIAN_POINT ( 'NONE',  ( 109.8288047610148936, -3.105058450138034498, 6.829076936735990699 ) ) ;
#23482 = CONTEXT_DEPENDENT_SHAPE_REPRESENTATION ( #7592, #9802 ) ;
#23483 = EDGE_LOOP ( 'NONE', ( #32489, #16495, #20557, #27558 ) ) ;
#23484 = CARTESIAN_POINT ( 'NONE',  ( -430.0000000000000000, 114.9999999999999716, 126.0000000000000000 ) ) ;
#23485 = ADVANCED_FACE ( 'NONE', ( #4896 ), #15789, .F. ) ;
#23486 = EDGE_CURVE ( 'NONE', #2835, #18207, #29477, .T. ) ;
#23487 = CIRCLE ( 'NONE', #31996, 2.000000000000001776 ) ;
#23489 = CYLINDRICAL_SURFACE ( 'NONE', #23817, 16.19999999999999574 ) ;
#23488 = CARTESIAN_POINT ( 'NONE',  ( -441.9999999999999432, -141.0000000000000000, 154.9999999999999716 ) ) ;
#23490 = ORIENTED_EDGE ( 'NONE', *, *, #17476, .F. ) ;
#23491 = VERTEX_POINT ( 'NONE', #10428 ) ;
#23492 = CARTESIAN_POINT ( 'NONE',  ( 15.99999999999998579, 75.55999999999990280, -172.9900000000000091 ) ) ;
#23493 = ORIENTED_EDGE ( 'NONE', *, *, #14642, .F. ) ;
#23494 = ADVANCED_FACE ( 'NONE', ( #21288 ), #2408, .T. ) ;
#23495 = PLANE ( 'NONE',  #2814 ) ;
#23496 = CARTESIAN_POINT ( 'NONE',  ( 2.789999999999999147, 14.59907093257254296, -26.74544485249450787 ) ) ;
#23497 = ORIENTED_EDGE ( 'NONE', *, *, #11670, .T. ) ;
#23498 = AXIS2_PLACEMENT_3D ( 'NONE', #22392, #16539, #30581 ) ;
#23499 = CARTESIAN_POINT ( 'NONE',  ( 2.783107618827354024, -21.36453267519060617, -22.28230728414027340 ) ) ;
#23500 = AXIS2_PLACEMENT_3D ( 'NONE', #19078, #8275, #30158 ) ;
#23501 = CIRCLE ( 'NONE', #8153, 3.999999999999976019 ) ;
#23502 = PRODUCT_DEFINITION_SHAPE ( 'NONE', 'NONE',  #35210 ) ;
#23503 = ORIENTED_EDGE ( 'NONE', *, *, #3948, .F. ) ;
#23504 = DIRECTION ( 'NONE',  ( -1.000000000000000000, 0.000000000000000000, 0.000000000000000000 ) ) ;
#23505 = DIRECTION ( 'NONE',  ( -1.232595164407830946E-32, -3.421138828918010427E-49, 1.000000000000000000 ) ) ;
#23506 = DIRECTION ( 'NONE',  ( 0.000000000000000000, 0.000000000000000000, -1.000000000000000000 ) ) ;
#23508 = CARTESIAN_POINT ( 'NONE',  ( 0.000000000000000000, 3.524919873834583163E-15, 68.31122994652405112 ) ) ;
#23507 = FACE_OUTER_BOUND ( 'NONE', #28790, .T. ) ;
#23509 = EDGE_CURVE ( 'NONE', #20630, #22441, #32134, .T. ) ;
#23510 = EDGE_CURVE ( 'NONE', #12627, #18640, #5424, .T. ) ;
#23511 =( REPRESENTATION_RELATIONSHIP ('NONE','NONE', #23037, #34141 ) REPRESENTATION_RELATIONSHIP_WITH_TRANSFORMATION ( #21914 )SHAPE_REPRESENTATION_RELATIONSHIP( ) );
#23512 = FACE_OUTER_BOUND ( 'NONE', #30840, .T. ) ;
#23513 = CARTESIAN_POINT ( 'NONE',  ( 0.5344654698445945318, 14.30876692738954858, -2.216488688100095139 ) ) ;
#23514 = CARTESIAN_POINT ( 'NONE',  ( 0.7561992140789179917, -9.974544214302882850, 32.41523709743427872 ) ) ;
#23515 = CARTESIAN_POINT ( 'NONE',  ( 0.5288002571296349652, -28.88016830755685405, -16.75753762755175558 ) ) ;
#23516 = MANIFOLD_SOLID_BREP ( 'Cut-Extrude1', #17395 ) ;
#23517 = VECTOR ( 'NONE', #22044, 1000.000000000000000 ) ;
#23518 = ORIENTED_EDGE ( 'NONE', *, *, #7786, .T. ) ;
#23519 = VERTEX_POINT ( 'NONE', #16137 ) ;
#23520 = VERTEX_POINT ( 'NONE', #31950 ) ;
#23521 = AXIS2_PLACEMENT_3D ( 'NONE', #6535, #1721, #1553 ) ;
#23522 = CIRCLE ( 'NONE', #11035, 2.033421858999711507 ) ;
#23523 = CARTESIAN_POINT ( 'NONE',  ( 110.1195297133390625, 2.618976401886136340, 7.037310091161540271 ) ) ;
#23524 = CARTESIAN_POINT ( 'NONE',  ( 811.0931266444453058, 1361.079637510369821, 1753.598338701303192 ) ) ;
#23525 = ORIENTED_EDGE ( 'NONE', *, *, #29386, .F. ) ;
#23526 = ORIENTED_EDGE ( 'NONE', *, *, #32010, .T. ) ;
#23527 = ORIENTED_EDGE ( 'NONE', *, *, #6773, .F. ) ;
#23528 = DIRECTION ( 'NONE',  ( 0.000000000000000000, 0.000000000000000000, 1.000000000000000000 ) ) ;
#23529 = EDGE_CURVE ( 'NONE', #3883, #8463, #1756, .T. ) ;
#23530 = EDGE_CURVE ( 'NONE', #25265, #25155, #2756, .T. ) ;
#23531 = ORIENTED_EDGE ( 'NONE', *, *, #5037, .T. ) ;
#23532 = CARTESIAN_POINT ( 'NONE',  ( 2.789999999999999147, 14.59907093257254296, -26.74544485249450787 ) ) ;
#23533 = CARTESIAN_POINT ( 'NONE',  ( 15.99999999999998579, -56.99999999999997868, -175.0000000000000000 ) ) ;
#23534 = ORIENTED_EDGE ( 'NONE', *, *, #14015, .F. ) ;
#23535 = ORIENTED_EDGE ( 'NONE', *, *, #12233, .T. ) ;
#23536 = CARTESIAN_POINT ( 'NONE',  ( -414.0000000000000568, -105.0000000000000142, -101.9999999999999858 ) ) ;
#23537 = CARTESIAN_POINT ( 'NONE',  ( -1.030735741678193262, 1.713938105891546382, 5.429999999999999716 ) ) ;
#23538 = DIRECTION ( 'NONE',  ( 1.000000000000000000, 0.000000000000000000, 0.000000000000000000 ) ) ;
#23539 = CARTESIAN_POINT ( 'NONE',  ( 10.00000000000000000, 2.296212748401288367E-15, 87.50000000000000000 ) ) ;
#23540 = DIRECTION ( 'NONE',  ( -1.000000000000000000, 0.000000000000000000, 0.000000000000000000 ) ) ;
#23541 = ORIENTED_EDGE ( 'NONE', *, *, #20612, .T. ) ;
#23542 = CARTESIAN_POINT ( 'NONE',  ( 44.94043929807611448, -32.65143121711728469, 0.000000000000000000 ) ) ;
#23543 = CARTESIAN_POINT ( 'NONE',  ( -35.55956070192387841, -12.65143121711728291, 14.30932821646982411 ) ) ;
#23544 = VECTOR ( 'NONE', #18992, 1000.000000000000000 ) ;
#23545 = PLANE ( 'NONE',  #1673 ) ;
#23546 = VERTEX_POINT ( 'NONE', #17328 ) ;
#23547 = EDGE_CURVE ( 'NONE', #29867, #11190, #28342, .T. ) ;
#23548 = VECTOR ( 'NONE', #24924, 1000.000000000000000 ) ;
#23549 = CARTESIAN_POINT ( 'NONE',  ( -12.00000000000001066, 134.9999999999999432, -186.9999999999999716 ) ) ;
#23550 = DIRECTION ( 'NONE',  ( -1.000000000000000000, 0.000000000000000000, 0.000000000000000000 ) ) ;
#23551 = DIRECTION ( 'NONE',  ( 3.697785493223492838E-32, 1.934419779023891545E-16, -1.000000000000000000 ) ) ;
#23552 = LINE ( 'NONE', #12368, #21772 ) ;
#23554 = CARTESIAN_POINT ( 'NONE',  ( -105.6968603966071498, 5.070301591678565423, -5.526538532257564640 ) ) ;
#23553 = DIRECTION ( 'NONE',  ( 1.000000000000000000, 0.000000000000000000, 0.000000000000000000 ) ) ;
#23555 = AXIS2_PLACEMENT_3D ( 'NONE', #8936, #22119, #22292 ) ;
#23556 = AXIS2_PLACEMENT_3D ( 'NONE', #33856, #17152, #25833 ) ;
#23557 = CARTESIAN_POINT ( 'NONE',  ( 0.000000000000000000, 11.69134295108991495, 6.750000000000012434 ) ) ;
#23558 = ORIENTED_EDGE ( 'NONE', *, *, #27521, .F. ) ;
#23559 = CARTESIAN_POINT ( 'NONE',  ( 99.56251466041456410, 1.870982065537967420, -12.36420004006153839 ) ) ;
#23561 = CYLINDRICAL_SURFACE ( 'NONE', #6625, 1.155000000000000027 ) ;
#23560 = FACE_OUTER_BOUND ( 'NONE', #5739, .T. ) ;
#23562 = AXIS2_PLACEMENT_3D ( 'NONE', #16196, #23661, #7446 ) ;
#23563 = ORIENTED_EDGE ( 'NONE', *, *, #31868, .F. ) ;
#23564 = DIRECTION ( 'NONE',  ( 0.000000000000000000, -1.000000000000000000, -3.083952846180991760E-16 ) ) ;
#23565 = ADVANCED_FACE ( 'NONE', ( #31348 ), #17150, .T. ) ;
#23566 = ORIENTED_EDGE ( 'NONE', *, *, #1927, .T. ) ;
#23567 = CIRCLE ( 'NONE', #29822, 7.999999999999979572 ) ;
#23568 = ORIENTED_EDGE ( 'NONE', *, *, #21653, .F. ) ;
#23569 = CARTESIAN_POINT ( 'NONE',  ( 2.789999999999999147, 0.000000000000000000, 0.000000000000000000 ) ) ;
#23570 = EDGE_LOOP ( 'NONE', ( #26955, #31863, #16027, #29474 ) ) ;
#23571 = ORIENTED_EDGE ( 'NONE', *, *, #29136, .T. ) ;
#23572 = CARTESIAN_POINT ( 'NONE',  ( -20.63749999999999574, 0.000000000000000000, -16.00000000000000000 ) ) ;
#23573 = AXIS2_PLACEMENT_3D ( 'NONE', #25238, #28094, #874 ) ;
#23574 = ADVANCED_FACE ( 'NONE', ( #19980 ), #14822, .F. ) ;
#23575 = ORIENTED_EDGE ( 'NONE', *, *, #21570, .T. ) ;
#23576 = EDGE_CURVE ( 'NONE', #18057, #9166, #4008, .T. ) ;
#23577 = ADVANCED_FACE ( 'NONE', ( #19327 ), #1284, .F. ) ;
#23578 = TOROIDAL_SURFACE ( 'NONE', #4255, 30.47050528711511674, 8.000000000000000000 ) ;
#23579 = DIRECTION ( 'NONE',  ( -1.000000000000000000, -0.000000000000000000, 0.000000000000000000 ) ) ;
#23580 = DIRECTION ( 'NONE',  ( 0.000000000000000000, -3.374343856708137958E-53, 1.000000000000000000 ) ) ;
#23581 = ORIENTED_EDGE ( 'NONE', *, *, #34960, .T. ) ;
#23582 = ORIENTED_EDGE ( 'NONE', *, *, #6965, .F. ) ;
#23583 = CIRCLE ( 'NONE', #4813, 3.999999999999976019 ) ;
#23584 = CARTESIAN_POINT ( 'NONE',  ( -363.0000000000000000, 134.9999999999999716, 126.0000000000000000 ) ) ;
#23585 = DIRECTION ( 'NONE',  ( 1.000000000000000000, 0.000000000000000000, -0.000000000000000000 ) ) ;
#23586 = DIRECTION ( 'NONE',  ( 0.000000000000000000, -1.000000000000000000, -0.000000000000000000 ) ) ;
#23587 = CIRCLE ( 'NONE', #23010, 2.525000000000001243 ) ;
#23588 = LINE ( 'NONE', #29458, #8465 ) ;
#23589 = FACE_OUTER_BOUND ( 'NONE', #1690, .T. ) ;
#23590 = ORIENTED_EDGE ( 'NONE', *, *, #31366, .F. ) ;
#23591 = ORIENTED_EDGE ( 'NONE', *, *, #15677, .T. ) ;
#23592 = CARTESIAN_POINT ( 'NONE',  ( -43.31669544645773584, 30.33919503331657808, 6.106833536353696523 ) ) ;
#23593 = CARTESIAN_POINT ( 'NONE',  ( -5.210000000000000853, 0.000000000000000000, 0.000000000000000000 ) ) ;
#23594 = ORIENTED_EDGE ( 'NONE', *, *, #2027, .F. ) ;
#23595 = PLANE ( 'NONE',  #13953 ) ;
#23596 = CARTESIAN_POINT ( 'NONE',  ( -12.00000000000001066, -124.9999999999999432, -154.9999999999999716 ) ) ;
#23597 = ORIENTED_EDGE ( 'NONE', *, *, #22760, .T. ) ;
#23598 = CARTESIAN_POINT ( 'NONE',  ( -34.66645501699844090, -15.21971901163155216, 68.31122994652405112 ) ) ;
#23599 = ORIENTED_EDGE ( 'NONE', *, *, #25707, .F. ) ;
#23600 = AXIS2_PLACEMENT_3D ( 'NONE', #31198, #4121, #15184 ) ;
#23601 = CIRCLE ( 'NONE', #3701, 3.999999999999976019 ) ;
#23602 = DIRECTION ( 'NONE',  ( 0.000000000000000000, -1.000000000000000000, -5.145227585319922065E-49 ) ) ;
#23603 = VERTEX_POINT ( 'NONE', #3934 ) ;
#23605 = DIRECTION ( 'NONE',  ( 1.000000000000000000, 0.000000000000000000, 0.000000000000000000 ) ) ;
#23604 = DIRECTION ( 'NONE',  ( 1.000000000000000000, 0.000000000000000000, 0.000000000000000000 ) ) ;
#23606 = AXIS2_PLACEMENT_3D ( 'NONE', #31935, #34448, #13443 ) ;
#23607 = FACE_OUTER_BOUND ( 'NONE', #19772, .T. ) ;
#23608 = VERTEX_POINT ( 'NONE', #25309 ) ;
#23609 = CIRCLE ( 'NONE', #21356, 30.47050528711512030 ) ;
#23610 = FACE_OUTER_BOUND ( 'NONE', #12088, .T. ) ;
#23611 = AXIS2_PLACEMENT_3D ( 'NONE', #31745, #5040, #34254 ) ;
#23612 = LINE ( 'NONE', #7394, #29864 ) ;
#23613 = CIRCLE ( 'NONE', #28716, 7.999999999999979572 ) ;
#23614 = VERTEX_POINT ( 'NONE', #11977 ) ;
#23615 = VECTOR ( 'NONE', #7190, 1000.000000000000000 ) ;
#23616 = DIRECTION ( 'NONE',  ( -0.1063910735369225230, 0.9943243633099118073, -1.000770725407345128E-14 ) ) ;
#23617 = EDGE_CURVE ( 'NONE', #14065, #8194, #7432, .T. ) ;
#23618 = ORIENTED_EDGE ( 'NONE', *, *, #1686, .T. ) ;
#23619 = CARTESIAN_POINT ( 'NONE',  ( 109.9600497711273448, -2.891119662789794820, 12.16223328578254836 ) ) ;
#23620 = ORIENTED_EDGE ( 'NONE', *, *, #2668, .F. ) ;
#23621 = DIRECTION ( 'NONE',  ( 0.000000000000000000, 0.000000000000000000, 1.000000000000000000 ) ) ;
#23622 = EDGE_CURVE ( 'NONE', #12785, #33069, #13752, .T. ) ;
#23623 = DIRECTION ( 'NONE',  ( 1.000000000000000000, 0.000000000000000000, 0.000000000000000000 ) ) ;
#23624 = VECTOR ( 'NONE', #25728, 1000.000000000000000 ) ;
#23625 = EDGE_CURVE ( 'NONE', #12505, #7313, #6929, .T. ) ;
#23626 = CARTESIAN_POINT ( 'NONE',  ( -101.6279274993559198, -3.859727759966185001, -6.435874498883202399 ) ) ;
#23627 = FACE_OUTER_BOUND ( 'NONE', #26998, .T. ) ;
#23628 = VERTEX_POINT ( 'NONE', #22998 ) ;
#23629 = ORIENTED_EDGE ( 'NONE', *, *, #19818, .F. ) ;
#23630 = VERTEX_POINT ( 'NONE', #33854 ) ;
#23631 = ADVANCED_FACE ( 'NONE', ( #6430 ), #22657, .F. ) ;
#23632 = PLANE ( 'NONE',  #2128 ) ;
#23633 = CIRCLE ( 'NONE', #20242, 16.00000000000000000 ) ;
#23634 = DIRECTION ( 'NONE',  ( -1.000000000000000000, 0.000000000000000000, -0.000000000000000000 ) ) ;
#23635 = DIRECTION ( 'NONE',  ( -0.000000000000000000, -1.000000000000000000, -0.000000000000000000 ) ) ;
#23636 = FACE_BOUND ( 'NONE', #32709, .T. ) ;
#23637 = DIRECTION ( 'NONE',  ( 0.000000000000000000, 0.000000000000000000, 1.000000000000000000 ) ) ;
#23638 = ORIENTED_EDGE ( 'NONE', *, *, #16252, .T. ) ;
#23639 = VECTOR ( 'NONE', #5897, 1000.000000000000000 ) ;
#23640 = DIRECTION ( 'NONE',  ( 0.000000000000000000, 0.9961946980917455452, -0.08715574274765887364 ) ) ;
#23641 = EDGE_CURVE ( 'NONE', #8202, #12737, #3770, .T. ) ;
#23642 = CARTESIAN_POINT ( 'NONE',  ( 11.99999999999999645, 124.9999999999999716, 155.0000000000000000 ) ) ;
#23643 = DIRECTION ( 'NONE',  ( 1.000000000000000000, 0.000000000000000000, 0.000000000000000000 ) ) ;
#23644 = ORIENTED_EDGE ( 'NONE', *, *, #10963, .F. ) ;
#23645 = DIRECTION ( 'NONE',  ( 0.000000000000000000, 1.131431318426415506E-52, 1.000000000000000000 ) ) ;
#23646 = EDGE_LOOP ( 'NONE', ( #25720, #8288, #16757, #18409 ) ) ;
#23647 = CARTESIAN_POINT ( 'NONE',  ( 145.0000000000000568, 85.49999999999998579, 65.00000000000000000 ) ) ;
#23648 = DIRECTION ( 'NONE',  ( 1.000000000000000000, 0.000000000000000000, 0.000000000000000000 ) ) ;
#23649 = VECTOR ( 'NONE', #8780, 1000.000000000000000 ) ;
#23650 = LINE ( 'NONE', #31821, #34737 ) ;
#23651 = CARTESIAN_POINT ( 'NONE',  ( -418.0000000000000000, 124.9999999999999432, -162.9999999999999716 ) ) ;
#23652 = CARTESIAN_POINT ( 'NONE',  ( 11.62236370382047923, -30.39942490923500884, 49.43553178847298568 ) ) ;
#23653 = AXIS2_PLACEMENT_3D ( 'NONE', #15463, #33315, #14643 ) ;
#23654 = VERTEX_POINT ( 'NONE', #33670 ) ;
#23655 = ORIENTED_EDGE ( 'NONE', *, *, #34274, .T. ) ;
#23656 = CARTESIAN_POINT ( 'NONE',  ( 817.6345509492954307, 1342.999246745606115, 1753.598338701303419 ) ) ;
#23657 = ORIENTED_EDGE ( 'NONE', *, *, #27957, .F. ) ;
#23658 = VECTOR ( 'NONE', #24729, 1000.000000000000114 ) ;
#23659 = CARTESIAN_POINT ( 'NONE',  ( 3.235562306570555532E-30, 18.16264470403145381, -87.50000000000000000 ) ) ;
#23660 = B_SPLINE_CURVE_WITH_KNOTS ( 'NONE', 3,
 ( #6900, #22598, #20625, #25427, #25600, #19927 ),
 .UNSPECIFIED., .F., .F.,
 ( 4, 2, 4 ),
 ( 4.404817133663990876E-07, 0.001874269703891902252, 0.003748098926070445210 ),
 .UNSPECIFIED. ) ;
#23661 = DIRECTION ( 'NONE',  ( -0.000000000000000000, -0.000000000000000000, -1.000000000000000000 ) ) ;
#23662 = CARTESIAN_POINT ( 'NONE',  ( 102.1010437937541298, -4.964839546134684589, 5.627339305134570147 ) ) ;
#23663 = ORIENTED_EDGE ( 'NONE', *, *, #27974, .T. ) ;
#23664 = EDGE_CURVE ( 'NONE', #1613, #12821, #26476, .T. ) ;
#23665 = CARTESIAN_POINT ( 'NONE',  ( -349.0000000000000000, -125.0000000000000284, 164.9999999999999716 ) ) ;
#23666 = EDGE_CURVE ( 'NONE', #23700, #17587, #9294, .T. ) ;
#23667 = AXIS2_PLACEMENT_3D ( 'NONE', #13568, #24759, #32941 ) ;
#23669 = PLANE ( 'NONE',  #11299 ) ;
#23668 = DIRECTION ( 'NONE',  ( 1.000000000000000000, 3.469446951953834515E-18, 0.000000000000000000 ) ) ;
#23670 = VERTEX_POINT ( 'NONE', #12328 ) ;
#23671 = ORIENTED_EDGE ( 'NONE', *, *, #18809, .F. ) ;
#23672 = ADVANCED_FACE ( 'NONE', ( #24637, #28510, #21989 ), #23176, .T. ) ;
#23673 = EDGE_CURVE ( 'NONE', #4640, #4766, #23691, .T. ) ;
#23674 = CARTESIAN_POINT ( 'NONE',  ( 1.749999999999999778, 22.14447232807545163, -26.34405054495532639 ) ) ;
#23675 = ORIENTED_EDGE ( 'NONE', *, *, #8237, .F. ) ;
#23676 = AXIS2_PLACEMENT_3D ( 'NONE', #32988, #33175, #11478 ) ;
#23677 = LINE ( 'NONE', #29192, #27818 ) ;
#23678 = CARTESIAN_POINT ( 'NONE',  ( -442.0000000000000000, -109.0000000000000142, 155.0000000000000000 ) ) ;
#23679 = ORIENTED_EDGE ( 'NONE', *, *, #1394, .T. ) ;
#23680 = DIRECTION ( 'NONE',  ( 1.000000000000000000, 0.000000000000000000, 0.000000000000000000 ) ) ;
#23681 = VERTEX_POINT ( 'NONE', #31689 ) ;
#23682 = VECTOR ( 'NONE', #22335, 1000.000000000000000 ) ;
#23683 = DIRECTION ( 'NONE',  ( 0.000000000000000000, 0.000000000000000000, 1.000000000000000000 ) ) ;
#23684 = B_SPLINE_CURVE_WITH_KNOTS ( 'NONE', 3,
 ( #5221, #21783, #10402, #2737, #26949, #5049 ),
 .UNSPECIFIED., .F., .F.,
 ( 4, 2, 4 ),
 ( 2.717607641618553552E-07, 0.001873470133380086616, 0.003746668505996011457 ),
 .UNSPECIFIED. ) ;
#23685 = FACE_OUTER_BOUND ( 'NONE', #16316, .T. ) ;
#23686 = EDGE_CURVE ( 'NONE', #21237, #16, #7457, .T. ) ;
#23687 = DIRECTION ( 'NONE',  ( 1.000000000000000000, 0.000000000000000000, 0.000000000000000000 ) ) ;
#23689 = DIRECTION ( 'NONE',  ( 0.000000000000000000, 1.310824597558155437E-49, 1.000000000000000000 ) ) ;
#23688 = DIRECTION ( 'NONE',  ( 0.000000000000000000, 1.000000000000000000, -3.374343856708137958E-53 ) ) ;
#23690 = CYLINDRICAL_SURFACE ( 'NONE', #27513, 7.999999999999979572 ) ;
#23691 = LINE ( 'NONE', #29021, #23902 ) ;
#23692 = DIRECTION ( 'NONE',  ( -1.000000000000000000, 0.000000000000000000, -0.000000000000000000 ) ) ;
#23693 = FACE_OUTER_BOUND ( 'NONE', #32187, .T. ) ;
#23694 = PRODUCT_DEFINITION_SHAPE ( 'NONE', 'NONE',  #35151 ) ;
#23695 = CIRCLE ( 'NONE', #21411, 14.20000000000000107 ) ;
#23696 = ADVANCED_FACE ( 'NONE', ( #18555 ), #4453, .F. ) ;
#23697 = VECTOR ( 'NONE', #26472, 999.9999999999998863 ) ;
#23698 = ORIENTED_EDGE ( 'NONE', *, *, #28223, .F. ) ;
#23699 = ADVANCED_FACE ( 'NONE', ( #12676 ), #26530, .T. ) ;
#23700 = VERTEX_POINT ( 'NONE', #13197 ) ;
#23701 = ORIENTED_EDGE ( 'NONE', *, *, #32961, .F. ) ;
#23702 = CARTESIAN_POINT ( 'NONE',  ( 107.9015628886182867, 4.963291960430601613, 5.628698742319545367 ) ) ;
#23703 = ORIENTED_EDGE ( 'NONE', *, *, #15224, .T. ) ;
#23704 = ORIENTED_EDGE ( 'NONE', *, *, #13101, .T. ) ;
#23705 = ORIENTED_EDGE ( 'NONE', *, *, #33723, .T. ) ;
#23706 = LINE ( 'NONE', #21393, #24142 ) ;
#23707 = DIRECTION ( 'NONE',  ( 0.9985334138511239299, 0.05413890858541756113, -0.000000000000000000 ) ) ;
#23708 = VERTEX_POINT ( 'NONE', #17846 ) ;
#23709 = CARTESIAN_POINT ( 'NONE',  ( -20.00000000000007461, 112.9999999999999574, 187.0000000000000000 ) ) ;
#23710 = PLANE ( 'NONE',  #26230 ) ;
#23711 = ORIENTED_EDGE ( 'NONE', *, *, #2174, .F. ) ;
#23712 = ORIENTED_EDGE ( 'NONE', *, *, #21058, .F. ) ;
#23713 = EDGE_CURVE ( 'NONE', #169, #27132, #34909, .T. ) ;
#23714 = EDGE_CURVE ( 'NONE', #10924, #27638, #4600, .T. ) ;
#23715 = CARTESIAN_POINT ( 'NONE',  ( -12.00000000000001066, -32.99999999999997158, -175.0000000000000000 ) ) ;
#23716 = LINE ( 'NONE', #24231, #27180 ) ;
#23717 = VECTOR ( 'NONE', #5583, 1000.000000000000000 ) ;
#23718 = DIRECTION ( 'NONE',  ( -0.000000000000000000, -0.000000000000000000, -1.000000000000000000 ) ) ;
#23719 = EDGE_CURVE ( 'NONE', #6202, #24651, #14304, .T. ) ;
#23720 = LINE ( 'NONE', #5011, #6289 ) ;
#23721 = CARTESIAN_POINT ( 'NONE',  ( -30.76765767668600660, -10.60922306139172555, 68.31122994652405112 ) ) ;
#23722 = ORIENTED_EDGE ( 'NONE', *, *, #10375, .T. ) ;
#23724 = AXIS2_PLACEMENT_3D ( 'NONE', #14196, #1142, #20193 ) ;
#23723 = DIRECTION ( 'NONE',  ( 3.697785493223492838E-32, 1.934419779023891545E-16, -1.000000000000000000 ) ) ;
#23726 = CARTESIAN_POINT ( 'NONE',  ( -365.0000000000000000, -131.0000000000000000, 109.9999999999999858 ) ) ;
#23725 = AXIS2_PLACEMENT_3D ( 'NONE', #16972, #41, #8405 ) ;
#23727 = ORIENTED_EDGE ( 'NONE', *, *, #4398, .T. ) ;
#23728 = CARTESIAN_POINT ( 'NONE',  ( 22.10765473302597073, -16.64466345897532662, -77.50000000000000000 ) ) ;
#23729 = CARTESIAN_POINT ( 'NONE',  ( -7.700000000000000178, 0.000000000000000000, -9.999999999999998224 ) ) ;
#23730 = DIRECTION ( 'NONE',  ( 0.000000000000000000, 0.000000000000000000, -1.000000000000000000 ) ) ;
#23731 = VECTOR ( 'NONE', #22546, 1000.000000000000114 ) ;
#23733 = CARTESIAN_POINT ( 'NONE',  ( -12.00000000000001066, -145.0000000000000000, -154.9999999999999716 ) ) ;
#23732 = DIRECTION ( 'NONE',  ( 1.000000000000000000, 0.000000000000000000, 0.000000000000000000 ) ) ;
#23734 = DIRECTION ( 'NONE',  ( -0.000000000000000000, 1.836970198721029688E-16, -1.000000000000000000 ) ) ;
#23735 = ORIENTED_EDGE ( 'NONE', *, *, #32382, .F. ) ;
#23736 = LINE ( 'NONE', #1670, #22393 ) ;
#23738 = LINE ( 'NONE', #17899, #9491 ) ;
#23737 = PLANE ( 'NONE',  #2411 ) ;
#23739 = EDGE_CURVE ( 'NONE', #22581, #14635, #24027, .T. ) ;
#23740 = EDGE_CURVE ( 'NONE', #9411, #2729, #21022, .T. ) ;
#23741 = ADVANCED_FACE ( 'NONE', ( #34369 ), #28680, .F. ) ;
#23742 = AXIS2_PLACEMENT_3D ( 'NONE', #5253, #637, #32487 ) ;
#23743 = ORIENTED_EDGE ( 'NONE', *, *, #22942, .T. ) ;
#23744 = DIRECTION ( 'NONE',  ( -0.000000000000000000, -0.000000000000000000, 1.000000000000000000 ) ) ;
#23745 = EDGE_CURVE ( 'NONE', #10400, #20728, #17174, .T. ) ;
#23746 = VERTEX_POINT ( 'NONE', #12850 ) ;
#23747 = VECTOR ( 'NONE', #11256, 1000.000000000000000 ) ;
#23748 = CIRCLE ( 'NONE', #24877, 7.999999999999979572 ) ;
#23749 = EDGE_CURVE ( 'NONE', #24468, #14881, #10523, .T. ) ;
#23750 = EDGE_CURVE ( 'NONE', #26118, #8857, #9813, .T. ) ;
#23751 = ORIENTED_EDGE ( 'NONE', *, *, #30371, .F. ) ;
#23752 = CARTESIAN_POINT ( 'NONE',  ( -25.14484813934701535, 2.898127806110619709, -15.07978102403234644 ) ) ;
#23753 = ORIENTED_EDGE ( 'NONE', *, *, #9771, .F. ) ;
#23754 = ORIENTED_EDGE ( 'NONE', *, *, #19786, .F. ) ;
#23755 = CARTESIAN_POINT ( 'NONE',  ( -449.9999999999999432, 104.9999999999999858, -175.0000000000000000 ) ) ;
#23756 = VECTOR ( 'NONE', #33347, 1000.000000000000000 ) ;
#23757 = DIRECTION ( 'NONE',  ( 1.000000000000000000, 0.000000000000000000, -0.000000000000000000 ) ) ;
#23758 = CARTESIAN_POINT ( 'NONE',  ( -15.99999999999998579, 136.9999999999999716, 155.0000000000000000 ) ) ;
#23759 = EDGE_LOOP ( 'NONE', ( #27690, #24267, #11087, #9025, #20849, #17728, #31594, #14474 ) ) ;
#23760 = EDGE_LOOP ( 'NONE', ( #16735, #31472, #15326, #14344 ) ) ;
#23761 = CARTESIAN_POINT ( 'NONE',  ( 2.789999999999999147, 30.11551674275786539, -4.430359003076015156 ) ) ;
#23762 = DIRECTION ( 'NONE',  ( 0.000000000000000000, -1.000000000000000000, 6.123233995736766036E-17 ) ) ;
#23763 = CARTESIAN_POINT ( 'NONE',  ( -17.07420202168509604, 33.79163469797341435, 68.31122994652405112 ) ) ;
#23764 = DIRECTION ( 'NONE',  ( -1.000000000000000000, 0.000000000000000000, 0.000000000000000000 ) ) ;
#23765 = ORIENTED_EDGE ( 'NONE', *, *, #15313, .F. ) ;
#23766 = LINE ( 'NONE', #28930, #871 ) ;
#23767 = VECTOR ( 'NONE', #20864, 1000.000000000000000 ) ;
#23768 = FACE_OUTER_BOUND ( 'NONE', #8640, .T. ) ;
#23769 = VERTEX_POINT ( 'NONE', #18197 ) ;
#23770 = DIRECTION ( 'NONE',  ( 0.000000000000000000, 0.000000000000000000, -1.000000000000000000 ) ) ;
#23771 = CARTESIAN_POINT ( 'NONE',  ( 2.765921099433444219, 31.00221527374952046, 2.344426712874309260 ) ) ;
#23772 = LINE ( 'NONE', #34630, #33371 ) ;
#23773 = ORIENTED_EDGE ( 'NONE', *, *, #20430, .T. ) ;
#23774 = DIRECTION ( 'NONE',  ( 0.000000000000000000, -1.000000000000000000, 0.000000000000000000 ) ) ;
#23775 = VERTEX_POINT ( 'NONE', #26172 ) ;
#23776 = VECTOR ( 'NONE', #25622, 1000.000000000000000 ) ;
#23777 =( REPRESENTATION_RELATIONSHIP ('NONE','NONE', #23037, #28231 ) REPRESENTATION_RELATIONSHIP_WITH_TRANSFORMATION ( #14092 )SHAPE_REPRESENTATION_RELATIONSHIP( ) );
#23778 = VECTOR ( 'NONE', #347, 1000.000000000000000 ) ;
#23779 = DIRECTION ( 'NONE',  ( -0.6473862847818285804, 0.7621620551276356847, 0.000000000000000000 ) ) ;
#23780 = ORIENTED_EDGE ( 'NONE', *, *, #27361, .F. ) ;
#23782 = DIRECTION ( 'NONE',  ( 0.000000000000000000, -1.000000000000000000, 6.842277657836020854E-49 ) ) ;
#23781 = DIRECTION ( 'NONE',  ( -1.000000000000000000, -0.000000000000000000, 0.000000000000000000 ) ) ;
#23783 = VECTOR ( 'NONE', #34935, 1000.000000000000000 ) ;
#23784 = ADVANCED_FACE ( 'NONE', ( #18025 ), #26357, .F. ) ;
#23785 = EDGE_CURVE ( 'NONE', #11116, #15497, #26706, .T. ) ;
#23786 = VERTEX_POINT ( 'NONE', #28852 ) ;
#23787 = LINE ( 'NONE', #1717, #26244 ) ;
#23788 = CARTESIAN_POINT ( 'NONE',  ( 0.000000000000000000, 0.000000000000000000, 0.000000000000000000 ) ) ;
#23789 = ORIENTED_EDGE ( 'NONE', *, *, #23823, .T. ) ;
#23790 = CIRCLE ( 'NONE', #7277, 7.999999999999979572 ) ;
#23791 = DIRECTION ( 'NONE',  ( -0.1063910735369225230, 0.9943243633099118073, -1.000770725407345128E-14 ) ) ;
#23792 = ORIENTED_EDGE ( 'NONE', *, *, #31143, .T. ) ;
#23793 = CARTESIAN_POINT ( 'NONE',  ( 105.9428472181658236, -5.663308120860370387, 11.14355020191728940 ) ) ;
#23794 = ORIENTED_EDGE ( 'NONE', *, *, #19013, .T. ) ;
#23795 = FACE_BOUND ( 'NONE', #22736, .T. ) ;
#23796 = DIRECTION ( 'NONE',  ( 1.000000000000000000, 0.000000000000000000, 0.000000000000000000 ) ) ;
#23797 =( GEOMETRIC_REPRESENTATION_CONTEXT ( 3 ) GLOBAL_UNCERTAINTY_ASSIGNED_CONTEXT ( ( #15585 ) ) GLOBAL_UNIT_ASSIGNED_CONTEXT ( ( #5257, #24133, #29318 ) ) REPRESENTATION_CONTEXT ( 'NONE', 'WORKASPACE' ) );
#23798 = CARTESIAN_POINT ( 'NONE',  ( 11.99999999999999645, 134.9999999999998863, 155.0000000000000000 ) ) ;
#23799 = CARTESIAN_POINT ( 'NONE',  ( 0.1859802861825020359, 32.15598440394879276, -2.846506069495843949 ) ) ;
#23800 = CONTEXT_DEPENDENT_SHAPE_REPRESENTATION ( #11944, #26236 ) ;
#23801 = ORIENTED_EDGE ( 'NONE', *, *, #15351, .F. ) ;
#23802 = EDGE_LOOP ( 'NONE', ( #24659, #27806 ) ) ;
#23803 = PRODUCT_DEFINITION_SHAPE ( 'NONE', 'NONE',  #35230 ) ;
#23804 = ORIENTED_EDGE ( 'NONE', *, *, #8350, .T. ) ;
#23805 = CARTESIAN_POINT ( 'NONE',  ( 145.0000000000000568, -88.29863524074325198, -74.12844257252345415 ) ) ;
#23806 = DIRECTION ( 'NONE',  ( 0.000000000000000000, 0.000000000000000000, 1.000000000000000000 ) ) ;
#23807 = VECTOR ( 'NONE', #4227, 1000.000000000000114 ) ;
#23808 = CARTESIAN_POINT ( 'NONE',  ( 99.26191511054632599, 0.000000000000000000, -57.49999999999999289 ) ) ;
#23809 = DIRECTION ( 'NONE',  ( 1.000000000000000000, -0.000000000000000000, -0.000000000000000000 ) ) ;
#23810 = DIRECTION ( 'NONE',  ( 0.000000000000000000, -6.123233995736766036E-17, -1.000000000000000000 ) ) ;
#23811 = DIRECTION ( 'NONE',  ( -1.000000000000000000, 0.000000000000000000, -0.000000000000000000 ) ) ;
#23812 = ORIENTED_EDGE ( 'NONE', *, *, #28529, .T. ) ;
#23813 = LINE ( 'NONE', #129, #26495 ) ;
#23814 = CARTESIAN_POINT ( 'NONE',  ( 99.26191511054632599, 1.643815732525060864E-21, 12.50000000000000000 ) ) ;
#23815 = DIRECTION ( 'NONE',  ( -1.000000000000000000, -3.469446951953834515E-18, 2.736911063134582149E-48 ) ) ;
#23816 = ORIENTED_EDGE ( 'NONE', *, *, #21058, .T. ) ;
#23817 = AXIS2_PLACEMENT_3D ( 'NONE', #20998, #23323, #34169 ) ;
#23818 = CARTESIAN_POINT ( 'NONE',  ( 27.64943126350855707, -17.16721653852535212, 68.31122994652405112 ) ) ;
#23819 = ORIENTED_EDGE ( 'NONE', *, *, #23739, .F. ) ;
#23820 = CARTESIAN_POINT ( 'NONE',  ( 3.235562306570555532E-30, 8.235406450278427215, -67.50000000000000000 ) ) ;
#23821 = EDGE_CURVE ( 'NONE', #24518, #14045, #19245, .T. ) ;
#23822 = DIRECTION ( 'NONE',  ( -1.000000000000000000, -0.000000000000000000, -0.000000000000000000 ) ) ;
#23823 = EDGE_CURVE ( 'NONE', #27322, #33889, #29915, .T. ) ;
#23824 = VERTEX_POINT ( 'NONE', #13373 ) ;
#23825 = CARTESIAN_POINT ( 'NONE',  ( 1.040000000000000924, 0.000000000000000000, 0.000000000000000000 ) ) ;
#23826 = DIRECTION ( 'NONE',  ( 0.000000000000000000, 0.000000000000000000, -1.000000000000000000 ) ) ;
#23828 = ADVANCED_FACE ( 'NONE', ( #21554 ), #8185, .T. ) ;
#23827 = DIRECTION ( 'NONE',  ( 0.000000000000000000, 6.183172785659898852E-15, -1.000000000000000000 ) ) ;
#23829 = VERTEX_POINT ( 'NONE', #370 ) ;
#23830 = ORIENTED_EDGE ( 'NONE', *, *, #458, .F. ) ;
#23831 = CARTESIAN_POINT ( 'NONE',  ( 795.1160410757272530, 1371.734899083927303, 1753.598338701303874 ) ) ;
#23832 = ORIENTED_EDGE ( 'NONE', *, *, #20144, .T. ) ;
#23833 = DIRECTION ( 'NONE',  ( 0.000000000000000000, 0.000000000000000000, -1.000000000000000000 ) ) ;
#23834 = DIRECTION ( 'NONE',  ( 0.000000000000000000, 1.836970198721029441E-16, -1.000000000000000000 ) ) ;
#23835 = AXIS2_PLACEMENT_3D ( 'NONE', #7685, #2178, #20702 ) ;
#23836 = CARTESIAN_POINT ( 'NONE',  ( -365.0000000000000000, -131.0000000000000000, 113.9999999999999858 ) ) ;
#23837 = LINE ( 'NONE', #32198, #22747 ) ;
#23838 = ORIENTED_EDGE ( 'NONE', *, *, #18335, .T. ) ;
#23839 = PLANE ( 'NONE',  #8499 ) ;
#23841 = DIRECTION ( 'NONE',  ( -0.000000000000000000, -0.000000000000000000, -1.000000000000000000 ) ) ;
#23840 = FACE_OUTER_BOUND ( 'NONE', #30839, .T. ) ;
#23842 = VERTEX_POINT ( 'NONE', #24908 ) ;
#23843 = VERTEX_POINT ( 'NONE', #24546 ) ;
#23844 = CARTESIAN_POINT ( 'NONE',  ( 2.765921099433442443, 20.99477179376858871, -22.93149026599722617 ) ) ;
#23845 = ORIENTED_EDGE ( 'NONE', *, *, #29744, .T. ) ;
#23846 = FACE_OUTER_BOUND ( 'NONE', #4631, .T. ) ;
#23847 = DIRECTION ( 'NONE',  ( 0.000000000000000000, 0.9822872507286906085, -0.1873813145857145812 ) ) ;
#23848 = ORIENTED_EDGE ( 'NONE', *, *, #17732, .T. ) ;
#23849 = CARTESIAN_POINT ( 'NONE',  ( 22.89764159710613001, 8.346743312457579833, -77.50000000000000000 ) ) ;
#23850 = DIRECTION ( 'NONE',  ( 0.000000000000000000, 0.000000000000000000, 1.000000000000000000 ) ) ;
#23851 = ORIENTED_EDGE ( 'NONE', *, *, #24709, .F. ) ;
#23852 = CARTESIAN_POINT ( 'NONE',  ( 22.10765473302597073, -16.64466345897532662, -77.50000000000000000 ) ) ;
#23853 = ADVANCED_FACE ( 'NONE', ( #32565 ), #29734, .T. ) ;
#23854 = CARTESIAN_POINT ( 'NONE',  ( -12.00000000000001066, -24.99999999999999289, 154.9999999999999716 ) ) ;
#23856 = DIRECTION ( 'NONE',  ( 1.000000000000000000, 0.000000000000000000, -0.000000000000000000 ) ) ;
#23855 = DIRECTION ( 'NONE',  ( 0.000000000000000000, 0.000000000000000000, 1.000000000000000000 ) ) ;
#23857 = DIRECTION ( 'NONE',  ( 0.000000000000000000, 1.000000000000000000, 0.000000000000000000 ) ) ;
#23858 = DIRECTION ( 'NONE',  ( -1.000000000000000000, -0.000000000000000000, -0.000000000000000000 ) ) ;
#23860 = EDGE_CURVE ( 'NONE', #34805, #23614, #8023, .T. ) ;
#23859 = DIRECTION ( 'NONE',  ( 0.000000000000000000, 0.000000000000000000, 1.000000000000000000 ) ) ;
#23861 = ADVANCED_FACE ( 'NONE', ( #5154 ), #32747, .F. ) ;
#23862 = VERTEX_POINT ( 'NONE', #3020 ) ;
#23863 = EDGE_CURVE ( 'NONE', #1712, #26408, #28187, .T. ) ;
#23864 = EDGE_CURVE ( 'NONE', #27613, #27823, #190, .T. ) ;
#23865 = DIRECTION ( 'NONE',  ( 2.631201909438060269E-14, -5.396010391056495992E-16, 0.9999999999999998890 ) ) ;
#23866 = ORIENTED_EDGE ( 'NONE', *, *, #15312, .F. ) ;
#23867 = ORIENTED_EDGE ( 'NONE', *, *, #11459, .F. ) ;
#23868 = EDGE_CURVE ( 'NONE', #7179, #32232, #543, .T. ) ;
#23869 = DIRECTION ( 'NONE',  ( 0.000000000000000000, -0.000000000000000000, -1.000000000000000000 ) ) ;
#23870 = DIRECTION ( 'NONE',  ( 2.631201909438060585E-14, -5.396010391056496978E-16, 1.000000000000000000 ) ) ;
#23871 = ORIENTED_EDGE ( 'NONE', *, *, #21886, .F. ) ;
#23872 = ORIENTED_EDGE ( 'NONE', *, *, #2644, .F. ) ;
#23873 = CARTESIAN_POINT ( 'NONE',  ( 0.02407890056655695096, 20.99477179376825120, 22.93149026599753526 ) ) ;
#23874 = DIRECTION ( 'NONE',  ( 0.000000000000000000, 1.000000000000000000, 0.000000000000000000 ) ) ;
#23875 = FACE_OUTER_BOUND ( 'NONE', #31783, .T. ) ;
#23876 = CARTESIAN_POINT ( 'NONE',  ( 127.4999999999999147, 0.000000000000000000, 0.000000000000000000 ) ) ;
#23877 = VERTEX_POINT ( 'NONE', #3198 ) ;
#23878 = VERTEX_POINT ( 'NONE', #16047 ) ;
#23879 = CARTESIAN_POINT ( 'NONE',  ( 0.02407890056655781832, 7.350529080603967813, -30.20932655202929595 ) ) ;
#23880 = CARTESIAN_POINT ( 'NONE',  ( 2.789999999999999147, 0.000000000000000000, 0.000000000000000000 ) ) ;
#23881 = LINE ( 'NONE', #2002, #9641 ) ;
#23882 = LINE ( 'NONE', #21404, #5146 ) ;
#23883 = CARTESIAN_POINT ( 'NONE',  ( 10.00000000000000000, -1.505030548027689319, 3.180000000000000160 ) ) ;
#23884 = VERTEX_POINT ( 'NONE', #11393 ) ;
#23885 = DIRECTION ( 'NONE',  ( -0.000000000000000000, -1.000000000000000000, -0.000000000000000000 ) ) ;
#23886 = CARTESIAN_POINT ( 'NONE',  ( 145.0000000000000568, -173.5121282296299796, -41.09364177412887642 ) ) ;
#23887 = DIRECTION ( 'NONE',  ( 1.000000000000000000, 0.000000000000000000, -1.232595164407831220E-32 ) ) ;
#23888 = DIRECTION ( 'NONE',  ( 1.000000000000000000, 0.000000000000000000, 0.000000000000000000 ) ) ;
#23889 = AXIS2_PLACEMENT_3D ( 'NONE', #30016, #5608, #13306 ) ;
#23890 = CARTESIAN_POINT ( 'NONE',  ( 110.5782799041639350, 1.358924363732619600, -7.378408734721662476 ) ) ;
#23892 = DIRECTION ( 'NONE',  ( 0.000000000000000000, 0.000000000000000000, -1.000000000000000000 ) ) ;
#23891 = DIRECTION ( 'NONE',  ( 0.000000000000000000, 0.000000000000000000, -1.000000000000000000 ) ) ;
#23893 = FACE_OUTER_BOUND ( 'NONE', #14504, .T. ) ;
#23894 = ORIENTED_EDGE ( 'NONE', *, *, #7789, .F. ) ;
#23895 = DIRECTION ( 'NONE',  ( 0.000000000000000000, -1.000000000000000000, -2.465190328815662439E-32 ) ) ;
#23897 = CARTESIAN_POINT ( 'NONE',  ( -365.0000000000000000, 132.9999999999999716, 113.9999999999999858 ) ) ;
#23896 = CARTESIAN_POINT ( 'NONE',  ( 3.235562306570555532E-30, -15.68591377522703390, -87.50000000000000000 ) ) ;
#23898 = ORIENTED_EDGE ( 'NONE', *, *, #20387, .T. ) ;
#23899 = ADVANCED_FACE ( 'NONE', ( #5335 ), #7839, .T. ) ;
#23900 = EDGE_CURVE ( 'NONE', #32940, #6803, #5678, .T. ) ;
#23901 = CARTESIAN_POINT ( 'NONE',  ( -8.000000000000000000, 0.000000000000000000, 0.000000000000000000 ) ) ;
#23902 = VECTOR ( 'NONE', #29211, 1000.000000000000000 ) ;
#23903 = ORIENTED_EDGE ( 'NONE', *, *, #6002, .T. ) ;
#23904 = ORIENTED_EDGE ( 'NONE', *, *, #28841, .F. ) ;
#23905 = FACE_BOUND ( 'NONE', #26948, .T. ) ;
#23906 = EDGE_LOOP ( 'NONE', ( #27290, #2772, #31754, #18616, #34902, #22183 ) ) ;
#23907 = EDGE_LOOP ( 'NONE', ( #4111, #23794, #24816, #17080 ) ) ;
#23908 = AXIS2_PLACEMENT_3D ( 'NONE', #34091, #26251, #18259 ) ;
#23909 = LINE ( 'NONE', #23755, #20177 ) ;
#23910 = EDGE_CURVE ( 'NONE', #26015, #22194, #12594, .T. ) ;
#23911 = AXIS2_PLACEMENT_3D ( 'NONE', #27474, #10399, #21258 ) ;
#23912 = CARTESIAN_POINT ( 'NONE',  ( -48.14940018563182633, -31.98399783210736302, 40.89330243838653445 ) ) ;
#23913 = CYLINDRICAL_SURFACE ( 'NONE', #25621, 3.999999999999976019 ) ;
#23914 = ORIENTED_EDGE ( 'NONE', *, *, #9982, .T. ) ;
#23915 = EDGE_LOOP ( 'NONE', ( #7228, #9818, #6482, #8118 ) ) ;
#23916 = CARTESIAN_POINT ( 'NONE',  ( -143.0000000000000568, -90.29102463692673552, -73.95413108702813076 ) ) ;
#23917 = DIRECTION ( 'NONE',  ( 0.000000000000000000, 1.000000000000000000, -6.123233995736766036E-17 ) ) ;
#23918 = DIRECTION ( 'NONE',  ( -1.000000000000000000, -0.000000000000000000, -0.000000000000000000 ) ) ;
#23919 = EDGE_CURVE ( 'NONE', #2852, #34959, #10705, .T. ) ;
#23920 = DIRECTION ( 'NONE',  ( -1.000000000000000000, -0.000000000000000000, -0.000000000000000000 ) ) ;
#23921 = CARTESIAN_POINT ( 'NONE',  ( 27.64943126350854286, -17.16721653852533791, 49.43553178847298568 ) ) ;
#23922 = EDGE_LOOP ( 'NONE', ( #14238, #1747, #23155, #18822 ) ) ;
#23923 = EDGE_CURVE ( 'NONE', #3220, #7946, #13678, .T. ) ;
#23924 = EDGE_CURVE ( 'NONE', #7441, #13039, #27670, .T. ) ;
#23925 = CARTESIAN_POINT ( 'NONE',  ( 2.789999999999999147, 9.869977788041397915, -30.37666815053925973 ) ) ;
#23926 = VECTOR ( 'NONE', #28838, 1000.000000000000000 ) ;
#23927 = CARTESIAN_POINT ( 'NONE',  ( -36.80830595996284416, 8.862931941313773265, 68.31122994652405112 ) ) ;
#23928 = ORIENTED_EDGE ( 'NONE', *, *, #13680, .T. ) ;
#23929 =( GEOMETRIC_REPRESENTATION_CONTEXT ( 3 ) GLOBAL_UNCERTAINTY_ASSIGNED_CONTEXT ( ( #756 ) ) GLOBAL_UNIT_ASSIGNED_CONTEXT ( ( #23264, #4533, #15606 ) ) REPRESENTATION_CONTEXT ( 'NONE', 'WORKASPACE' ) );
#23930 = CARTESIAN_POINT ( 'NONE',  ( 0.02407890056655868569, -8.112136323388726922, -30.01377904834218668 ) ) ;
#23931 = EDGE_CURVE ( 'NONE', #6040, #8267, #10273, .T. ) ;
#23932 = PLANE ( 'NONE',  #26240 ) ;
#23933 = CARTESIAN_POINT ( 'NONE',  ( -410.0000000000000568, 124.9999999999999574, -187.0000000000000000 ) ) ;
#23934 = ORIENTED_EDGE ( 'NONE', *, *, #19862, .T. ) ;
#23935 = DIRECTION ( 'NONE',  ( -1.000000000000000000, -0.000000000000000000, -0.000000000000000000 ) ) ;
#23936 = VERTEX_POINT ( 'NONE', #1417 ) ;
#23937 = CARTESIAN_POINT ( 'NONE',  ( -499.9999999999999432, -105.0000000000000142, -162.9999999999999716 ) ) ;
#23938 = ORIENTED_EDGE ( 'NONE', *, *, #2101, .F. ) ;
#23939 = VECTOR ( 'NONE', #23540, 1000.000000000000000 ) ;
#23940 = DIRECTION ( 'NONE',  ( -1.000000000000000000, 0.000000000000000000, 0.000000000000000000 ) ) ;
#23941 = DIRECTION ( 'NONE',  ( 1.000000000000000000, 0.000000000000000000, 0.000000000000000000 ) ) ;
#23942 = VECTOR ( 'NONE', #11914, 1000.000000000000000 ) ;
#23943 = ORIENTED_EDGE ( 'NONE', *, *, #32382, .T. ) ;
#23944 = ADVANCED_FACE ( 'NONE', ( #8895 ), #30616, .T. ) ;
#23945 = CARTESIAN_POINT ( 'NONE',  ( 2.765921099433441999, -21.56796757982826307, 22.39322359481599278 ) ) ;
#23946 = LINE ( 'NONE', #34827, #22268 ) ;
#23947 = ORIENTED_EDGE ( 'NONE', *, *, #16775, .F. ) ;
#23948 = CIRCLE ( 'NONE', #24524, 2.500000000000002220 ) ;
#23949 = DIRECTION ( 'NONE',  ( -0.1063910735369225230, 0.9943243633099118073, -1.000770725407345128E-14 ) ) ;
#23950 = VECTOR ( 'NONE', #1196, 1000.000000000000000 ) ;
#23952 = VERTEX_POINT ( 'NONE', #1071 ) ;
#23951 = CIRCLE ( 'NONE', #13180, 32.54542015209055705 ) ;
#23953 = LINE ( 'NONE', #32488, #21008 ) ;
#23954 = ORIENTED_EDGE ( 'NONE', *, *, #33828, .F. ) ;
#23955 = DIRECTION ( 'NONE',  ( 1.000000000000000000, 3.469446951954617213E-18, -2.891205793294674875E-16 ) ) ;
#23956 = DIRECTION ( 'NONE',  ( -0.6876994588534233177, 0.7259954919231308423, 0.000000000000000000 ) ) ;
#23957 = CARTESIAN_POINT ( 'NONE',  ( -99.88497961182919482, 9.184690493976639608E-16, -7.500000000000000000 ) ) ;
#23958 = FACE_OUTER_BOUND ( 'NONE', #947, .T. ) ;
#23959 = ORIENTED_EDGE ( 'NONE', *, *, #2532, .T. ) ;
#23960 = ORIENTED_EDGE ( 'NONE', *, *, #6081, .F. ) ;
#23961 = ORIENTED_EDGE ( 'NONE', *, *, #20513, .T. ) ;
#23962 = CARTESIAN_POINT ( 'NONE',  ( -37.69926482250235722, 3.578808500140865156, 68.31122994652405112 ) ) ;
#23963 = CARTESIAN_POINT ( 'NONE',  ( -130.6469666100234406, 6.000000000000000000, 62.49999999999999289 ) ) ;
#23965 = DIRECTION ( 'NONE',  ( 0.000000000000000000, 0.000000000000000000, 1.000000000000000000 ) ) ;
#23964 = AXIS2_PLACEMENT_3D ( 'NONE', #28412, #28585, #6850 ) ;
#23966 = EDGE_CURVE ( 'NONE', #16444, #11612, #14785, .T. ) ;
#23967 = EDGE_CURVE ( 'NONE', #29489, #34521, #22959, .T. ) ;
#23968 = DIRECTION ( 'NONE',  ( 0.000000000000000000, 1.000000000000000000, 0.000000000000000000 ) ) ;
#23969 = CARTESIAN_POINT ( 'NONE',  ( -7.700000000000000178, 0.000000000000000000, 0.000000000000000000 ) ) ;
#23971 = DIRECTION ( 'NONE',  ( 0.2149704402110236556, -0.9766205557100866574, -0.000000000000000000 ) ) ;
#23970 =( REPRESENTATION_RELATIONSHIP ('NONE','NONE', #23037, #15767 ) REPRESENTATION_RELATIONSHIP_WITH_TRANSFORMATION ( #35060 )SHAPE_REPRESENTATION_RELATIONSHIP( ) );
#23972 = LINE ( 'NONE', #29509, #12464 ) ;
#23973 = VERTEX_POINT ( 'NONE', #20291 ) ;
#23974 = DIRECTION ( 'NONE',  ( 0.000000000000000000, 0.000000000000000000, -1.000000000000000000 ) ) ;
#23975 = CARTESIAN_POINT ( 'NONE',  ( 0.02407890056655564992, -30.46391896562411716, 6.211548095912460710 ) ) ;
#23976 = CARTESIAN_POINT ( 'NONE',  ( -35.00000000000000000, -12.29554237047777576, -20.46290632209285576 ) ) ;
#23977 = EDGE_LOOP ( 'NONE', ( #12410, #18252, #26438, #33032, #20679, #34794, #22226, #14761 ) ) ;
#23978 = AXIS2_PLACEMENT_3D ( 'NONE', #26305, #29514, #23643 ) ;
#23979 = CARTESIAN_POINT ( 'NONE',  ( 0.006871066869920603760, 30.78681169157792041, -2.258271426746185195 ) ) ;
#23980 = ORIENTED_EDGE ( 'NONE', *, *, #28029, .T. ) ;
#23981 = COLOUR_RGB ( '',0.7921568627450980005, 0.8196078431372548767, 0.9333333333333333481 ) ;
#23982 = LINE ( 'NONE', #7785, #5780 ) ;
#23983 = CARTESIAN_POINT ( 'NONE',  ( -499.9999999999999432, -137.0000000000000000, -162.9999999999999716 ) ) ;
#23984 = ORIENTED_EDGE ( 'NONE', *, *, #4155, .T. ) ;
#23985 = DIRECTION ( 'NONE',  ( -0.000000000000000000, 1.836970198721029934E-16, -1.000000000000000000 ) ) ;
#23986 = CARTESIAN_POINT ( 'NONE',  ( 2.765921099433441999, -0.3931553186915530129, 31.08824725498900321 ) ) ;
#23987 = DIRECTION ( 'NONE',  ( 0.000000000000000000, -1.000000000000000000, -2.465190328815662439E-32 ) ) ;
#23988 = VERTEX_POINT ( 'NONE', #17637 ) ;
#23989 = EDGE_LOOP ( 'NONE', ( #20388, #9125, #31154, #8375 ) ) ;
#23990 = CARTESIAN_POINT ( 'NONE',  ( 769.8320140383036687, 1216.956872122643517, 1753.598338701303419 ) ) ;
#23991 = EDGE_CURVE ( 'NONE', #21689, #995, #30440, .T. ) ;
#23992 = ORIENTED_EDGE ( 'NONE', *, *, #16687, .F. ) ;
#23993 = CARTESIAN_POINT ( 'NONE',  ( -499.9999999999999432, 112.9999999999999574, -187.0000000000000000 ) ) ;
#23994 = CIRCLE ( 'NONE', #20614, 2.525000000000000355 ) ;
#23995 = PRESENTATION_STYLE_ASSIGNMENT (( #10305 ) ) ;
#23996 = AXIS2_PLACEMENT_3D ( 'NONE', #25161, #17543, #22513 ) ;
#23997 = CARTESIAN_POINT ( 'NONE',  ( -35.55956070192387841, -12.65143121711728291, 10.00000000000000000 ) ) ;
#23998 = DIRECTION ( 'NONE',  ( 1.000000000000000000, 0.000000000000000000, 0.000000000000000000 ) ) ;
#23999 = CONTEXT_DEPENDENT_SHAPE_REPRESENTATION ( #4616, #31400 ) ;
#24000 = VECTOR ( 'NONE', #28421, 1000.000000000000000 ) ;
#24001 = ORIENTED_EDGE ( 'NONE', *, *, #10167, .F. ) ;
#24002 = DIRECTION ( 'NONE',  ( 0.000000000000000000, 0.000000000000000000, 1.000000000000000000 ) ) ;
#24003 = ADVANCED_FACE ( 'NONE', ( #6209 ), #3546, .F. ) ;
#24004 = EDGE_CURVE ( 'NONE', #22962, #22410, #24697, .T. ) ;
#24005 = EDGE_CURVE ( 'NONE', #32629, #26161, #34936, .T. ) ;
#24007 = DIRECTION ( 'NONE',  ( -1.000000000000000000, -0.000000000000000000, -0.000000000000000000 ) ) ;
#24006 = DIRECTION ( 'NONE',  ( 0.000000000000000000, 0.000000000000000000, 1.000000000000000000 ) ) ;
#24008 = ORIENTED_EDGE ( 'NONE', *, *, #24824, .T. ) ;
#24009 = ORIENTED_EDGE ( 'NONE', *, *, #1952, .T. ) ;
#24010 = CARTESIAN_POINT ( 'NONE',  ( 0.5288002521483733398, 5.497007441955001461, 32.93420861807582867 ) ) ;
#24011 = ORIENTED_EDGE ( 'NONE', *, *, #2197, .F. ) ;
#24012 = DIRECTION ( 'NONE',  ( -0.000000000000000000, -1.000000000000000000, -0.000000000000000000 ) ) ;
#24013 = CARTESIAN_POINT ( 'NONE',  ( -365.0000000000000000, -114.9999999999999858, 126.0000000000000000 ) ) ;
#24014 = ORIENTED_EDGE ( 'NONE', *, *, #13712, .T. ) ;
#24015 = DIRECTION ( 'NONE',  ( 0.000000000000000000, -0.8660254037844380415, 0.5000000000000012212 ) ) ;
#24016 = DIRECTION ( 'NONE',  ( -0.000000000000000000, -0.000000000000000000, -1.000000000000000000 ) ) ;
#24017 = ORIENTED_EDGE ( 'NONE', *, *, #15964, .T. ) ;
#24018 = LINE ( 'NONE', #15695, #21491 ) ;
#24019 = DIRECTION ( 'NONE',  ( -0.000000000000000000, 1.836970198721029934E-16, -1.000000000000000000 ) ) ;
#24020 = CARTESIAN_POINT ( 'NONE',  ( 0.7564103431398414568, -1.600050605839945961, -33.87778227150288757 ) ) ;
#24023 = CARTESIAN_POINT ( 'NONE',  ( 2.789999999999999147, 23.28319895603611300, -21.86437915510192909 ) ) ;
#24022 = CYLINDRICAL_SURFACE ( 'NONE', #15088, 3.999999999999976019 ) ;
#24021 = AXIS2_PLACEMENT_3D ( 'NONE', #27767, #8547, #5684 ) ;
#24024 = CONICAL_SURFACE ( 'NONE', #28594, 32.54542015209057126, 1.110254297872109275 ) ;
#24025 = VECTOR ( 'NONE', #24208, 1000.000000000000000 ) ;
#24026 = VECTOR ( 'NONE', #14293, 1000.000000000000000 ) ;
#24027 = LINE ( 'NONE', #7474, #6318 ) ;
#24028 = CARTESIAN_POINT ( 'NONE',  ( 0.000000000000000000, 2.296212748401288367E-15, 47.49999999999999289 ) ) ;
#24029 = LINE ( 'NONE', #21024, #34198 ) ;
#24030 = ORIENTED_EDGE ( 'NONE', *, *, #18898, .F. ) ;
#24031 = DIRECTION ( 'NONE',  ( 0.000000000000000000, -1.000000000000000000, -2.132064625830773463E-16 ) ) ;
#24032 = DIRECTION ( 'NONE',  ( 0.000000000000000000, 0.000000000000000000, 1.000000000000000000 ) ) ;
#24033 = VERTEX_POINT ( 'NONE', #29166 ) ;
#24034 = VERTEX_POINT ( 'NONE', #26312 ) ;
#24035 = AXIS2_PLACEMENT_3D ( 'NONE', #34413, #20881, #31893 ) ;
#24036 = CARTESIAN_POINT ( 'NONE',  ( 110.4189565558304906, 1.924456215511286983, 7.258046499395033102 ) ) ;
#24037 = DIRECTION ( 'NONE',  ( 0.000000000000000000, -1.000000000000000000, 0.000000000000000000 ) ) ;
#24038 = EDGE_CURVE ( 'NONE', #25686, #16360, #12018, .T. ) ;
#24039 = ORIENTED_EDGE ( 'NONE', *, *, #22869, .F. ) ;
#24040 = CARTESIAN_POINT ( 'NONE',  ( -445.9999999999999432, -105.0000000000000142, -101.9999999999999858 ) ) ;
#24041 = CARTESIAN_POINT ( 'NONE',  ( -9.978866888775733912, -13.65249191622732816, -67.50000000000000000 ) ) ;
#24042 = ADVANCED_FACE ( 'NONE', ( #15304 ), #4761, .F. ) ;
#24044 = AXIS2_PLACEMENT_3D ( 'NONE', #34688, #26847, #13340 ) ;
#24043 = CONTEXT_DEPENDENT_SHAPE_REPRESENTATION ( #20151, #28135 ) ;
#24045 = DIRECTION ( 'NONE',  ( 0.000000000000000000, 0.000000000000000000, 1.000000000000000000 ) ) ;
#24046 = ORIENTED_EDGE ( 'NONE', *, *, #12425, .F. ) ;
#24047 = ORIENTED_EDGE ( 'NONE', *, *, #19077, .T. ) ;
#24048 = CIRCLE ( 'NONE', #8718, 7.999999999999979572 ) ;
#24049 = DIRECTION ( 'NONE',  ( -0.000000000000000000, -0.000000000000000000, 1.000000000000000000 ) ) ;
#24050 = CARTESIAN_POINT ( 'NONE',  ( -0.9727285265192152641, -1.747512292859696670, -0.7500000000000000000 ) ) ;
#24051 = ADVANCED_FACE ( 'NONE', ( #31649 ), #23138, .T. ) ;
#24052 = DIRECTION ( 'NONE',  ( -1.000000000000000000, -0.000000000000000000, 0.000000000000000000 ) ) ;
#24053 = LINE ( 'NONE', #34577, #17125 ) ;
#24054 = CARTESIAN_POINT ( 'NONE',  ( -430.0000000000000000, 118.9999999999999716, 126.0000000000000000 ) ) ;
#24055 = ORIENTED_EDGE ( 'NONE', *, *, #4235, .T. ) ;
#24056 = DIRECTION ( 'NONE',  ( 1.000000000000000000, 3.040835319149746090E-31, 1.232595164407830946E-32 ) ) ;
#24057 = DIRECTION ( 'NONE',  ( 0.000000000000000000, 2.309213040847544338E-50, 1.000000000000000000 ) ) ;
#24058 = CARTESIAN_POINT ( 'NONE',  ( -19.99999999999998934, -105.0000000000000142, 187.0000000000000000 ) ) ;
#24059 = ADVANCED_FACE ( 'NONE', ( #26137 ), #10122, .F. ) ;
#24060 = CARTESIAN_POINT ( 'NONE',  ( 25.76952721012208158, 19.87802405277947315, 68.31122994652405112 ) ) ;
#24061 = DIRECTION ( 'NONE',  ( 0.000000000000000000, 0.000000000000000000, -1.000000000000000000 ) ) ;
#24062 = EDGE_CURVE ( 'NONE', #6872, #13784, #16569, .T. ) ;
#24063 = ADVANCED_FACE ( 'NONE', ( #7433 ), #34148, .T. ) ;
#24064 = CARTESIAN_POINT ( 'NONE',  ( -145.0000000000000568, -97.56119630548165844, -180.0000000000000000 ) ) ;
#24066 = DIRECTION ( 'NONE',  ( -3.040835319149746528E-31, -1.000000000000000000, 0.000000000000000000 ) ) ;
#24065 = PLANE ( 'NONE',  #9361 ) ;
#24067 = CIRCLE ( 'NONE', #25213, 1.799999999999999600 ) ;
#24068 = CARTESIAN_POINT ( 'NONE',  ( -12.00000000000001066, -124.9999999999999432, -154.9999999999999716 ) ) ;
#24069 = ORIENTED_EDGE ( 'NONE', *, *, #32190, .T. ) ;
#24070 = CYLINDRICAL_SURFACE ( 'NONE', #33184, 2.000000000000001776 ) ;
#24072 = FACE_OUTER_BOUND ( 'NONE', #23346, .T. ) ;
#24071 = DIRECTION ( 'NONE',  ( 0.000000000000000000, 1.000000000000000000, 2.309213040847544338E-50 ) ) ;
#24073 = AXIS2_PLACEMENT_3D ( 'NONE', #9572, #12428, #23275 ) ;
#24075 = VERTEX_POINT ( 'NONE', #4943 ) ;
#24074 = AXIS2_PLACEMENT_3D ( 'NONE', #8453, #14160, #32650 ) ;
#24076 = CIRCLE ( 'NONE', #237, 8.000000000000000000 ) ;
#24077 = FACE_OUTER_BOUND ( 'NONE', #24633, .T. ) ;
#24078 = PRODUCT_DEFINITION_SHAPE ( 'NONE', 'NONE',  #35199 ) ;
#24079 = ORIENTED_EDGE ( 'NONE', *, *, #17597, .F. ) ;
#24080 = ORIENTED_EDGE ( 'NONE', *, *, #21700, .T. ) ;
#24081 = FACE_BOUND ( 'NONE', #6565, .T. ) ;
#24082 = ORIENTED_EDGE ( 'NONE', *, *, #5677, .T. ) ;
#24083 = ORIENTED_EDGE ( 'NONE', *, *, #12540, .T. ) ;
#24084 = FACE_OUTER_BOUND ( 'NONE', #4868, .T. ) ;
#24085 = AXIS2_PLACEMENT_3D ( 'NONE', #3821, #9869, #4340 ) ;
#24086 = DIRECTION ( 'NONE',  ( -1.000000000000000000, -0.000000000000000000, -0.000000000000000000 ) ) ;
#24087 = CARTESIAN_POINT ( 'NONE',  ( -418.0000000000000000, -124.9999999999999716, 132.0000000000000000 ) ) ;
#24088 = ORIENTED_EDGE ( 'NONE', *, *, #3893, .F. ) ;
#24089 = ORIENTED_EDGE ( 'NONE', *, *, #9336, .F. ) ;
#24090 = FACE_OUTER_BOUND ( 'NONE', #2244, .T. ) ;
#24091 = CIRCLE ( 'NONE', #17886, 2.033421858999711951 ) ;
#24092 = ADVANCED_FACE ( 'NONE', ( #15836 ), #26667, .T. ) ;
#24093 = DIRECTION ( 'NONE',  ( -1.000000000000000000, 0.000000000000000000, -0.000000000000000000 ) ) ;
#24094 = CARTESIAN_POINT ( 'NONE',  ( 60.00000000000000000, -33.69708579775584667, -49.43553178847298568 ) ) ;
#24095 = VERTEX_POINT ( 'NONE', #20982 ) ;
#24096 = ORIENTED_EDGE ( 'NONE', *, *, #32779, .F. ) ;
#24097 = DIRECTION ( 'NONE',  ( -0.000000000000000000, -1.000000000000000000, -0.000000000000000000 ) ) ;
#24098 = TOROIDAL_SURFACE ( 'NONE', #16150, 30.47050528711512030, 8.000000000000000000 ) ;
#24099 = ADVANCED_FACE ( 'NONE', ( #12980 ), #9607, .F. ) ;
#24100 = ADVANCED_FACE ( 'NONE', ( #4576 ), #20461, .F. ) ;
#24101 = CIRCLE ( 'NONE', #6500, 2.524999999999999467 ) ;
#24102 = CARTESIAN_POINT ( 'NONE',  ( 1.040000000000000924, 0.000000000000000000, 0.000000000000000000 ) ) ;
#24103 = ORIENTED_EDGE ( 'NONE', *, *, #22258, .F. ) ;
#24104 = AXIS2_PLACEMENT_3D ( 'NONE', #29787, #2727, #2550 ) ;
#24105 = CARTESIAN_POINT ( 'NONE',  ( -20.63749999999999929, 0.000000000000000000, 0.000000000000000000 ) ) ;
#24106 = CYLINDRICAL_SURFACE ( 'NONE', #8076, 7.500000000000000000 ) ;
#24107 = CARTESIAN_POINT ( 'NONE',  ( 2.261199753130818113, -9.581412748858477713, 31.98555481955049729 ) ) ;
#24108 = ORIENTED_EDGE ( 'NONE', *, *, #31402, .T. ) ;
#24109 = DIRECTION ( 'NONE',  ( 1.000000000000000000, -0.000000000000000000, 0.000000000000000000 ) ) ;
#24110 = VERTEX_POINT ( 'NONE', #15480 ) ;
#24111 = CARTESIAN_POINT ( 'NONE',  ( -21.67835495107042476, 31.04982069277122747, 68.31122994652405112 ) ) ;
#24112 = ORIENTED_EDGE ( 'NONE', *, *, #3849, .F. ) ;
#24113 = CARTESIAN_POINT ( 'NONE',  ( 0.02407890056655738464, 26.03801215795517621, 16.98986790278620873 ) ) ;
#24114 = LINE ( 'NONE', #2584, #5147 ) ;
#24115 = EDGE_CURVE ( 'NONE', #16456, #10877, #30187, .T. ) ;
#24116 = VECTOR ( 'NONE', #2730, 1000.000000000000000 ) ;
#24117 = ORIENTED_EDGE ( 'NONE', *, *, #25456, .F. ) ;
#24118 = DIRECTION ( 'NONE',  ( 0.000000000000000000, 0.000000000000000000, 1.000000000000000000 ) ) ;
#24119 = FACE_OUTER_BOUND ( 'NONE', #22466, .T. ) ;
#24120 = VECTOR ( 'NONE', #33259, 1000.000000000000000 ) ;
#24121 = EDGE_CURVE ( 'NONE', #24780, #33691, #23650, .T. ) ;
#24122 = ORIENTED_EDGE ( 'NONE', *, *, #29744, .F. ) ;
#24123 = DIRECTION ( 'NONE',  ( 0.000000000000000000, 1.000000000000000000, 5.053935297177146739E-49 ) ) ;
#24124 = EDGE_CURVE ( 'NONE', #22483, #11290, #33021, .T. ) ;
#24125 = CIRCLE ( 'NONE', #22444, 2.524999999999999467 ) ;
#24126 = EDGE_CURVE ( 'NONE', #13256, #13866, #8198, .T. ) ;
#24127 = DIRECTION ( 'NONE',  ( -7.893486629456754622E-14, 1.675393697758169048E-15, 1.000000000000000000 ) ) ;
#24128 = ORIENTED_EDGE ( 'NONE', *, *, #2432, .T. ) ;
#24129 = CARTESIAN_POINT ( 'NONE',  ( -107.1458265010192861, 4.646131333787441697, 5.888157618374225244 ) ) ;
#24130 = VERTEX_POINT ( 'NONE', #2801 ) ;
#24131 = DIRECTION ( 'NONE',  ( -0.000000000000000000, -0.000000000000000000, -1.000000000000000000 ) ) ;
#24132 = AXIS2_PLACEMENT_3D ( 'NONE', #27903, #27205, #30059 ) ;
#24133 =( NAMED_UNIT ( * ) PLANE_ANGLE_UNIT ( ) SI_UNIT ( $, .RADIAN. ) );
#24134 = CARTESIAN_POINT ( 'NONE',  ( -109.4154700880919080, -2.602876666701938291, -7.039998176148507092 ) ) ;
#24135 = FACE_OUTER_BOUND ( 'NONE', #2165, .T. ) ;
#24136 = ORIENTED_EDGE ( 'NONE', *, *, #12983, .T. ) ;
#24137 = ORIENTED_EDGE ( 'NONE', *, *, #31930, .F. ) ;
#24138 = ORIENTED_EDGE ( 'NONE', *, *, #23003, .F. ) ;
#24139 = CARTESIAN_POINT ( 'NONE',  ( 127.4999999999999147, 0.000000000000000000, 12.50000000000000000 ) ) ;
#24140 = FACE_OUTER_BOUND ( 'NONE', #5484, .T. ) ;
#24141 = DIRECTION ( 'NONE',  ( 1.000000000000000000, 0.000000000000000000, 0.000000000000000000 ) ) ;
#24142 = VECTOR ( 'NONE', #15898, 1000.000000000000000 ) ;
#24143 = LINE ( 'NONE', #21316, #3114 ) ;
#24144 = FACE_OUTER_BOUND ( 'NONE', #22832, .T. ) ;
#24145 = EDGE_CURVE ( 'NONE', #980, #707, #35045, .T. ) ;
#24146 = EDGE_CURVE ( 'NONE', #1315, #34034, #29063, .T. ) ;
#24147 = DIRECTION ( 'NONE',  ( -0.000000000000000000, -2.465190328815661892E-32, -1.000000000000000000 ) ) ;
#24148 = CARTESIAN_POINT ( 'NONE',  ( -430.0000000000000000, -119.0000000000000000, 126.0000000000000000 ) ) ;
#24149 = ORIENTED_EDGE ( 'NONE', *, *, #25448, .T. ) ;
#24150 = VECTOR ( 'NONE', #10638, 1000.000000000000000 ) ;
#24151 = CARTESIAN_POINT ( 'NONE',  ( 0.02407890056655651728, 18.59128259035506758, -24.91982945642901726 ) ) ;
#24152 = FACE_OUTER_BOUND ( 'NONE', #4442, .T. ) ;
#24153 = EDGE_CURVE ( 'NONE', #8593, #22052, #16183, .T. ) ;
#24154 = DIRECTION ( 'NONE',  ( 0.000000000000000000, 1.836970198721029688E-16, -1.000000000000000000 ) ) ;
#24155 = ORIENTED_EDGE ( 'NONE', *, *, #7340, .T. ) ;
#24156 = CIRCLE ( 'NONE', #25871, 14.19999999999999929 ) ;
#24157 = VECTOR ( 'NONE', #11394, 1000.000000000000227 ) ;
#24158 = DIRECTION ( 'NONE',  ( 0.000000000000000000, 1.000000000000000000, 0.000000000000000000 ) ) ;
#24159 = ORIENTED_EDGE ( 'NONE', *, *, #9533, .T. ) ;
#24161 = CLOSED_SHELL ( 'NONE', ( #5317, #12418, #17653, #20771, #16845, #16244, #15760, #21531, #20968, #33419, #18734, #23899, #15605, #24342, #33685, #4165, #16820, #26686, #33012, #32091, #2198, #9247, #10531, #13075, #28212, #23092, #21692 ) ) ;
#24160 = CARTESIAN_POINT ( 'NONE',  ( -106.6598137192883939, 4.841160850826504713, -11.52458411820204454 ) ) ;
#24162 = DIRECTION ( 'NONE',  ( -0.000000000000000000, 0.000000000000000000, 1.000000000000000000 ) ) ;
#24163 = ORIENTED_EDGE ( 'NONE', *, *, #22501, .T. ) ;
#24164 = DIRECTION ( 'NONE',  ( 0.000000000000000000, 1.374038396813312784E-15, -1.000000000000000000 ) ) ;
#24165 = DIRECTION ( 'NONE',  ( 0.000000000000000000, 1.000000000000000000, -3.374343856708137958E-53 ) ) ;
#24166 = CARTESIAN_POINT ( 'NONE',  ( 10.00000000000000000, 0.000000000000000000, 0.000000000000000000 ) ) ;
#24167 = ORIENTED_EDGE ( 'NONE', *, *, #28479, .T. ) ;
#24168 = EDGE_CURVE ( 'NONE', #2999, #28220, #13154, .T. ) ;
#24169 = EDGE_CURVE ( 'NONE', #19146, #34985, #21850, .T. ) ;
#24170 = VECTOR ( 'NONE', #13647, 1000.000000000000000 ) ;
#24171 = ORIENTED_EDGE ( 'NONE', *, *, #22022, .T. ) ;
#24172 = CARTESIAN_POINT ( 'NONE',  ( 770.1747490121555302, 1367.713053646422850, 1753.598338701303646 ) ) ;
#24173 = VECTOR ( 'NONE', #34235, 1000.000000000000114 ) ;
#24174 = CARTESIAN_POINT ( 'NONE',  ( 22.10765473302597073, -16.64466345897532307, -87.50000000000000000 ) ) ;
#24175 = EDGE_LOOP ( 'NONE', ( #30351, #5621, #6789, #21712 ) ) ;
#24176 = VECTOR ( 'NONE', #26776, 1000.000000000000000 ) ;
#24177 = PLANE ( 'NONE',  #14103 ) ;
#24178 = EDGE_CURVE ( 'NONE', #6460, #24468, #17184, .T. ) ;
#24179 =( LENGTH_UNIT ( ) NAMED_UNIT ( * ) SI_UNIT ( .MILLI., .METRE. ) );
#24180 = CARTESIAN_POINT ( 'NONE',  ( 145.0000000000000568, -90.42893218813456713, 44.81798139211241505 ) ) ;
#24181 = CARTESIAN_POINT ( 'NONE',  ( -41.91768190017683793, 16.36789378607383583, -36.69384042039221328 ) ) ;
#24182 = ITEM_DEFINED_TRANSFORMATION ( 'NONE', 'NONE', #5823,  #28566 ) ;
#24183 =( REPRESENTATION_RELATIONSHIP ('NONE','NONE', #23037, #15767 ) REPRESENTATION_RELATIONSHIP_WITH_TRANSFORMATION ( #20473 )SHAPE_REPRESENTATION_RELATIONSHIP( ) );
#24185 = EDGE_CURVE ( 'NONE', #11691, #8132, #5814, .T. ) ;
#24184 = ORIENTED_EDGE ( 'NONE', *, *, #24443, .F. ) ;
#24186 = DIRECTION ( 'NONE',  ( 0.000000000000000000, 0.000000000000000000, -1.000000000000000000 ) ) ;
#24187 = VECTOR ( 'NONE', #19113, 1000.000000000000114 ) ;
#24188 = CARTESIAN_POINT ( 'NONE',  ( -442.0000000000000000, -125.0000000000000000, -105.9999999999999574 ) ) ;
#24189 = VERTEX_POINT ( 'NONE', #8145 ) ;
#24190 = ORIENTED_EDGE ( 'NONE', *, *, #28764, .F. ) ;
#24191 = LINE ( 'NONE', #32207, #8351 ) ;
#24192 = EDGE_LOOP ( 'NONE', ( #25898, #28620, #6679, #31939 ) ) ;
#24193 = DIRECTION ( 'NONE',  ( 0.000000000000000000, 1.000000000000000000, 0.000000000000000000 ) ) ;
#24194 = CARTESIAN_POINT ( 'NONE',  ( 2.789999999999999147, -0.3931553186911057041, -31.08824725498900676 ) ) ;
#24195 = ORIENTED_EDGE ( 'NONE', *, *, #26483, .T. ) ;
#24196 = VECTOR ( 'NONE', #24800, 1000.000000000000000 ) ;
#24197 = DIRECTION ( 'NONE',  ( -1.000000000000000000, -0.000000000000000000, -0.000000000000000000 ) ) ;
#24198 = FACE_OUTER_BOUND ( 'NONE', #29980, .T. ) ;
#24199 = ORIENTED_EDGE ( 'NONE', *, *, #13471, .T. ) ;
#24200 = ADVANCED_FACE ( 'NONE', ( #2977 ), #13500, .T. ) ;
#24201 = VECTOR ( 'NONE', #5931, 1000.000000000000000 ) ;
#24202 = DIRECTION ( 'NONE',  ( 0.000000000000000000, -1.000000000000000000, 6.123233995736766036E-17 ) ) ;
#24203 = DIRECTION ( 'NONE',  ( 0.000000000000000000, 1.836970198721029441E-16, -1.000000000000000000 ) ) ;
#24204 = DIRECTION ( 'NONE',  ( -0.000000000000000000, -1.836970198721029688E-16, 1.000000000000000000 ) ) ;
#24205 = CARTESIAN_POINT ( 'NONE',  ( -31.87924797510909869, -6.551177101682124970, 68.31122994652405112 ) ) ;
#24206 = CARTESIAN_POINT ( 'NONE',  ( -10.00000000000000000, 0.000000000000000000, 0.000000000000000000 ) ) ;
#24207 = LINE ( 'NONE', #35086, #13359 ) ;
#24208 = DIRECTION ( 'NONE',  ( -1.000000000000000000, 0.000000000000000000, 0.000000000000000000 ) ) ;
#24209 = VECTOR ( 'NONE', #11760, 1000.000000000000000 ) ;
#24210 = EDGE_CURVE ( 'NONE', #9452, #6968, #33049, .T. ) ;
#24211 = EDGE_CURVE ( 'NONE', #15708, #23824, #21674, .T. ) ;
#24212 = ADVANCED_FACE ( 'NONE', ( #27192 ), #19203, .F. ) ;
#24213 = ORIENTED_EDGE ( 'NONE', *, *, #31545, .F. ) ;
#24214 = CARTESIAN_POINT ( 'NONE',  ( 2.789999999999999147, -22.61000311763359250, 20.38038735157074655 ) ) ;
#24215 = DIRECTION ( 'NONE',  ( -0.4744971090113305756, -0.8802570610565357834, -2.839999580434951552E-15 ) ) ;
#24216 = PRODUCT_DEFINITION_CONTEXT ( 'detailed design', #33968, 'design' ) ;
#24217 = ORIENTED_EDGE ( 'NONE', *, *, #30594, .T. ) ;
#24218 = ORIENTED_EDGE ( 'NONE', *, *, #19345, .F. ) ;
#24219 = AXIS2_PLACEMENT_3D ( 'NONE', #22103, #5882, #27608 ) ;
#24220 = DIRECTION ( 'NONE',  ( 0.000000000000000000, 3.435095992033281961E-15, -1.000000000000000000 ) ) ;
#24221 = APPLICATION_PROTOCOL_DEFINITION ( 'draft international standard', 'automotive_design', 1998, #22376 ) ;
#24222 = ORIENTED_EDGE ( 'NONE', *, *, #32251, .T. ) ;
#24223 = CARTESIAN_POINT ( 'NONE',  ( -145.0000000000000568, -12.50000000000001066, 1.224646799147353217E-14 ) ) ;
#24224 = VECTOR ( 'NONE', #32508, 1000.000000000000000 ) ;
#24225 = DIRECTION ( 'NONE',  ( 1.000000000000000000, 0.000000000000000000, -0.000000000000000000 ) ) ;
#24226 = ITEM_DEFINED_TRANSFORMATION ( 'NONE', 'NONE', #28077,  #28566 ) ;
#24227 = FACE_BOUND ( 'NONE', #28322, .T. ) ;
#24228 = ORIENTED_EDGE ( 'NONE', *, *, #13468, .T. ) ;
#24229 = VERTEX_POINT ( 'NONE', #5470 ) ;
#24230 = CARTESIAN_POINT ( 'NONE',  ( 0.07098930855017421271, 4.557722287734508271, -31.36513882472102210 ) ) ;
#24231 = CARTESIAN_POINT ( 'NONE',  ( 2.789999999999999147, -31.05158812718222450, 1.559667679918499417 ) ) ;
#24232 = AXIS2_PLACEMENT_3D ( 'NONE', #24421, #52, #10747 ) ;
#24233 = DIRECTION ( 'NONE',  ( 0.000000000000000000, 0.000000000000000000, -1.000000000000000000 ) ) ;
#24234 = DIRECTION ( 'NONE',  ( 0.000000000000000000, 0.000000000000000000, 1.000000000000000000 ) ) ;
#24235 = DIRECTION ( 'NONE',  ( 1.000000000000000000, 0.000000000000000000, 1.300283923313630633E-47 ) ) ;
#24236 = ORIENTED_EDGE ( 'NONE', *, *, #33174, .F. ) ;
#24237 = DIRECTION ( 'NONE',  ( 0.000000000000000000, 0.000000000000000000, -1.000000000000000000 ) ) ;
#24238 = DIRECTION ( 'NONE',  ( -1.848892746611746419E-32, -6.842277657836020854E-49, 1.000000000000000000 ) ) ;
#24239 = DIRECTION ( 'NONE',  ( 1.000000000000000000, 0.000000000000000000, 0.000000000000000000 ) ) ;
#24240 = DIRECTION ( 'NONE',  ( 0.000000000000000000, 0.000000000000000000, -1.000000000000000000 ) ) ;
#24241 = AXIS2_PLACEMENT_3D ( 'NONE', #25996, #7117, #28840 ) ;
#24242 = DIRECTION ( 'NONE',  ( -3.469446951953832974E-18, -1.000000000000000000, 7.888609052210118054E-31 ) ) ;
#24243 = DIRECTION ( 'NONE',  ( 0.000000000000000000, 0.000000000000000000, -1.000000000000000000 ) ) ;
#24245 = CARTESIAN_POINT ( 'NONE',  ( -99.88497961182919482, 9.184690493976639608E-16, -7.500000000000000000 ) ) ;
#24244 = CARTESIAN_POINT ( 'NONE',  ( -5.021133111224886036, 4.168562732279004202, -67.50000000000000000 ) ) ;
#24246 = AXIS2_PLACEMENT_3D ( 'NONE', #6727, #25595, #22765 ) ;
#24247 = DIRECTION ( 'NONE',  ( 1.000000000000000000, 0.000000000000000000, 0.000000000000000000 ) ) ;
#24248 = VERTEX_POINT ( 'NONE', #22034 ) ;
#24249 = LINE ( 'NONE', #5721, #32082 ) ;
#24250 = DIRECTION ( 'NONE',  ( 0.000000000000000000, 3.374343856708137958E-53, -1.000000000000000000 ) ) ;
#24251 = EDGE_CURVE ( 'NONE', #25357, #28489, #3504, .T. ) ;
#24252 = EDGE_CURVE ( 'NONE', #7193, #34878, #12073, .T. ) ;
#24253 = ORIENTED_EDGE ( 'NONE', *, *, #20572, .F. ) ;
#24254 = AXIS2_PLACEMENT_3D ( 'NONE', #17774, #20437, #25944 ) ;
#24255 = EDGE_CURVE ( 'NONE', #1478, #29515, #27363, .T. ) ;
#24256 = VERTEX_POINT ( 'NONE', #30210 ) ;
#24257 = VERTEX_POINT ( 'NONE', #2277 ) ;
#24258 = DIRECTION ( 'NONE',  ( 0.000000000000000000, -1.000000000000000000, -2.132064625830773463E-16 ) ) ;
#24259 = ORIENTED_EDGE ( 'NONE', *, *, #21653, .T. ) ;
#24260 = EDGE_LOOP ( 'NONE', ( #3160, #3495, #31186, #19333, #3141, #24725 ) ) ;
#24261 = LINE ( 'NONE', #29790, #27533 ) ;
#24262 = ADVANCED_FACE ( 'NONE', ( #34869 ), #10481, .F. ) ;
#24263 = VECTOR ( 'NONE', #23810, 1000.000000000000000 ) ;
#24264 = AXIS2_PLACEMENT_3D ( 'NONE', #3579, #14466, #25298 ) ;
#24265 = DIRECTION ( 'NONE',  ( -0.2149704402110236556, -0.9766205557100866574, 0.000000000000000000 ) ) ;
#24266 = DIRECTION ( 'NONE',  ( -1.000000000000000000, -0.000000000000000000, -0.000000000000000000 ) ) ;
#24267 = ORIENTED_EDGE ( 'NONE', *, *, #22391, .T. ) ;
#24268 = ORIENTED_EDGE ( 'NONE', *, *, #13615, .T. ) ;
#24269 = LINE ( 'NONE', #21440, #2599 ) ;
#24270 = DIRECTION ( 'NONE',  ( -1.000000000000000000, 0.000000000000000000, 0.000000000000000000 ) ) ;
#24271 = CARTESIAN_POINT ( 'NONE',  ( -35.00000000000000000, -4.831299144296466785, 15.81122994652406355 ) ) ;
#24272 = DIRECTION ( 'NONE',  ( 0.000000000000000000, 1.000000000000000000, 5.145227585319922065E-49 ) ) ;
#24273 = ORIENTED_EDGE ( 'NONE', *, *, #32454, .T. ) ;
#24274 = VECTOR ( 'NONE', #6503, 1000.000000000000000 ) ;
#24275 = CARTESIAN_POINT ( 'NONE',  ( -1.307386931792819285, 32.51914993179681090, -36.68877005347593467 ) ) ;
#24276 = DIRECTION ( 'NONE',  ( 1.000000000000000000, 0.000000000000000000, 0.000000000000000000 ) ) ;
#24277 = ORIENTED_EDGE ( 'NONE', *, *, #4625, .F. ) ;
#24278 = DIRECTION ( 'NONE',  ( -0.2675283385292199778, 0.9635499925192232418, 1.770012621235684061E-16 ) ) ;
#24279 = FACE_OUTER_BOUND ( 'NONE', #16153, .T. ) ;
#24280 = FACE_OUTER_BOUND ( 'NONE', #12134, .T. ) ;
#24281 = CARTESIAN_POINT ( 'NONE',  ( 3.235562306570555532E-30, 14.09580098603202458, -67.50000000000000000 ) ) ;
#24282 = CARTESIAN_POINT ( 'NONE',  ( -0.2989565185775304723, 0.000000000000000000, 0.000000000000000000 ) ) ;
#24283 = CARTESIAN_POINT ( 'NONE',  ( -7.218132304338721994, -1.866624223957557671, 4.679999999999999716 ) ) ;
#24284 = ORIENTED_EDGE ( 'NONE', *, *, #31300, .F. ) ;
#24286 = CARTESIAN_POINT ( 'NONE',  ( 37.86520737902618805, 0.5181781365365116798, 68.31122994652405112 ) ) ;
#24285 = DIRECTION ( 'NONE',  ( 1.000000000000000000, 0.000000000000000000, -1.232595164407831220E-32 ) ) ;
#24287 = DIRECTION ( 'NONE',  ( 0.000000000000000000, 0.000000000000000000, 1.000000000000000000 ) ) ;
#24288 = EDGE_CURVE ( 'NONE', #26055, #15405, #16004, .T. ) ;
#24289 = CIRCLE ( 'NONE', #3842, 4.750000000000004441 ) ;
#24290 = EDGE_LOOP ( 'NONE', ( #11100, #15116, #16327, #3530 ) ) ;
#24291 = CARTESIAN_POINT ( 'NONE',  ( 2.033589663287954430, 27.74660763222603066, 19.50359089280082614 ) ) ;
#24292 = ADVANCED_FACE ( 'NONE', ( #851 ), #6528, .F. ) ;
#24293 = EDGE_CURVE ( 'NONE', #22621, #9284, #22383, .T. ) ;
#24294 = ORIENTED_EDGE ( 'NONE', *, *, #19572, .T. ) ;
#24295 = AXIS2_PLACEMENT_3D ( 'NONE', #7725, #29624, #21784 ) ;
#24296 = EDGE_CURVE ( 'NONE', #9411, #18417, #2938, .T. ) ;
#24297 = ADVANCED_FACE ( 'NONE', ( #11359 ), #6169, .T. ) ;
#24298 = ORIENTED_EDGE ( 'NONE', *, *, #21552, .T. ) ;
#24299 = CYLINDRICAL_SURFACE ( 'NONE', #7797, 1.649999999999999467 ) ;
#24300 = DIRECTION ( 'NONE',  ( 0.1081190184239419622, -0.9941379571543595972, 0.000000000000000000 ) ) ;
#24301 = ORIENTED_EDGE ( 'NONE', *, *, #11401, .F. ) ;
#24302 = ORIENTED_EDGE ( 'NONE', *, *, #26634, .F. ) ;
#24303 = CARTESIAN_POINT ( 'NONE',  ( -365.0000000000000000, 130.9999999999999716, 113.9999999999999858 ) ) ;
#24304 = EDGE_CURVE ( 'NONE', #7139, #14417, #24528, .T. ) ;
#24305 = CARTESIAN_POINT ( 'NONE',  ( -361.0000000000000000, -125.0000000000000284, 128.0000000000000000 ) ) ;
#24306 = AXIS2_PLACEMENT_3D ( 'NONE', #23709, #4471, #26551 ) ;
#24307 = CARTESIAN_POINT ( 'NONE',  ( -109.9748806441469924, -1.201525761660785951, -7.405089084531744525 ) ) ;
#24308 = CYLINDRICAL_SURFACE ( 'NONE', #17679, 1.649999999999999911 ) ;
#24309 = ORIENTED_EDGE ( 'NONE', *, *, #11782, .T. ) ;
#24310 = ORIENTED_EDGE ( 'NONE', *, *, #2472, .T. ) ;
#24311 = VERTEX_POINT ( 'NONE', #33410 ) ;
#24312 = DIRECTION ( 'NONE',  ( 0.000000000000000000, 0.000000000000000000, 1.000000000000000000 ) ) ;
#24313 = DIRECTION ( 'NONE',  ( 0.000000000000000000, 0.000000000000000000, 1.000000000000000000 ) ) ;
#24314 = EDGE_CURVE ( 'NONE', #21613, #29231, #17428, .T. ) ;
#24315 = LINE ( 'NONE', #13331, #26738 ) ;
#24316 = VECTOR ( 'NONE', #18710, 1000.000000000000000 ) ;
#24317 = VECTOR ( 'NONE', #1079, 1000.000000000000000 ) ;
#24318 = DIRECTION ( 'NONE',  ( 0.000000000000000000, 0.000000000000000000, 1.000000000000000000 ) ) ;
#24319 = LINE ( 'NONE', #5270, #29031 ) ;
#24320 = DIRECTION ( 'NONE',  ( -1.000000000000000000, 0.000000000000000000, 0.000000000000000000 ) ) ;
#24321 = DIRECTION ( 'NONE',  ( -0.2675283385292215321, -0.9635499925192227977, -0.000000000000000000 ) ) ;
#24322 = ORIENTED_EDGE ( 'NONE', *, *, #13965, .F. ) ;
#24323 = CARTESIAN_POINT ( 'NONE',  ( -20.00000000000004619, -124.9999999999999432, -162.9999999999999432 ) ) ;
#24324 = DIRECTION ( 'NONE',  ( 0.000000000000000000, 0.000000000000000000, 1.000000000000000000 ) ) ;
#24325 = VECTOR ( 'NONE', #1820, 1000.000000000000000 ) ;
#24326 = DIRECTION ( 'NONE',  ( -1.000000000000000000, 0.000000000000000000, -1.292961597001347186E-16 ) ) ;
#24327 = EDGE_LOOP ( 'NONE', ( #16807, #28955, #3132, #7960 ) ) ;
#24328 = DIRECTION ( 'NONE',  ( 0.000000000000000000, 1.000000000000000000, 0.000000000000000000 ) ) ;
#24329 = ORIENTED_EDGE ( 'NONE', *, *, #21025, .F. ) ;
#24330 = CARTESIAN_POINT ( 'NONE',  ( -499.9999999999999432, 136.9999999999999432, -187.0000000000000000 ) ) ;
#24331 = AXIS2_PLACEMENT_3D ( 'NONE', #23163, #15329, #26159 ) ;
#24332 = DIRECTION ( 'NONE',  ( 0.000000000000000000, 1.836970198721029688E-16, -1.000000000000000000 ) ) ;
#24333 = CIRCLE ( 'NONE', #27750, 34.41491905851385269 ) ;
#24334 = ORIENTED_EDGE ( 'NONE', *, *, #7533, .F. ) ;
#24335 = CARTESIAN_POINT ( 'NONE',  ( -12.00000000000001066, 144.9999999999999716, -162.9999999999999432 ) ) ;
#24336 = CARTESIAN_POINT ( 'NONE',  ( 127.4999999999999147, 1.530808498934191521E-15, -12.50000000000000000 ) ) ;
#24337 = DIRECTION ( 'NONE',  ( 1.000000000000000000, 0.000000000000000000, 0.000000000000000000 ) ) ;
#24338 = ORIENTED_EDGE ( 'NONE', *, *, #21052, .F. ) ;
#24339 = VECTOR ( 'NONE', #11368, 1000.000000000000000 ) ;
#24340 = VERTEX_POINT ( 'NONE', #27719 ) ;
#24341 = EDGE_CURVE ( 'NONE', #6008, #27613, #25138, .T. ) ;
#24342 = ADVANCED_FACE ( 'NONE', ( #3854 ), #22206, .T. ) ;
#24343 = DIRECTION ( 'NONE',  ( 0.1444367634087880270, -0.9895140329353564468, -2.337439158924956656E-15 ) ) ;
#24344 = DIRECTION ( 'NONE',  ( -0.9635499925192230197, -0.2675283385292204774, -0.000000000000000000 ) ) ;
#24345 = B_SPLINE_CURVE_WITH_KNOTS ( 'NONE', 3,
 ( #12391, #21080, #7361, #17737 ),
 .UNSPECIFIED., .F., .F.,
 ( 4, 4 ),
 ( 0.005298356295608590283, 0.005985224943342820451 ),
 .UNSPECIFIED. ) ;
#24346 = ORIENTED_EDGE ( 'NONE', *, *, #24747, .F. ) ;
#24347 = FACE_OUTER_BOUND ( 'NONE', #7286, .T. ) ;
#24348 = CIRCLE ( 'NONE', #18144, 4.000000000000003553 ) ;
#24349 = DIRECTION ( 'NONE',  ( -0.000000000000000000, 1.000000000000000000, -0.000000000000000000 ) ) ;
#24350 = DIRECTION ( 'NONE',  ( -1.000000000000000000, 0.000000000000000000, 0.000000000000000000 ) ) ;
#24351 = CARTESIAN_POINT ( 'NONE',  ( -110.1150203881707910, -1.604996202923496961E-20, 7.500000000000000000 ) ) ;
#24352 = ITEM_DEFINED_TRANSFORMATION ( 'NONE', 'NONE', #1335,  #28566 ) ;
#24353 = VERTEX_POINT ( 'NONE', #6701 ) ;
#24354 = ORIENTED_EDGE ( 'NONE', *, *, #5961, .T. ) ;
#24355 = DIRECTION ( 'NONE',  ( 0.000000000000000000, -0.5000000000000008882, 0.8660254037844382635 ) ) ;
#24356 = EDGE_CURVE ( 'NONE', #18581, #33069, #22859, .T. ) ;
#24358 = CARTESIAN_POINT ( 'NONE',  ( 0.000000000000000000, 3.524919873834583163E-15, 68.31122994652405112 ) ) ;
#24357 = CARTESIAN_POINT ( 'NONE',  ( -5.021133111225092982, -13.65249191622732461, -87.50000000000000000 ) ) ;
#24359 = VECTOR ( 'NONE', #26080, 1000.000000000000000 ) ;
#24360 = ORIENTED_EDGE ( 'NONE', *, *, #26865, .F. ) ;
#24361 = ORIENTED_EDGE ( 'NONE', *, *, #8064, .T. ) ;
#24362 = CARTESIAN_POINT ( 'NONE',  ( 0.7564103383402180913, 21.20732892273795756, 26.46721543659850795 ) ) ;
#24363 = ORIENTED_EDGE ( 'NONE', *, *, #9583, .F. ) ;
#24364 = EDGE_CURVE ( 'NONE', #19626, #10008, #14030, .T. ) ;
#24365 = CARTESIAN_POINT ( 'NONE',  ( -3.250000000000000000, 5.404196845913421754, 0.000000000000000000 ) ) ;
#24366 = CARTESIAN_POINT ( 'NONE',  ( -445.9999999999999432, 105.0000000000000142, -101.9999999999999858 ) ) ;
#24367 = VERTEX_POINT ( 'NONE', #3505 ) ;
#24368 = EDGE_CURVE ( 'NONE', #20834, #14594, #34769, .T. ) ;
#24369 = VECTOR ( 'NONE', #31874, 1000.000000000000000 ) ;
#24371 = EDGE_CURVE ( 'NONE', #34682, #25632, #22570, .T. ) ;
#24370 = ORIENTED_EDGE ( 'NONE', *, *, #33517, .T. ) ;
#24372 = DIRECTION ( 'NONE',  ( 1.000000000000000000, 0.000000000000000000, 0.000000000000000000 ) ) ;
#24373 = PRODUCT_DEFINITION_SHAPE ( 'NONE', 'NONE',  #35194 ) ;
#24374 = DIRECTION ( 'NONE',  ( 0.000000000000000000, 0.000000000000000000, -1.000000000000000000 ) ) ;
#24375 = ORIENTED_EDGE ( 'NONE', *, *, #34154, .T. ) ;
#24376 = DIRECTION ( 'NONE',  ( 0.000000000000000000, 0.000000000000000000, 1.000000000000000000 ) ) ;
#24377 = LINE ( 'NONE', #21714, #18326 ) ;
#24378 = EDGE_CURVE ( 'NONE', #13039, #29128, #19550, .T. ) ;
#24379 = CARTESIAN_POINT ( 'NONE',  ( 15.99999999999998579, -145.0000000000000000, 187.0000000000000000 ) ) ;
#24380 = CIRCLE ( 'NONE', #9631, 2.036051781435508801 ) ;
#24381 = LINE ( 'NONE', #19242, #32170 ) ;
#24382 = CARTESIAN_POINT ( 'NONE',  ( -8.222411227241363201E-14, -17.84469521343992326, 24.93532764985518568 ) ) ;
#24383 = FACE_OUTER_BOUND ( 'NONE', #10181, .T. ) ;
#24384 = CYLINDRICAL_SURFACE ( 'NONE', #14961, 16.19999999999999574 ) ;
#24385 = CIRCLE ( 'NONE', #13602, 32.54542015209057126 ) ;
#24386 = ORIENTED_EDGE ( 'NONE', *, *, #15048, .T. ) ;
#24387 = CARTESIAN_POINT ( 'NONE',  ( -418.0000000000000000, -104.9999999999999858, -155.0000000000000000 ) ) ;
#24388 = DIRECTION ( 'NONE',  ( 2.631201909438060269E-14, -5.396010391056495992E-16, 0.9999999999999998890 ) ) ;
#24389 = EDGE_LOOP ( 'NONE', ( #16814, #17135, #8280, #13915 ) ) ;
#24390 = VERTEX_POINT ( 'NONE', #24866 ) ;
#24391 = VECTOR ( 'NONE', #19520, 1000.000000000000000 ) ;
#24392 = CARTESIAN_POINT ( 'NONE',  ( 2.789999999999999147, 30.27116788629740185, 3.198253332533701698 ) ) ;
#24393 = APPLICATION_PROTOCOL_DEFINITION ( 'draft international standard', 'automotive_design', 1998, #29861 ) ;
#24394 = EDGE_LOOP ( 'NONE', ( #4537, #20552, #19833, #2338 ) ) ;
#24395 = DIRECTION ( 'NONE',  ( -0.000000000000000000, -0.000000000000000000, -1.000000000000000000 ) ) ;
#24396 = LINE ( 'NONE', #2510, #25542 ) ;
#24397 = VECTOR ( 'NONE', #16897, 1000.000000000000000 ) ;
#24398 = DIRECTION ( 'NONE',  ( 1.000000000000000000, 0.000000000000000000, 0.000000000000000000 ) ) ;
#24399 = ORIENTED_EDGE ( 'NONE', *, *, #32441, .T. ) ;
#24400 = ORIENTED_EDGE ( 'NONE', *, *, #11367, .F. ) ;
#24401 = LINE ( 'NONE', #6058, #20283 ) ;
#24402 = DIRECTION ( 'NONE',  ( 0.000000000000000000, 0.000000000000000000, 1.000000000000000000 ) ) ;
#24403 = CARTESIAN_POINT ( 'NONE',  ( 0.000000000000000000, 6.992329373473909019E-15, 49.43553178847298568 ) ) ;
#24404 = CARTESIAN_POINT ( 'NONE',  ( -5.021133111224989953, -1.691831803474591833, -67.50000000000000000 ) ) ;
#24405 = CARTESIAN_POINT ( 'NONE',  ( 2.789999999999999147, -3.506335382740735529, 30.89238256715863784 ) ) ;
#24406 = ORIENTED_EDGE ( 'NONE', *, *, #7221, .F. ) ;
#24407 = EDGE_CURVE ( 'NONE', #17012, #30030, #17107, .T. ) ;
#24408 = DIRECTION ( 'NONE',  ( 0.000000000000000000, -1.000000000000000000, -2.465190328815662439E-32 ) ) ;
#24409 = CARTESIAN_POINT ( 'NONE',  ( -499.9999999999999432, 136.9999999999999432, 194.9999999999999716 ) ) ;
#24410 = ADVANCED_FACE ( 'NONE', ( #30574 ), #17245, .F. ) ;
#24411 = FACE_OUTER_BOUND ( 'NONE', #14498, .T. ) ;
#24412 = CIRCLE ( 'NONE', #2740, 2.000000000000001776 ) ;
#24413 = CARTESIAN_POINT ( 'NONE',  ( -410.0000000000000568, -112.9999999999999858, -155.0000000000000000 ) ) ;
#24414 = DIRECTION ( 'NONE',  ( 0.000000000000000000, 1.000000000000000000, 0.000000000000000000 ) ) ;
#24416 = CARTESIAN_POINT ( 'NONE',  ( -99.92113738465764072, 0.6978363313042835747, -7.475210363867073937 ) ) ;
#24415 = CARTESIAN_POINT ( 'NONE',  ( -8.208060149029089991E-14, -23.48523522029074329, 19.71414358107259091 ) ) ;
#24417 = CARTESIAN_POINT ( 'NONE',  ( -15.99999999999998579, -145.0000000000000000, 162.9999999999999716 ) ) ;
#24418 = ORIENTED_EDGE ( 'NONE', *, *, #29080, .T. ) ;
#24419 = CARTESIAN_POINT ( 'NONE',  ( -499.9999999999999432, 136.9999999999999432, 159.0000000000000000 ) ) ;
#24421 = CARTESIAN_POINT ( 'NONE',  ( -499.9999999999999432, 136.9999999999999432, -162.9999999999999716 ) ) ;
#24420 = CARTESIAN_POINT ( 'NONE',  ( -499.9999999999999432, -113.0000000000000000, -162.9999999999999716 ) ) ;
#24422 = ORIENTED_EDGE ( 'NONE', *, *, #27771, .F. ) ;
#24423 = DIRECTION ( 'NONE',  ( 0.000000000000000000, 0.9510565162951500895, 0.3090169943749579984 ) ) ;
#24424 = ORIENTED_EDGE ( 'NONE', *, *, #13519, .T. ) ;
#24425 =( REPRESENTATION_RELATIONSHIP ('NONE','NONE', #23037, #28231 ) REPRESENTATION_RELATIONSHIP_WITH_TRANSFORMATION ( #27428 )SHAPE_REPRESENTATION_RELATIONSHIP( ) );
#24426 = ORIENTED_EDGE ( 'NONE', *, *, #18459, .F. ) ;
#24427 = FACE_BOUND ( 'NONE', #12679, .T. ) ;
#24428 = ORIENTED_EDGE ( 'NONE', *, *, #4200, .F. ) ;
#24429 = VERTEX_POINT ( 'NONE', #22741 ) ;
#24430 = CARTESIAN_POINT ( 'NONE',  ( -499.9999999999999432, 136.9999999999999432, 194.9999999999999716 ) ) ;
#24431 = DIRECTION ( 'NONE',  ( -0.000000000000000000, -0.000000000000000000, -1.000000000000000000 ) ) ;
#24432 = PLANE ( 'NONE',  #28477 ) ;
#24433 = ORIENTED_EDGE ( 'NONE', *, *, #971, .F. ) ;
#24434 = EDGE_LOOP ( 'NONE', ( #2616, #11058, #6667, #27333 ) ) ;
#24435 = LINE ( 'NONE', #15945, #3746 ) ;
#24436 = DIRECTION ( 'NONE',  ( 0.000000000000000000, 0.000000000000000000, 1.000000000000000000 ) ) ;
#24437 = EDGE_CURVE ( 'NONE', #10330, #12319, #20424, .T. ) ;
#24438 = DIRECTION ( 'NONE',  ( 1.000000000000000000, 0.000000000000000000, 0.000000000000000000 ) ) ;
#24439 = FACE_OUTER_BOUND ( 'NONE', #4127, .T. ) ;
#24440 = ORIENTED_EDGE ( 'NONE', *, *, #806, .F. ) ;
#24441 = AXIS2_PLACEMENT_3D ( 'NONE', #18735, #7667, #7488 ) ;
#24442 = LINE ( 'NONE', #32815, #24201 ) ;
#24443 = EDGE_CURVE ( 'NONE', #19066, #4867, #34645, .T. ) ;
#24444 = DIRECTION ( 'NONE',  ( 0.000000000000000000, 1.000000000000000000, -2.309213040847544338E-50 ) ) ;
#24445 = ORIENTED_EDGE ( 'NONE', *, *, #23919, .T. ) ;
#24446 = PRODUCT_RELATED_PRODUCT_CATEGORY ( 'part', '', ( #32778 ) ) ;
#24447 = CARTESIAN_POINT ( 'NONE',  ( 145.0000000000000568, -90.42893218813456713, 44.81798139211241505 ) ) ;
#24448 = LINE ( 'NONE', #32989, #20592 ) ;
#24449 = DIRECTION ( 'NONE',  ( 0.000000000000000000, 0.000000000000000000, -1.000000000000000000 ) ) ;
#24450 = CARTESIAN_POINT ( 'NONE',  ( -20.00000000000007461, 104.9999999999999858, 162.9999999999999716 ) ) ;
#24451 = ORIENTED_EDGE ( 'NONE', *, *, #23191, .T. ) ;
#24452 = CIRCLE ( 'NONE', #29013, 4.309328216469825001 ) ;
#24453 = LINE ( 'NONE', #16483, #7029 ) ;
#24454 = B_SPLINE_CURVE_WITH_KNOTS ( 'NONE', 3,
 ( #21701, #32548, #16917, #8698, #8167, #14239 ),
 .UNSPECIFIED., .F., .F.,
 ( 4, 2, 4 ),
 ( 2.717607641618062802E-07, 0.001873470133380088784, 0.003746668505996015794 ),
 .UNSPECIFIED. ) ;
#24455 = ORIENTED_EDGE ( 'NONE', *, *, #2391, .F. ) ;
#24456 = CARTESIAN_POINT ( 'NONE',  ( 2.789999999999999147, 27.98916443103598439, 15.38717335695048227 ) ) ;
#24457 = LINE ( 'NONE', #18978, #2304 ) ;
#24458 = ORIENTED_EDGE ( 'NONE', *, *, #14398, .T. ) ;
#24459 = SURFACE_STYLE_FILL_AREA ( #13631 ) ;
#24460 = CARTESIAN_POINT ( 'NONE',  ( 10.00000000000000000, 7.794228634059941818, 13.49999999999999645 ) ) ;
#24461 = CIRCLE ( 'NONE', #26765, 32.54542015209055705 ) ;
#24462 = ORIENTED_EDGE ( 'NONE', *, *, #367, .T. ) ;
#24463 = VECTOR ( 'NONE', #6715, 1000.000000000000000 ) ;
#24464 = EDGE_LOOP ( 'NONE', ( #9050, #17729, #31427, #18853 ) ) ;
#24465 = LINE ( 'NONE', #106, #4971 ) ;
#24466 = CARTESIAN_POINT ( 'NONE',  ( -100.0586838875211413, 1.365406536427365758, 7.382450522560827899 ) ) ;
#24467 = EDGE_LOOP ( 'NONE', ( #34988, #21260, #23575, #10652, #22740, #4408, #7382, #26539, #24440, #19164, #19517, #15227, #286, #11307, #29263, #34965, #431, #31934, #35044, #2005, #2157, #33771, #33143, #14354, #25606, #18653, #8602, #15425, #13475, #6630, #16105, #2682, #25546, #34028, #3320, #1536, #26419, #2, #27151, #32099, #25832, #19518, #3641, #22658, #2994, #31245, #28397, #21812, #18088, #27590, #31286, #22775, #3465, #4169, #24277, #34747, #28252, #32539, #22305, #29742, #1301, #20867, #27242, #34755, #3006, #31725, #28183, #10357, #8955, #23472, #28141, #22051, #29877, #28210, #31024, #8168, #26939, #26693, #3400, #25974, #28321, #27145, #33942, #32304 ) ) ;
#24468 = VERTEX_POINT ( 'NONE', #9729 ) ;
#24469 = CARTESIAN_POINT ( 'NONE',  ( 145.0000000000000568, -78.33668825982579165, -75.00000000000001421 ) ) ;
#24470 = LINE ( 'NONE', #32152, #30664 ) ;
#24471 = CARTESIAN_POINT ( 'NONE',  ( 2.265105808055940972, -23.79505697368644235, -23.40952781232680024 ) ) ;
#24472 = CIRCLE ( 'NONE', #13703, 32.54542015209057126 ) ;
#24473 = DIRECTION ( 'NONE',  ( -0.000000000000000000, -0.000000000000000000, -1.000000000000000000 ) ) ;
#24474 = VERTEX_POINT ( 'NONE', #15265 ) ;
#24475 = VERTEX_POINT ( 'NONE', #20941 ) ;
#24476 = CARTESIAN_POINT ( 'NONE',  ( -19.99999999999998934, 134.9999999999998863, 187.0000000000000000 ) ) ;
#24477 = DIRECTION ( 'NONE',  ( 0.000000000000000000, 0.000000000000000000, 1.000000000000000000 ) ) ;
#24478 = COLOUR_RGB ( '',0.7921568627450980005, 0.8196078431372548767, 0.9333333333333333481 ) ;
#24479 = CARTESIAN_POINT ( 'NONE',  ( 2.789999999999999147, 14.59907093257217170, 26.74544485249471393 ) ) ;
#24480 = ADVANCED_FACE ( 'NONE', ( #25933 ), #1550, .F. ) ;
#24481 = DIRECTION ( 'NONE',  ( 0.000000000000000000, 2.309213040847544338E-50, 1.000000000000000000 ) ) ;
#24482 = LINE ( 'NONE', #11516, #29301 ) ;
#24483 = DIRECTION ( 'NONE',  ( 0.000000000000000000, 1.000000000000000000, 1.224646799147353207E-16 ) ) ;
#24484 = FACE_OUTER_BOUND ( 'NONE', #26610, .T. ) ;
#24485 = EDGE_LOOP ( 'NONE', ( #32568, #16181, #3116, #15178 ) ) ;
#24486 = AXIS2_PLACEMENT_3D ( 'NONE', #32419, #3050, #10731 ) ;
#24487 = ADVANCED_FACE ( 'NONE', ( #23610 ), #17763, .T. ) ;
#24488 = DIRECTION ( 'NONE',  ( 0.000000000000000000, 1.836970198721029688E-16, -1.000000000000000000 ) ) ;
#24489 = CARTESIAN_POINT ( 'NONE',  ( 1.999999999999999556, 0.000000000000000000, 0.000000000000000000 ) ) ;
#24490 = AXIS2_PLACEMENT_3D ( 'NONE', #6497, #9178, #23073 ) ;
#24491 = DIRECTION ( 'NONE',  ( 0.000000000000000000, 0.000000000000000000, -1.000000000000000000 ) ) ;
#24492 = ORIENTED_EDGE ( 'NONE', *, *, #31257, .F. ) ;
#24493 = EDGE_CURVE ( 'NONE', #21561, #9083, #23270, .T. ) ;
#24494 = CARTESIAN_POINT ( 'NONE',  ( 2.789999999999999147, -29.69698570178010755, -11.75786841620047163 ) ) ;
#24495 = ORIENTED_EDGE ( 'NONE', *, *, #10700, .F. ) ;
#24496 = CARTESIAN_POINT ( 'NONE',  ( -102.4259802790519416, 4.432569708812561515, -11.68934771181378629 ) ) ;
#24497 = EDGE_CURVE ( 'NONE', #33261, #8977, #23787, .T. ) ;
#24498 = PLANE ( 'NONE',  #32054 ) ;
#24499 = EDGE_CURVE ( 'NONE', #7307, #9877, #18874, .T. ) ;
#24501 = ORIENTED_EDGE ( 'NONE', *, *, #11144, .F. ) ;
#24500 = AXIS2_PLACEMENT_3D ( 'NONE', #29550, #12837, #21006 ) ;
#24502 = VECTOR ( 'NONE', #7967, 1000.000000000000000 ) ;
#24503 = CARTESIAN_POINT ( 'NONE',  ( -45.00000000000000000, 16.36947364650383818, 36.69637551990492597 ) ) ;
#24504 = VECTOR ( 'NONE', #17382, 1000.000000000000000 ) ;
#24505 = DIRECTION ( 'NONE',  ( -1.000000000000000000, -0.000000000000000000, -0.000000000000000000 ) ) ;
#24506 = LINE ( 'NONE', #22036, #20591 ) ;
#24507 = ORIENTED_EDGE ( 'NONE', *, *, #23316, .T. ) ;
#24508 = EDGE_LOOP ( 'NONE', ( #6422, #19540, #11690, #17572 ) ) ;
#24509 = B_SPLINE_CURVE_WITH_KNOTS ( 'NONE', 3,
 ( #9359, #31074, #6675, #2168, #10352, #34565 ),
 .UNSPECIFIED., .F., .F.,
 ( 4, 2, 4 ),
 ( 4.404817065346997443E-07, 0.001874269648071526803, 0.003748098814436519148 ),
 .UNSPECIFIED. ) ;
#24510 = DIRECTION ( 'NONE',  ( 0.1063910735369155841, -0.9943243633099125844, -3.335902418025060287E-15 ) ) ;
#24511 = LINE ( 'NONE', #32359, #7571 ) ;
#24512 = ORIENTED_EDGE ( 'NONE', *, *, #33390, .T. ) ;
#24513 = DIRECTION ( 'NONE',  ( 1.000000000000000000, 0.000000000000000000, 5.546364386991661285E-52 ) ) ;
#24514 = VECTOR ( 'NONE', #9053, 1000.000000000000000 ) ;
#24515 = DIRECTION ( 'NONE',  ( 1.000000000000000000, 0.000000000000000000, -0.000000000000000000 ) ) ;
#24516 = CARTESIAN_POINT ( 'NONE',  ( 0.000000000000000000, 20.79173593595263370, 22.27454621808773538 ) ) ;
#24517 = LINE ( 'NONE', #29705, #10236 ) ;
#24518 = VERTEX_POINT ( 'NONE', #10083 ) ;
#24519 = ORIENTED_EDGE ( 'NONE', *, *, #4549, .F. ) ;
#24520 = VERTEX_POINT ( 'NONE', #31271 ) ;
#24521 = DIRECTION ( 'NONE',  ( -1.000000000000000000, 0.000000000000000000, -5.546364386991661285E-52 ) ) ;
#24522 = CARTESIAN_POINT ( 'NONE',  ( -8.483176869585901368E-14, -30.61525927030269756, -1.705757817505873630 ) ) ;
#24523 = CARTESIAN_POINT ( 'NONE',  ( 55.00000000000000711, 0.000000000000000000, 6.898500000000000298 ) ) ;
#24525 = VERTEX_POINT ( 'NONE', #31785 ) ;
#24524 = AXIS2_PLACEMENT_3D ( 'NONE', #25776, #1579, #3536 ) ;
#24526 = ORIENTED_EDGE ( 'NONE', *, *, #5002, .T. ) ;
#24527 = DIRECTION ( 'NONE',  ( -1.000000000000000000, -0.000000000000000000, 0.000000000000000000 ) ) ;
#24528 = CIRCLE ( 'NONE', #20565, 10.00000000000000000 ) ;
#24529 = VERTEX_POINT ( 'NONE', #25752 ) ;
#24530 = AXIS2_PLACEMENT_3D ( 'NONE', #23969, #7243, #15987 ) ;
#24531 = VECTOR ( 'NONE', #28633, 1000.000000000000000 ) ;
#24532 = CARTESIAN_POINT ( 'NONE',  ( 2.789999999999999147, 17.11426446101236820, -26.96776559937708129 ) ) ;
#24533 = ADVANCED_FACE ( 'NONE', ( #9903 ), #7044, .F. ) ;
#24534 = CARTESIAN_POINT ( 'NONE',  ( -361.0000000000000000, 134.9999999999999716, 110.0000000000000000 ) ) ;
#24535 = EDGE_LOOP ( 'NONE', ( #13462, #25741, #3309, #14798 ) ) ;
#24536 = EDGE_LOOP ( 'NONE', ( #1527, #25268, #33699, #17726 ) ) ;
#24537 = DIRECTION ( 'NONE',  ( 0.000000000000000000, 0.000000000000000000, 1.000000000000000000 ) ) ;
#24538 = EDGE_CURVE ( 'NONE', #25895, #7844, #23433, .T. ) ;
#24539 = ADVANCED_FACE ( 'NONE', ( #20766 ), #21110, .T. ) ;
#24540 = DIRECTION ( 'NONE',  ( 0.000000000000000000, 1.000000000000000000, 5.053935297177146739E-49 ) ) ;
#24541 = ORIENTED_EDGE ( 'NONE', *, *, #21204, .T. ) ;
#24542 = LINE ( 'NONE', #30434, #29440 ) ;
#24543 = DIRECTION ( 'NONE',  ( 0.000000000000000000, -1.000000000000000000, -1.836970198721029934E-16 ) ) ;
#24544 = LINE ( 'NONE', #21716, #768 ) ;
#24545 = LINE ( 'NONE', #2148, #22528 ) ;
#24546 = CARTESIAN_POINT ( 'NONE',  ( 2.765921099434983876, -15.32140196853734970, -27.05343472113007763 ) ) ;
#24547 = DIRECTION ( 'NONE',  ( -0.000000000000000000, -0.000000000000000000, -1.000000000000000000 ) ) ;
#24548 = FACE_OUTER_BOUND ( 'NONE', #30929, .T. ) ;
#24549 = ADVANCED_FACE ( 'NONE', ( #31957 ), #7220, .T. ) ;
#24550 = VECTOR ( 'NONE', #19727, 1000.000000000000114 ) ;
#24551 = ORIENTED_EDGE ( 'NONE', *, *, #5654, .F. ) ;
#24552 = VECTOR ( 'NONE', #11845, 1000.000000000000000 ) ;
#24553 = DIRECTION ( 'NONE',  ( -1.000000000000000000, 0.000000000000000000, 0.000000000000000000 ) ) ;
#24554 = DIRECTION ( 'NONE',  ( 6.982748503361761110E-15, -6.990337062275464198E-15, 1.000000000000000000 ) ) ;
#24555 = AXIS2_PLACEMENT_3D ( 'NONE', #18499, #29337, #31641 ) ;
#24556 = ORIENTED_EDGE ( 'NONE', *, *, #11807, .F. ) ;
#24558 = ORIENTED_EDGE ( 'NONE', *, *, #25837, .F. ) ;
#24557 = ADVANCED_FACE ( 'NONE', ( #15434 ), #26272, .T. ) ;
#24559 = ADVANCED_FACE ( 'NONE', ( #1887, #12768 ), #15612, .F. ) ;
#24560 = EDGE_CURVE ( 'NONE', #22259, #7553, #6870, .T. ) ;
#24561 = CARTESIAN_POINT ( 'NONE',  ( 99.26191511054601335, -2.804307960831458189E-14, 7.500000000000241585 ) ) ;
#24562 = SHAPE_DEFINITION_REPRESENTATION ( #17780, #29156 ) ;
#24563 = ORIENTED_EDGE ( 'NONE', *, *, #23435, .F. ) ;
#24564 = CARTESIAN_POINT ( 'NONE',  ( -11.99999999999998224, -134.9999999999999716, 155.0000000000000000 ) ) ;
#24565 = LINE ( 'NONE', #32762, #33500 ) ;
#24566 = ADVANCED_FACE ( 'NONE', ( #10790 ), #11146, .T. ) ;
#24567 = ITEM_DEFINED_TRANSFORMATION ( 'NONE', 'NONE', #7027,  #28566 ) ;
#24569 = CARTESIAN_POINT ( 'NONE',  ( -8.149999999999998579, 2.020667218593133001E-16, 3.180000000000000160 ) ) ;
#24568 = CYLINDRICAL_SURFACE ( 'NONE', #13901, 1.649999999999999467 ) ;
#24570 = ORIENTED_EDGE ( 'NONE', *, *, #7181, .F. ) ;
#24571 = ORIENTED_EDGE ( 'NONE', *, *, #20136, .F. ) ;
#24572 = FACE_OUTER_BOUND ( 'NONE', #30428, .T. ) ;
#24573 = FACE_OUTER_BOUND ( 'NONE', #21629, .T. ) ;
#24574 = DIRECTION ( 'NONE',  ( 0.000000000000000000, 0.000000000000000000, 1.000000000000000000 ) ) ;
#24575 = CARTESIAN_POINT ( 'NONE',  ( 10.17231796313409298, 4.274639749586561344, -77.50000000000000000 ) ) ;
#24576 = LINE ( 'NONE', #21928, #30919 ) ;
#24577 = ORIENTED_EDGE ( 'NONE', *, *, #14292, .F. ) ;
#24578 = AXIS2_PLACEMENT_3D ( 'NONE', #19251, #903, #28124 ) ;
#24579 = DIRECTION ( 'NONE',  ( -1.000000000000000000, -0.000000000000000000, -0.000000000000000000 ) ) ;
#24580 = DIRECTION ( 'NONE',  ( 0.000000000000000000, 0.000000000000000000, 1.000000000000000000 ) ) ;
#24581 = CARTESIAN_POINT ( 'NONE',  ( 22.89764159710613001, 8.346743312457579833, -77.50000000000000000 ) ) ;
#24582 = VECTOR ( 'NONE', #4318, 1000.000000000000000 ) ;
#24583 = CIRCLE ( 'NONE', #18367, 10.00000000000000000 ) ;
#24584 = EDGE_CURVE ( 'NONE', #24075, #8817, #16140, .T. ) ;
#24585 = EDGE_CURVE ( 'NONE', #21475, #6239, #30803, .T. ) ;
#24586 = CARTESIAN_POINT ( 'NONE',  ( 2.765921099433442443, 31.00221527374952046, -2.344426712874310148 ) ) ;
#24587 = LINE ( 'NONE', #18760, #21220 ) ;
#24589 = DIRECTION ( 'NONE',  ( 1.000000000000000000, 0.000000000000000000, 0.000000000000000000 ) ) ;
#24588 = CARTESIAN_POINT ( 'NONE',  ( -5.823698994896891357, -1.505030548027689319, 3.180000000000000160 ) ) ;
#24590 = CARTESIAN_POINT ( 'NONE',  ( 2.783107617264021005, 25.89094059359499056, -16.81082004999754531 ) ) ;
#24591 = EDGE_LOOP ( 'NONE', ( #23295, #27656, #10744, #17391 ) ) ;
#24592 = CARTESIAN_POINT ( 'NONE',  ( 0.02407890056655695096, -26.45933846664182099, -16.32596387352474565 ) ) ;
#24594 = CARTESIAN_POINT ( 'NONE',  ( 2.719010676553170303, -31.66360817300141406, -1.400248398912504300 ) ) ;
#24593 = LINE ( 'NONE', #5029, #21170 ) ;
#24595 = VECTOR ( 'NONE', #20371, 1000.000000000000000 ) ;
#24596 = ORIENTED_EDGE ( 'NONE', *, *, #6057, .T. ) ;
#24597 = CARTESIAN_POINT ( 'NONE',  ( 187.4264068711928530, -12.50000000000001066, 1.224646799147353217E-14 ) ) ;
#24598 = EDGE_LOOP ( 'NONE', ( #31200, #10221, #5987, #9630 ) ) ;
#24599 = ADVANCED_FACE ( 'NONE', ( #18462 ), #7568, .F. ) ;
#24600 = AXIS2_PLACEMENT_3D ( 'NONE', #6578, #17993, #17478 ) ;
#24601 = EDGE_CURVE ( 'NONE', #22010, #802, #32659, .T. ) ;
#24602 = AXIS2_PLACEMENT_3D ( 'NONE', #28940, #32303, #12761 ) ;
#24603 = AXIS2_PLACEMENT_3D ( 'NONE', #10907, #7879, #5714 ) ;
#24604 = ORIENTED_EDGE ( 'NONE', *, *, #6017, .F. ) ;
#24605 = PLANE ( 'NONE',  #5908 ) ;
#24606 = ORIENTED_EDGE ( 'NONE', *, *, #26141, .F. ) ;
#24607 = EDGE_LOOP ( 'NONE', ( #1406, #5527, #2992, #26936 ) ) ;
#24608 = DIRECTION ( 'NONE',  ( -0.000000000000000000, -0.000000000000000000, -1.000000000000000000 ) ) ;
#24609 = EDGE_CURVE ( 'NONE', #23520, #13039, #21726, .T. ) ;
#24610 = DIRECTION ( 'NONE',  ( -1.232595164407830946E-32, 0.000000000000000000, -1.000000000000000000 ) ) ;
#24611 = DIRECTION ( 'NONE',  ( -0.000000000000000000, 1.310824597558155437E-49, 1.000000000000000000 ) ) ;
#24612 = EDGE_LOOP ( 'NONE', ( #23568, #31543, #10074, #24861, #242, #22109, #29073, #27549 ) ) ;
#24613 = ORIENTED_EDGE ( 'NONE', *, *, #21415, .T. ) ;
#24614 = LINE ( 'NONE', #8433, #28754 ) ;
#24615 = EDGE_CURVE ( 'NONE', #27476, #19297, #21147, .T. ) ;
#24616 = DIRECTION ( 'NONE',  ( 1.000000000000000000, -0.000000000000000000, -0.000000000000000000 ) ) ;
#24617 = DIRECTION ( 'NONE',  ( -0.000000000000000000, 1.836970198721029688E-16, -1.000000000000000000 ) ) ;
#24618 = DIRECTION ( 'NONE',  ( 0.000000000000000000, 1.000000000000000000, 0.000000000000000000 ) ) ;
#24619 = ORIENTED_EDGE ( 'NONE', *, *, #3289, .T. ) ;
#24620 = LINE ( 'NONE', #19670, #17970 ) ;
#24621 = TOROIDAL_SURFACE ( 'NONE', #24647, 30.47050528711512030, 8.000000000000000000 ) ;
#24622 = CARTESIAN_POINT ( 'NONE',  ( 8.000000000000003553, 0.000000000000000000, 0.000000000000000000 ) ) ;
#24623 = VERTEX_POINT ( 'NONE', #281 ) ;
#24624 = DIRECTION ( 'NONE',  ( 0.000000000000000000, 0.000000000000000000, 1.000000000000000000 ) ) ;
#24625 = LINE ( 'NONE', #19493, #6372 ) ;
#24626 = LINE ( 'NONE', #27487, #23717 ) ;
#24627 = AXIS2_PLACEMENT_3D ( 'NONE', #13295, #20946, #15438 ) ;
#24628 = CARTESIAN_POINT ( 'NONE',  ( -19.99999999999998934, 144.9999999999999716, 187.0000000000000000 ) ) ;
#24629 = EDGE_LOOP ( 'NONE', ( #9597, #9306, #2229, #14161, #23388, #7849 ) ) ;
#24630 = TOROIDAL_SURFACE ( 'NONE', #767, 30.47050528711511674, 8.000000000000000000 ) ;
#24631 = AXIS2_PLACEMENT_3D ( 'NONE', #6205, #14069, #3724 ) ;
#24632 = CARTESIAN_POINT ( 'NONE',  ( -5.210000000000000853, 0.000000000000000000, 0.000000000000000000 ) ) ;
#24633 = EDGE_LOOP ( 'NONE', ( #32939, #23117, #18182, #14775 ) ) ;
#24634 = EDGE_CURVE ( 'NONE', #13694, #26431, #10728, .T. ) ;
#24636 = CARTESIAN_POINT ( 'NONE',  ( 0.02407890056655695096, 20.99477179376858871, -22.93149026599722617 ) ) ;
#24635 = DIRECTION ( 'NONE',  ( -1.000000000000000000, -0.000000000000000000, -0.000000000000000000 ) ) ;
#24637 = FACE_BOUND ( 'NONE', #25050, .T. ) ;
#24638 = ORIENTED_EDGE ( 'NONE', *, *, #20488, .T. ) ;
#24639 =( REPRESENTATION_RELATIONSHIP ('NONE','NONE', #23037, #15767 ) REPRESENTATION_RELATIONSHIP_WITH_TRANSFORMATION ( #6361 )SHAPE_REPRESENTATION_RELATIONSHIP( ) );
#24640 = DIRECTION ( 'NONE',  ( 0.000000000000000000, 0.000000000000000000, -1.000000000000000000 ) ) ;
#24641 = DIRECTION ( 'NONE',  ( 0.000000000000000000, -1.000000000000000000, 0.000000000000000000 ) ) ;
#24642 = ADVANCED_FACE ( 'NONE', ( #29306 ), #98, .F. ) ;
#24643 = ORIENTED_EDGE ( 'NONE', *, *, #5479, .T. ) ;
#24644 = EDGE_LOOP ( 'NONE', ( #5567, #8973, #24338, #16519 ) ) ;
#24645 = ADVANCED_FACE ( 'NONE', ( #13457 ), #5074, .F. ) ;
#24646 = EDGE_CURVE ( 'NONE', #1704, #16210, #5248, .T. ) ;
#24647 = AXIS2_PLACEMENT_3D ( 'NONE', #22458, #33312, #13857 ) ;
#24648 = ORIENTED_EDGE ( 'NONE', *, *, #20187, .T. ) ;
#24649 = CARTESIAN_POINT ( 'NONE',  ( 2.789999999999999147, 2.005524111408653720, -31.87689292423236154 ) ) ;
#24650 = CARTESIAN_POINT ( 'NONE',  ( -109.0659643713068903, 3.171022835462813383, 6.816853140736490069 ) ) ;
#24651 = VERTEX_POINT ( 'NONE', #15966 ) ;
#24652 = ORIENTED_EDGE ( 'NONE', *, *, #12810, .F. ) ;
#24653 = DIRECTION ( 'NONE',  ( 0.000000000000000000, 1.000000000000000000, 1.224646799147353207E-16 ) ) ;
#24654 = PLANE ( 'NONE',  #31701 ) ;
#24655 = LINE ( 'NONE', #3128, #34062 ) ;
#24656 = AXIS2_PLACEMENT_3D ( 'NONE', #25308, #11976, #9111 ) ;
#24657 = LINE ( 'NONE', #16679, #31650 ) ;
#24658 = CARTESIAN_POINT ( 'NONE',  ( 145.0000000000000568, -89.01471862576147487, 43.40376782973931569 ) ) ;
#24659 = ORIENTED_EDGE ( 'NONE', *, *, #10044, .T. ) ;
#24660 = EDGE_LOOP ( 'NONE', ( #21800, #168, #14602, #7764 ) ) ;
#24661 = CIRCLE ( 'NONE', #7030, 3.999999999999976019 ) ;
#24662 = CARTESIAN_POINT ( 'NONE',  ( -20.00000000000001776, -113.0000000000000000, 187.0000000000000000 ) ) ;
#24663 = CARTESIAN_POINT ( 'NONE',  ( -418.0000000000000568, 104.9999999999999858, -159.0000000000000000 ) ) ;
#24664 = LINE ( 'NONE', #18487, #11814 ) ;
#24665 = VECTOR ( 'NONE', #27989, 1000.000000000000000 ) ;
#24666 = DIRECTION ( 'NONE',  ( -1.000000000000000000, 0.000000000000000000, 0.000000000000000000 ) ) ;
#24667 = DIRECTION ( 'NONE',  ( -1.000000000000000000, -0.000000000000000000, -0.000000000000000000 ) ) ;
#24668 = CARTESIAN_POINT ( 'NONE',  ( 145.0000000000000568, -90.29102463692673552, -73.95413108702813076 ) ) ;
#24669 = DIRECTION ( 'NONE',  ( 0.000000000000000000, -1.000000000000000000, -2.132064625830773463E-16 ) ) ;
#24670 = ORIENTED_EDGE ( 'NONE', *, *, #15699, .F. ) ;
#24671 = DIRECTION ( 'NONE',  ( 0.000000000000000000, -1.000000000000000000, 0.000000000000000000 ) ) ;
#24672 = DIRECTION ( 'NONE',  ( 0.9476531711828023452, -0.3193015301359802827, -0.000000000000000000 ) ) ;
#24673 = CARTESIAN_POINT ( 'NONE',  ( 19.99999999999998934, 124.9999999999999716, 162.9999999999999716 ) ) ;
#24674 = ORIENTED_EDGE ( 'NONE', *, *, #33065, .F. ) ;
#24675 = AXIS2_PLACEMENT_3D ( 'NONE', #31967, #10262, #21121 ) ;
#24676 = DIRECTION ( 'NONE',  ( -1.000000000000000000, -0.000000000000000000, -0.000000000000000000 ) ) ;
#24677 = ORIENTED_EDGE ( 'NONE', *, *, #4398, .F. ) ;
#24678 = CARTESIAN_POINT ( 'NONE',  ( 8.000000000000000000, 0.000000000000000000, 0.000000000000000000 ) ) ;
#24679 = VECTOR ( 'NONE', #4870, 1000.000000000000114 ) ;
#24680 = CARTESIAN_POINT ( 'NONE',  ( -100.0523128185887600, 1.341502966352551951, -12.43231302123709625 ) ) ;
#24681 = VECTOR ( 'NONE', #2177, 1000.000000000000000 ) ;
#24682 = AXIS2_PLACEMENT_3D ( 'NONE', #21755, #34764, #21233 ) ;
#24683 = EDGE_LOOP ( 'NONE', ( #23851, #727, #12843, #31424 ) ) ;
#24684 = ADVANCED_FACE ( 'NONE', ( #7750 ), #18638, .F. ) ;
#24685 = MANIFOLD_SOLID_BREP ( 'Trim/Extend3[2]', #20037 ) ;
#24686 = DIRECTION ( 'NONE',  ( 0.000000000000000000, -1.000000000000000000, -5.145227585319922065E-49 ) ) ;
#24687 = CARTESIAN_POINT ( 'NONE',  ( -365.0000000000000000, -119.0000000000000000, 111.9999999999999858 ) ) ;
#24688 = FACE_OUTER_BOUND ( 'NONE', #21338, .T. ) ;
#24689 = EDGE_CURVE ( 'NONE', #640, #6216, #32513, .T. ) ;
#24690 = ORIENTED_EDGE ( 'NONE', *, *, #9611, .F. ) ;
#24692 = ORIENTED_EDGE ( 'NONE', *, *, #7180, .T. ) ;
#24691 = EDGE_CURVE ( 'NONE', #28031, #18691, #25175, .T. ) ;
#24693 = CARTESIAN_POINT ( 'NONE',  ( 842.2774702764955919, 1112.688053266747602, 1753.598338701303419 ) ) ;
#24694 = LINE ( 'NONE', #19037, #16143 ) ;
#24695 = ADVANCED_FACE ( 'NONE', ( #33000 ), #628, .T. ) ;
#24696 = ORIENTED_EDGE ( 'NONE', *, *, #11309, .T. ) ;
#24697 = B_SPLINE_CURVE_WITH_KNOTS ( 'NONE', 3,
 ( #25968, #12460, #15129, #4242 ),
 .UNSPECIFIED., .F., .F.,
 ( 4, 4 ),
 ( 0.005298382169618362676, 0.005985250355243617627 ),
 .UNSPECIFIED. ) ;
#24698 = DIRECTION ( 'NONE',  ( 0.000000000000000000, -1.131431318426415506E-52, -1.000000000000000000 ) ) ;
#24699 = FILL_AREA_STYLE ('',( #27729 ) ) ;
#24700 = VECTOR ( 'NONE', #10397, 1000.000000000000000 ) ;
#24701 = CARTESIAN_POINT ( 'NONE',  ( -9.144464960067640646, -31.23432620483745836, 68.31122994652405112 ) ) ;
#24702 = CARTESIAN_POINT ( 'NONE',  ( -106.3650732166412638, -4.941537997685736094, 5.642681918066573488 ) ) ;
#24703 = CONTEXT_DEPENDENT_SHAPE_REPRESENTATION ( #16725, #3773 ) ;
#24704 = EDGE_LOOP ( 'NONE', ( #659, #34802, #26453, #11982 ) ) ;
#24705 = ORIENTED_EDGE ( 'NONE', *, *, #17990, .T. ) ;
#24706 = ORIENTED_EDGE ( 'NONE', *, *, #1025, .T. ) ;
#24707 = FACE_OUTER_BOUND ( 'NONE', #4338, .T. ) ;
#24708 = CIRCLE ( 'NONE', #19602, 15.00000000000000000 ) ;
#24709 = EDGE_CURVE ( 'NONE', #5991, #5794, #6128, .T. ) ;
#24710 = CARTESIAN_POINT ( 'NONE',  ( 2.765921099433441555, 18.59128259035472297, 24.91982945642928016 ) ) ;
#24711 = PLANE ( 'NONE',  #7068 ) ;
#24712 = CARTESIAN_POINT ( 'NONE',  ( 2.033589659158014040, -24.35732449877370343, 23.60053042972024784 ) ) ;
#24713 = VECTOR ( 'NONE', #11356, 1000.000000000000000 ) ;
#24714 = ORIENTED_EDGE ( 'NONE', *, *, #10497, .F. ) ;
#24715 = ORIENTED_EDGE ( 'NONE', *, *, #14028, .F. ) ;
#24716 = AXIS2_PLACEMENT_3D ( 'NONE', #191, #18891, #13198 ) ;
#24717 = CARTESIAN_POINT ( 'NONE',  ( -29.72561944762172814, -13.25111019240559962, 68.31122994652405112 ) ) ;
#24718 = ORIENTED_EDGE ( 'NONE', *, *, #17850, .F. ) ;
#24719 = FACE_OUTER_BOUND ( 'NONE', #25234, .T. ) ;
#24720 = DIRECTION ( 'NONE',  ( -1.000000000000000000, 0.000000000000000000, -1.292961597001347186E-16 ) ) ;
#24721 = ORIENTED_EDGE ( 'NONE', *, *, #25872, .T. ) ;
#24722 = ORIENTED_EDGE ( 'NONE', *, *, #2757, .F. ) ;
#24723 = FILL_AREA_STYLE ('',( #28291 ) ) ;
#24724 = DIRECTION ( 'NONE',  ( -5.546364386991661285E-52, 0.000000000000000000, -1.000000000000000000 ) ) ;
#24725 = ORIENTED_EDGE ( 'NONE', *, *, #9450, .F. ) ;
#24726 = DIRECTION ( 'NONE',  ( 0.000000000000000000, 0.000000000000000000, 1.000000000000000000 ) ) ;
#24727 = DIRECTION ( 'NONE',  ( 0.000000000000000000, 1.000000000000000000, 1.224646799147353207E-16 ) ) ;
#24728 = CARTESIAN_POINT ( 'NONE',  ( 0.5288002557345565791, -1.325911039506977307, -33.36347027112250885 ) ) ;
#24729 = DIRECTION ( 'NONE',  ( 0.9635499925192231307, 0.2675283385292199223, 0.000000000000000000 ) ) ;
#24730 = VECTOR ( 'NONE', #18384, 1000.000000000000000 ) ;
#24731 = CIRCLE ( 'NONE', #33842, 7.999999999999979572 ) ;
#24732 = DIRECTION ( 'NONE',  ( 0.000000000000000000, 0.000000000000000000, -1.000000000000000000 ) ) ;
#24733 = CARTESIAN_POINT ( 'NONE',  ( -19.99999999999998934, 4.559999999999909015, -168.2400000000000091 ) ) ;
#24734 = AXIS2_PLACEMENT_3D ( 'NONE', #13832, #24667, #32859 ) ;
#24735 = EDGE_CURVE ( 'NONE', #7560, #30758, #30345, .T. ) ;
#24736 = ORIENTED_EDGE ( 'NONE', *, *, #17946, .F. ) ;
#24737 = ORIENTED_EDGE ( 'NONE', *, *, #30391, .T. ) ;
#24739 = CIRCLE ( 'NONE', #9419, 7.999999999999986677 ) ;
#24738 = CARTESIAN_POINT ( 'NONE',  ( 10.17231796313411429, 15.60017778382161246, -77.50000000000000000 ) ) ;
#24740 = DIRECTION ( 'NONE',  ( 0.1063910735368947813, -0.9943243633099144718, -3.335902418024520312E-15 ) ) ;
#24741 = VECTOR ( 'NONE', #21250, 1000.000000000000000 ) ;
#24742 = ADVANCED_FACE ( 'NONE', ( #19864 ), #33369, .F. ) ;
#24743 = ORIENTED_EDGE ( 'NONE', *, *, #4995, .T. ) ;
#24744 = VECTOR ( 'NONE', #20157, 1000.000000000000000 ) ;
#24745 = ORIENTED_EDGE ( 'NONE', *, *, #15158, .T. ) ;
#24746 = EDGE_CURVE ( 'NONE', #20661, #11247, #1257, .T. ) ;
#24747 = EDGE_CURVE ( 'NONE', #6860, #18426, #17202, .T. ) ;
#24748 = CARTESIAN_POINT ( 'NONE',  ( 104.0203572285688267, 5.657131480001861057, 4.924467467246998353 ) ) ;
#24749 = EDGE_CURVE ( 'NONE', #7373, #18794, #3459, .T. ) ;
#24750 = APPLICATION_PROTOCOL_DEFINITION ( 'draft international standard', 'automotive_design', 1998, #33968 ) ;
#24751 = EDGE_LOOP ( 'NONE', ( #5772, #9179, #2050, #2276 ) ) ;
#24752 = CARTESIAN_POINT ( 'NONE',  ( 15.99999999999998579, 144.9999999999999716, 187.0000000000000000 ) ) ;
#24753 = CYLINDRICAL_SURFACE ( 'NONE', #27244, 7.999999999999979572 ) ;
#24754 = AXIS2_PLACEMENT_3D ( 'NONE', #34087, #7194, #9701 ) ;
#24756 = DIRECTION ( 'NONE',  ( 1.000000000000000000, 3.040835319149746090E-31, -1.232595164407830946E-32 ) ) ;
#24755 = DIRECTION ( 'NONE',  ( 1.000000000000000000, 0.000000000000000000, 0.000000000000000000 ) ) ;
#24757 = VERTEX_POINT ( 'NONE', #27498 ) ;
#24758 = ORIENTED_EDGE ( 'NONE', *, *, #17990, .F. ) ;
#24759 = DIRECTION ( 'NONE',  ( -1.000000000000000000, 0.000000000000000000, 0.000000000000000000 ) ) ;
#24760 = LINE ( 'NONE', #1053, #17561 ) ;
#24761 = VECTOR ( 'NONE', #1143, 1000.000000000000000 ) ;
#24762 = DIRECTION ( 'NONE',  ( 0.000000000000000000, -1.000000000000000000, -2.132064625830773463E-16 ) ) ;
#24764 = ADVANCED_FACE ( 'NONE', ( #16849 ), #22167, .F. ) ;
#24763 = CARTESIAN_POINT ( 'NONE',  ( 8.485274312747506542, 31.41981051364776434, 49.43553178847298568 ) ) ;
#24765 = CARTESIAN_POINT ( 'NONE',  ( 2.765921099433442887, 24.20451283648829133, 19.51346322004938827 ) ) ;
#24766 = VERTEX_POINT ( 'NONE', #13989 ) ;
#24767 = CARTESIAN_POINT ( 'NONE',  ( 3.235562306570555532E-30, -1.691831803474588058, -87.50000000000000000 ) ) ;
#24768 = CARTESIAN_POINT ( 'NONE',  ( -12.00000000000001066, 144.9999999999999716, -194.9999999999999432 ) ) ;
#24769 = CARTESIAN_POINT ( 'NONE',  ( 2.604019747054050260, -16.26694784591052922, 27.88362116434737814 ) ) ;
#24770 = ORIENTED_EDGE ( 'NONE', *, *, #16300, .F. ) ;
#24771 = VECTOR ( 'NONE', #14070, 1000.000000000000000 ) ;
#24772 = DIRECTION ( 'NONE',  ( -1.000000000000000000, 0.000000000000000000, 0.000000000000000000 ) ) ;
#24773 = DIRECTION ( 'NONE',  ( 0.000000000000000000, 1.131431318426415506E-52, 1.000000000000000000 ) ) ;
#24774 = DIRECTION ( 'NONE',  ( 1.000000000000000000, 0.000000000000000000, 0.000000000000000000 ) ) ;
#24776 = CARTESIAN_POINT ( 'NONE',  ( -101.8759042855232479, 4.062957613056754624, -6.307943406627036786 ) ) ;
#24775 = CARTESIAN_POINT ( 'NONE',  ( 3.235562306570555532E-30, 4.168562732279004202, -67.50000000000000000 ) ) ;
#24777 = ADVANCED_FACE ( 'NONE', ( #24826 ), #11489, .T. ) ;
#24778 = ADVANCED_FACE ( 'NONE', ( #15645 ), #29154, .T. ) ;
#24779 = LINE ( 'NONE', #411, #18443 ) ;
#24780 = VERTEX_POINT ( 'NONE', #7959 ) ;
#24781 = CARTESIAN_POINT ( 'NONE',  ( 145.0000000000000568, -78.33668825982579165, -65.00000000000000000 ) ) ;
#24783 = DIRECTION ( 'NONE',  ( -1.000000000000000000, -0.000000000000000000, -0.000000000000000000 ) ) ;
#24782 = LINE ( 'NONE', #3589, #30878 ) ;
#24784 = AXIS2_PLACEMENT_3D ( 'NONE', #15408, #17574, #9544 ) ;
#24785 = ORIENTED_EDGE ( 'NONE', *, *, #8060, .F. ) ;
#24786 = VECTOR ( 'NONE', #32691, 1000.000000000000000 ) ;
#24787 = VERTEX_POINT ( 'NONE', #7780 ) ;
#24788 = EDGE_CURVE ( 'NONE', #30647, #33874, #10661, .T. ) ;
#24789 = EDGE_CURVE ( 'NONE', #22615, #11675, #12143, .T. ) ;
#24790 = ORIENTED_EDGE ( 'NONE', *, *, #16737, .F. ) ;
#24791 = CYLINDRICAL_SURFACE ( 'NONE', #25256, 7.999999999999979572 ) ;
#24792 = ORIENTED_EDGE ( 'NONE', *, *, #21309, .F. ) ;
#24793 = ORIENTED_EDGE ( 'NONE', *, *, #23079, .F. ) ;
#24794 = DIRECTION ( 'NONE',  ( 0.000000000000000000, 0.000000000000000000, -1.000000000000000000 ) ) ;
#24795 = VECTOR ( 'NONE', #10785, 1000.000000000000000 ) ;
#24796 = DIRECTION ( 'NONE',  ( 0.000000000000000000, 0.000000000000000000, 1.000000000000000000 ) ) ;
#24797 = DIRECTION ( 'NONE',  ( 0.9476531711828030113, 0.3193015301359780622, -0.000000000000000000 ) ) ;
#24798 = VERTEX_POINT ( 'NONE', #23976 ) ;
#24799 = ORIENTED_EDGE ( 'NONE', *, *, #21557, .F. ) ;
#24800 = DIRECTION ( 'NONE',  ( -0.000000000000000000, 1.836970198721029934E-16, -1.000000000000000000 ) ) ;
#24801 = CARTESIAN_POINT ( 'NONE',  ( -500.0000000000000000, -105.0000000000000142, 187.0000000000000000 ) ) ;
#24802 = CARTESIAN_POINT ( 'NONE',  ( -35.00000000000000000, 0.000000000000000000, 0.000000000000000000 ) ) ;
#24803 = DIRECTION ( 'NONE',  ( -1.000000000000000000, 0.000000000000000000, 0.000000000000000000 ) ) ;
#24804 = ORIENTED_EDGE ( 'NONE', *, *, #32135, .T. ) ;
#24805 = VECTOR ( 'NONE', #32767, 1000.000000000000000 ) ;
#24806 = CARTESIAN_POINT ( 'NONE',  ( 1.040000000000001368, 14.40815186467820652, -31.25366880301302785 ) ) ;
#24807 = DIRECTION ( 'NONE',  ( 1.000000000000000000, 0.000000000000000000, 1.300283923313630633E-47 ) ) ;
#24808 = ORIENTED_EDGE ( 'NONE', *, *, #9330, .F. ) ;
#24809 = AXIS2_PLACEMENT_3D ( 'NONE', #30909, #6689, #1184 ) ;
#24810 = DIRECTION ( 'NONE',  ( -0.3193015301359797276, 0.9476531711828024562, -0.000000000000000000 ) ) ;
#24812 = ADVANCED_FACE ( 'NONE', ( #28980 ), #4749, .F. ) ;
#24811 = CARTESIAN_POINT ( 'NONE',  ( 1.749999999999999778, 6.183021911001840287, 33.85493898757064812 ) ) ;
#24813 = LINE ( 'NONE', #19675, #24828 ) ;
#24814 = EDGE_CURVE ( 'NONE', #10259, #17236, #5105, .T. ) ;
#24815 = DIRECTION ( 'NONE',  ( -1.000000000000000000, 6.792721752314501023E-48, -3.697785493223492838E-32 ) ) ;
#24816 = ORIENTED_EDGE ( 'NONE', *, *, #15889, .T. ) ;
#24817 = EDGE_CURVE ( 'NONE', #24914, #19693, #4570, .T. ) ;
#24818 = CARTESIAN_POINT ( 'NONE',  ( 18.63894936814906345, 26.67946662374789213, 49.43553178847298568 ) ) ;
#24819 = VERTEX_POINT ( 'NONE', #29680 ) ;
#24821 = DIRECTION ( 'NONE',  ( -2.154935995002245207E-17, -0.000000000000000000, -1.000000000000000000 ) ) ;
#24820 = FACE_OUTER_BOUND ( 'NONE', #23115, .T. ) ;
#24822 = VECTOR ( 'NONE', #33901, 1000.000000000000000 ) ;
#24823 = EDGE_CURVE ( 'NONE', #5474, #26209, #22987, .T. ) ;
#24824 = EDGE_CURVE ( 'NONE', #32587, #20439, #20972, .T. ) ;
#24825 = VERTEX_POINT ( 'NONE', #34675 ) ;
#24826 = FACE_OUTER_BOUND ( 'NONE', #33082, .T. ) ;
#24827 = CARTESIAN_POINT ( 'NONE',  ( 1.040000000000001590, 27.68252950111337896, 20.44661865013498314 ) ) ;
#24828 = VECTOR ( 'NONE', #14156, 1000.000000000000000 ) ;
#24829 = EDGE_LOOP ( 'NONE', ( #31262, #34138, #9820, #11732 ) ) ;
#24830 = VECTOR ( 'NONE', #12654, 1000.000000000000000 ) ;
#24831 = AXIS2_PLACEMENT_3D ( 'NONE', #8161, #8346, #27212 ) ;
#24832 = ORIENTED_EDGE ( 'NONE', *, *, #34321, .F. ) ;
#24833 = CARTESIAN_POINT ( 'NONE',  ( 129.3530333899765594, 6.000000000000000000, 57.49999999999999289 ) ) ;
#24834 = CARTESIAN_POINT ( 'NONE',  ( -70.00000000000000000, 75.55999999999990280, 172.9900000000000091 ) ) ;
#24835 = EDGE_LOOP ( 'NONE', ( #20743, #2779, #26709, #4906 ) ) ;
#24836 = ORIENTED_EDGE ( 'NONE', *, *, #10157, .F. ) ;
#24837 = PLANE ( 'NONE',  #21256 ) ;
#24838 = CARTESIAN_POINT ( 'NONE',  ( 2.765921099433441999, -17.95514392185434360, 25.38201125280350468 ) ) ;
#24839 = CARTESIAN_POINT ( 'NONE',  ( 11.99999999999999645, 144.9999999999999716, 187.0000000000000000 ) ) ;
#24840 = DIRECTION ( 'NONE',  ( -1.000000000000000000, 0.000000000000000000, -5.546364386991661285E-52 ) ) ;
#24841 = VERTEX_POINT ( 'NONE', #21501 ) ;
#24842 = ORIENTED_EDGE ( 'NONE', *, *, #1007, .T. ) ;
#24843 = FACE_OUTER_BOUND ( 'NONE', #17222, .T. ) ;
#24844 = CARTESIAN_POINT ( 'NONE',  ( 15.99999999999998579, 75.55999999999990280, 172.9900000000000091 ) ) ;
#24845 = DIRECTION ( 'NONE',  ( 0.000000000000000000, 1.000000000000000000, 5.145227585319922065E-49 ) ) ;
#24846 = CARTESIAN_POINT ( 'NONE',  ( -418.0000000000000000, -112.9999999999999858, 155.0000000000000000 ) ) ;
#24847 = CARTESIAN_POINT ( 'NONE',  ( -0.2989565185775304723, 0.000000000000000000, 14.77500000000000036 ) ) ;
#24848 = AXIS2_PLACEMENT_3D ( 'NONE', #3999, #20056, #14725 ) ;
#24849 = CARTESIAN_POINT ( 'NONE',  ( 60.00000000000000000, 0.000000000000000000, 0.000000000000000000 ) ) ;
#24850 = CARTESIAN_POINT ( 'NONE',  ( 2.789999999999999147, 7.489092610871509237, -29.53582882395378562 ) ) ;
#24851 = ORIENTED_EDGE ( 'NONE', *, *, #21412, .F. ) ;
#24852 = DIRECTION ( 'NONE',  ( -0.000000000000000000, 1.000000000000000000, -0.000000000000000000 ) ) ;
#24853 = CARTESIAN_POINT ( 'NONE',  ( 2.789999999999999147, 3.909681563762101852, -30.21863799912378923 ) ) ;
#24854 = EDGE_CURVE ( 'NONE', #20519, #2835, #13785, .T. ) ;
#24855 = CARTESIAN_POINT ( 'NONE',  ( 1.749999999999999778, 0.000000000000000000, 0.000000000000000000 ) ) ;
#24856 = ORIENTED_EDGE ( 'NONE', *, *, #4286, .T. ) ;
#24857 = AXIS2_PLACEMENT_3D ( 'NONE', #1487, #18059, #15025 ) ;
#24858 = AXIS2_PLACEMENT_3D ( 'NONE', #751, #13579, #27267 ) ;
#24859 = EDGE_CURVE ( 'NONE', #24256, #4948, #31385, .T. ) ;
#24860 = DIRECTION ( 'NONE',  ( 1.000000000000000000, 0.000000000000000000, 0.000000000000000000 ) ) ;
#24861 = ORIENTED_EDGE ( 'NONE', *, *, #21204, .F. ) ;
#24862 = CARTESIAN_POINT ( 'NONE',  ( -418.0000000000000000, 124.9999999999999574, -190.9999999999999716 ) ) ;
#24863 = FACE_OUTER_BOUND ( 'NONE', #9509, .T. ) ;
#24864 = VECTOR ( 'NONE', #6721, 1000.000000000000000 ) ;
#24865 = EDGE_LOOP ( 'NONE', ( #24715, #25240, #6039, #18933 ) ) ;
#24866 = CARTESIAN_POINT ( 'NONE',  ( -410.0000000000000568, -105.0000000000000142, 187.0000000000000000 ) ) ;
#24867 = CARTESIAN_POINT ( 'NONE',  ( -12.00000000000001066, 124.9999999999999716, 159.0000000000000000 ) ) ;
#24868 = DIRECTION ( 'NONE',  ( 0.000000000000000000, 1.000000000000000000, -3.374343856708137958E-53 ) ) ;
#24869 = VERTEX_POINT ( 'NONE', #21325 ) ;
#24870 = VECTOR ( 'NONE', #9493, 1000.000000000000000 ) ;
#24871 = CARTESIAN_POINT ( 'NONE',  ( 846.4267198847176132, 1073.909424216847810, 1753.598338701303419 ) ) ;
#24872 = CARTESIAN_POINT ( 'NONE',  ( 2.789999999999999147, 9.869977788041397915, -30.37666815053925973 ) ) ;
#24873 = ORIENTED_EDGE ( 'NONE', *, *, #3359, .T. ) ;
#24874 = LINE ( 'NONE', #862, #18986 ) ;
#24875 = DIRECTION ( 'NONE',  ( -3.469446951953832974E-18, -1.000000000000000000, -7.888609052210116302E-31 ) ) ;
#24876 = CIRCLE ( 'NONE', #8958, 2.000000000000001776 ) ;
#24877 = AXIS2_PLACEMENT_3D ( 'NONE', #16927, #365, #2840 ) ;
#24878 = DIRECTION ( 'NONE',  ( 0.000000000000000000, 1.374038396813311798E-15, -1.000000000000000000 ) ) ;
#24879 = CARTESIAN_POINT ( 'NONE',  ( -100.5845299119079925, -2.602876666701936514, 7.039998176148507980 ) ) ;
#24880 = VERTEX_POINT ( 'NONE', #12971 ) ;
#24881 = ORIENTED_EDGE ( 'NONE', *, *, #3805, .T. ) ;
#24882 = ORIENTED_EDGE ( 'NONE', *, *, #13880, .T. ) ;
#24883 = CARTESIAN_POINT ( 'NONE',  ( -442.0000000000000000, -145.0000000000000000, -175.0000000000000000 ) ) ;
#24884 = CARTESIAN_POINT ( 'NONE',  ( 2.789999999999999147, -8.112136323388726922, -30.01377904834218668 ) ) ;
#24885 = AXIS2_PLACEMENT_3D ( 'NONE', #33519, #16644, #22499 ) ;
#24886 = DIRECTION ( 'NONE',  ( -1.000000000000000000, 0.000000000000000000, -1.300283923313630633E-47 ) ) ;
#24887 = ORIENTED_EDGE ( 'NONE', *, *, #22625, .T. ) ;
#24888 = ORIENTED_EDGE ( 'NONE', *, *, #30244, .T. ) ;
#24889 = CARTESIAN_POINT ( 'NONE',  ( 1.040000000000001146, 21.72796464722008025, 26.68861566460903134 ) ) ;
#24890 = EDGE_LOOP ( 'NONE', ( #9625, #21202, #4052, #8868, #22165, #21349, #4028, #17720 ) ) ;
#24891 = ADVANCED_FACE ( 'NONE', ( #33841 ), #1916, .F. ) ;
#24892 = DIRECTION ( 'NONE',  ( 0.000000000000000000, 0.000000000000000000, 1.000000000000000000 ) ) ;
#24893 = DIRECTION ( 'NONE',  ( 0.000000000000000000, 0.000000000000000000, 1.000000000000000000 ) ) ;
#24894 = ORIENTED_EDGE ( 'NONE', *, *, #19115, .T. ) ;
#24895 = ORIENTED_EDGE ( 'NONE', *, *, #22833, .T. ) ;
#24896 = CARTESIAN_POINT ( 'NONE',  ( 5.021133111224369117, -5.758675521474015291, -67.50000000000000000 ) ) ;
#24897 = EDGE_CURVE ( 'NONE', #30310, #8215, #33081, .T. ) ;
#24898 = FACE_OUTER_BOUND ( 'NONE', #18379, .T. ) ;
#24899 = ORIENTED_EDGE ( 'NONE', *, *, #21266, .T. ) ;
#24900 = PRODUCT_RELATED_PRODUCT_CATEGORY ( 'part', '', ( #27382 ) ) ;
#24901 = CARTESIAN_POINT ( 'NONE',  ( 1.224646799147352862E-15, 49.99999999999999289, 9.999999999999998224 ) ) ;
#24902 = CYLINDRICAL_SURFACE ( 'NONE', #21704, 2.525000000000001243 ) ;
#24903 = FACE_OUTER_BOUND ( 'NONE', #3419, .T. ) ;
#24904 = CARTESIAN_POINT ( 'NONE',  ( -499.9999999999999432, -113.0000000000000000, -187.0000000000000000 ) ) ;
#24905 = AXIS2_PLACEMENT_3D ( 'NONE', #9958, #6922, #31488 ) ;
#24906 =( REPRESENTATION_RELATIONSHIP ('NONE','NONE', #23037, #28231 ) REPRESENTATION_RELATIONSHIP_WITH_TRANSFORMATION ( #12690 )SHAPE_REPRESENTATION_RELATIONSHIP( ) );
#24907 = VECTOR ( 'NONE', #22403, 1000.000000000000000 ) ;
#24908 = CARTESIAN_POINT ( 'NONE',  ( -143.0000000000000568, -78.33668825982579165, -63.00000000000000000 ) ) ;
#24909 = DIRECTION ( 'NONE',  ( 1.000000000000000000, 0.000000000000000000, 0.000000000000000000 ) ) ;
#24910 = FILL_AREA_STYLE_COLOUR ( '', #5272 ) ;
#24911 = VECTOR ( 'NONE', #16428, 1000.000000000000000 ) ;
#24912 = ORIENTED_EDGE ( 'NONE', *, *, #19656, .F. ) ;
#24913 = DIRECTION ( 'NONE',  ( 0.1063910735368947813, -0.9943243633099144718, -3.335902418024520312E-15 ) ) ;
#24914 = VERTEX_POINT ( 'NONE', #12802 ) ;
#24915 = EDGE_LOOP ( 'NONE', ( #1583, #23571, #30834, #22838, #23233, #13031, #777, #17694 ) ) ;
#24916 = CARTESIAN_POINT ( 'NONE',  ( 2.765921099433440222, -27.96208973699893008, -13.59246946040217630 ) ) ;
#24917 = AXIS2_PLACEMENT_3D ( 'NONE', #19437, #5695, #32938 ) ;
#24918 = CARTESIAN_POINT ( 'NONE',  ( -35.55956070192387841, -12.65143121711728291, 5.690671783530174999 ) ) ;
#24919 = CONTEXT_DEPENDENT_SHAPE_REPRESENTATION ( #17621, #12090 ) ;
#24920 = ORIENTED_EDGE ( 'NONE', *, *, #11341, .F. ) ;
#24921 = DIRECTION ( 'NONE',  ( -1.000000000000000000, -0.000000000000000000, 0.000000000000000000 ) ) ;
#24922 = CONTEXT_DEPENDENT_SHAPE_REPRESENTATION ( #23777, #25280 ) ;
#24923 = CIRCLE ( 'NONE', #4461, 15.00000000000000000 ) ;
#24925 = CARTESIAN_POINT ( 'NONE',  ( 0.6763010051031069780, -1.505030548027689319, 3.180000000000000160 ) ) ;
#24924 = DIRECTION ( 'NONE',  ( 1.000000000000000000, 0.000000000000000000, 0.000000000000000000 ) ) ;
#24926 = ORIENTED_EDGE ( 'NONE', *, *, #11212, .T. ) ;
#24927 = EDGE_LOOP ( 'NONE', ( #28560, #1401, #26462, #2025 ) ) ;
#24928 = PLANE ( 'NONE',  #19143 ) ;
#24929 = ADVANCED_FACE ( 'NONE', ( #21143, #31990 ), #20797, .T. ) ;
#24930 = CARTESIAN_POINT ( 'NONE',  ( 0.000000000000000000, 0.000000000000000000, 3.180000000000000160 ) ) ;
#24931 = DIRECTION ( 'NONE',  ( -1.000000000000000000, -0.000000000000000000, -0.000000000000000000 ) ) ;
#24932 = DIRECTION ( 'NONE',  ( 0.000000000000000000, -1.000000000000000000, -1.836970198721029934E-16 ) ) ;
#24933 = ORIENTED_EDGE ( 'NONE', *, *, #34970, .T. ) ;
#24934 = VECTOR ( 'NONE', #19711, 1000.000000000000000 ) ;
#24935 = LINE ( 'NONE', #24767, #23747 ) ;
#24936 = DIRECTION ( 'NONE',  ( 1.848892746611746966E-32, -6.842277657836020854E-49, 1.000000000000000000 ) ) ;
#24937 = CARTESIAN_POINT ( 'NONE',  ( -365.0000000000000000, -131.0000000000000000, 130.0000000000000000 ) ) ;
#24938 = ORIENTED_EDGE ( 'NONE', *, *, #22625, .F. ) ;
#24939 = EDGE_CURVE ( 'NONE', #30502, #6669, #4931, .T. ) ;
#24940 = DIRECTION ( 'NONE',  ( -0.000000000000000000, -0.000000000000000000, -1.000000000000000000 ) ) ;
#24941 = CARTESIAN_POINT ( 'NONE',  ( -355.0000000000000000, 130.9999999999999716, 113.9999999999999858 ) ) ;
#24942 = ADVANCED_FACE ( 'NONE', ( #13840 ), #14357, .T. ) ;
#24943 = DIRECTION ( 'NONE',  ( 0.5155538571770218459, -0.8568571761675891629, 0.000000000000000000 ) ) ;
#24945 = DIRECTION ( 'NONE',  ( -1.000000000000000000, 0.000000000000000000, 0.000000000000000000 ) ) ;
#24944 = CARTESIAN_POINT ( 'NONE',  ( 0.000000000000000000, 3.524919873834583163E-15, 68.31122994652405112 ) ) ;
#24946 = AXIS2_PLACEMENT_3D ( 'NONE', #4002, #23410, #3661 ) ;
#24947 = ADVANCED_FACE ( 'NONE', ( #5460 ), #314, .T. ) ;
#24948 = EDGE_CURVE ( 'NONE', #17643, #8335, #27980, .T. ) ;
#24949 = DIRECTION ( 'NONE',  ( 0.1617819965527638737, 0.9868265225415262520, -0.000000000000000000 ) ) ;
#24950 = ORIENTED_EDGE ( 'NONE', *, *, #4561, .T. ) ;
#24951 = DIRECTION ( 'NONE',  ( 1.000000000000000000, 0.000000000000000000, 0.000000000000000000 ) ) ;
#24952 = DIRECTION ( 'NONE',  ( 0.000000000000000000, 0.000000000000000000, -1.000000000000000000 ) ) ;
#24953 = EDGE_CURVE ( 'NONE', #14854, #30600, #664, .T. ) ;
#24954 = AXIS2_PLACEMENT_3D ( 'NONE', #11868, #30181, #25184 ) ;
#24955 = ORIENTED_EDGE ( 'NONE', *, *, #12426, .T. ) ;
#24956 =( LENGTH_UNIT ( ) NAMED_UNIT ( * ) SI_UNIT ( .MILLI., .METRE. ) );
#24957 = VERTEX_POINT ( 'NONE', #16522 ) ;
#24958 = VECTOR ( 'NONE', #1363, 1000.000000000000114 ) ;
#24959 = ORIENTED_EDGE ( 'NONE', *, *, #25825, .T. ) ;
#24960 = CARTESIAN_POINT ( 'NONE',  ( -20.02113311122498729, -3.725253662474303784, -67.50000000000000000 ) ) ;
#24961 = ORIENTED_EDGE ( 'NONE', *, *, #10492, .T. ) ;
#24962 = ORIENTED_EDGE ( 'NONE', *, *, #7210, .F. ) ;
#24963 = CARTESIAN_POINT ( 'NONE',  ( 6.857172176539690689, 37.23415287044793587, 68.31122994652405112 ) ) ;
#24964 = CONTEXT_DEPENDENT_SHAPE_REPRESENTATION ( #6238, #26533 ) ;
#24965 = AXIS2_PLACEMENT_3D ( 'NONE', #19485, #3435, #30323 ) ;
#24966 = EDGE_LOOP ( 'NONE', ( #5174, #21003 ) ) ;
#24967 = DIRECTION ( 'NONE',  ( -1.000000000000000000, 0.000000000000000000, 0.000000000000000000 ) ) ;
#24968 = LINE ( 'NONE', #22140, #19420 ) ;
#24969 = VERTEX_POINT ( 'NONE', #11524 ) ;
#24970 = ORIENTED_EDGE ( 'NONE', *, *, #21600, .F. ) ;
#24971 = CARTESIAN_POINT ( 'NONE',  ( 28.11866956577617316, 16.38733641342591341, 49.43553178847298568 ) ) ;
#24972 = LINE ( 'NONE', #5741, #6131 ) ;
#24973 = CARTESIAN_POINT ( 'NONE',  ( 105.0034891410423512, -5.747432938596947594, -11.10030587185099726 ) ) ;
#24974 = DIRECTION ( 'NONE',  ( 0.000000000000000000, 0.000000000000000000, 1.000000000000000000 ) ) ;
#24975 = DIRECTION ( 'NONE',  ( 0.000000000000000000, -0.000000000000000000, 1.000000000000000000 ) ) ;
#24976 = VERTEX_POINT ( 'NONE', #2792 ) ;
#24977 = CARTESIAN_POINT ( 'NONE',  ( 0.02407890056655651728, 29.44518845714764765, 9.980709654879525772 ) ) ;
#24978 = CYLINDRICAL_SURFACE ( 'NONE', #2785, 5.115020388170798959 ) ;
#24979 = ORIENTED_EDGE ( 'NONE', *, *, #18852, .T. ) ;
#24980 = CARTESIAN_POINT ( 'NONE',  ( 0.000000000000000000, 3.524919873834583163E-15, 68.31122994652405112 ) ) ;
#24981 = DIRECTION ( 'NONE',  ( 0.000000000000000000, 0.000000000000000000, 1.000000000000000000 ) ) ;
#24982 = CARTESIAN_POINT ( 'NONE',  ( -442.0000000000000000, -104.9999999999999716, -187.0000000000000000 ) ) ;
#24983 = EDGE_CURVE ( 'NONE', #9821, #18812, #33038, .T. ) ;
#24984 = CARTESIAN_POINT ( 'NONE',  ( 0.02407890056655738464, -29.68817180695669578, -9.232883799364548949 ) ) ;
#24985 = CARTESIAN_POINT ( 'NONE',  ( -1.030735741678193262, 1.713938105891546382, 3.930000000000000160 ) ) ;
#24986 = EDGE_CURVE ( 'NONE', #493, #591, #18368, .T. ) ;
#24987 = EDGE_CURVE ( 'NONE', #27741, #24998, #29750, .T. ) ;
#24988 = CARTESIAN_POINT ( 'NONE',  ( -418.0000000000000000, -105.0000000000000142, 155.0000000000000000 ) ) ;
#24989 = ORIENTED_EDGE ( 'NONE', *, *, #14612, .F. ) ;
#24991 = CARTESIAN_POINT ( 'NONE',  ( 2.397606348813468014, 30.27116788627787614, 13.00174666746673324 ) ) ;
#24990 = CARTESIAN_POINT ( 'NONE',  ( -105.0000000000000000, 0.000000000000000000, 57.49999999999999289 ) ) ;
#24992 = ORIENTED_EDGE ( 'NONE', *, *, #22059, .T. ) ;
#24993 = DIRECTION ( 'NONE',  ( -0.000000000000000000, -0.000000000000000000, -1.000000000000000000 ) ) ;
#24994 = CARTESIAN_POINT ( 'NONE',  ( 27.64943126350854286, -17.16721653852534146, 68.31122994652405112 ) ) ;
#24995 = B_SPLINE_CURVE_WITH_KNOTS ( 'NONE', 3,
 ( #5352, #16772, #32581, #19089 ),
 .UNSPECIFIED., .F., .F.,
 ( 4, 4 ),
 ( 0.005298360586756124813, 0.005985229062776062023 ),
 .UNSPECIFIED. ) ;
#24996 = ORIENTED_EDGE ( 'NONE', *, *, #11270, .F. ) ;
#24997 = ADVANCED_FACE ( 'NONE', ( #10989 ), #32695, .T. ) ;
#24998 = VERTEX_POINT ( 'NONE', #33223 ) ;
#24999 = CARTESIAN_POINT ( 'NONE',  ( -5.021133111225196011, -23.57973016998034765, -87.50000000000000000 ) ) ;
#25000 = DIRECTION ( 'NONE',  ( 1.000000000000000000, -0.000000000000000000, -0.000000000000000000 ) ) ;
#25001 = ORIENTED_EDGE ( 'NONE', *, *, #22117, .T. ) ;
#25002 = ORIENTED_EDGE ( 'NONE', *, *, #20580, .F. ) ;
#25003 = DIRECTION ( 'NONE',  ( 0.3193015301359796165, -0.9476531711828025673, 0.000000000000000000 ) ) ;
#25004 = EDGE_CURVE ( 'NONE', #16210, #18812, #11175, .T. ) ;
#25005 = AXIS2_PLACEMENT_3D ( 'NONE', #4462, #7850, #18039 ) ;
#25006 = EDGE_CURVE ( 'NONE', #594, #15054, #14019, .T. ) ;
#25007 = FACE_OUTER_BOUND ( 'NONE', #27, .T. ) ;
#25008 = EDGE_CURVE ( 'NONE', #392, #5864, #16699, .T. ) ;
#25009 = CARTESIAN_POINT ( 'NONE',  ( 2.765921099433443331, 14.63235270440974922, -27.43224275967423509 ) ) ;
#25010 = CARTESIAN_POINT ( 'NONE',  ( 0.000000000000000000, 27.60935207499572996, -12.89090262359622585 ) ) ;
#25011 = VERTEX_POINT ( 'NONE', #30201 ) ;
#25012 = VERTEX_POINT ( 'NONE', #2965 ) ;
#25013 = DIRECTION ( 'NONE',  ( -4.043477172016612439E-17, 0.000000000000000000, -1.000000000000000000 ) ) ;
#25014 = CARTESIAN_POINT ( 'NONE',  ( -9.978866888775527855, 8.235406450278427215, -67.50000000000000000 ) ) ;
#25015 = DIRECTION ( 'NONE',  ( 0.000000000000000000, 0.000000000000000000, 1.000000000000000000 ) ) ;
#25016 = ADVANCED_FACE ( 'NONE', ( #13489 ), #22024, .T. ) ;
#25017 = DIRECTION ( 'NONE',  ( 0.000000000000000000, 5.145227585319922065E-49, 1.000000000000000000 ) ) ;
#25018 = CARTESIAN_POINT ( 'NONE',  ( -410.0000000000000568, 105.0000000000000000, 132.0000000000000000 ) ) ;
#25019 = DIRECTION ( 'NONE',  ( -1.000000000000000000, -0.000000000000000000, -0.000000000000000000 ) ) ;
#25020 = DIRECTION ( 'NONE',  ( -0.000000000000000000, 0.000000000000000000, 1.000000000000000000 ) ) ;
#25021 = ORIENTED_EDGE ( 'NONE', *, *, #17689, .F. ) ;
#25022 = DIRECTION ( 'NONE',  ( 1.000000000000000000, 0.000000000000000000, 0.000000000000000000 ) ) ;
#25023 = DIRECTION ( 'NONE',  ( -0.000000000000000000, 1.836970198721029934E-16, -1.000000000000000000 ) ) ;
#25024 = DIRECTION ( 'NONE',  ( -1.000000000000000000, -0.000000000000000000, -0.000000000000000000 ) ) ;
#25025 = ORIENTED_EDGE ( 'NONE', *, *, #33140, .F. ) ;
#25026 = EDGE_CURVE ( 'NONE', #20230, #15534, #14385, .T. ) ;
#25027 = DIRECTION ( 'NONE',  ( 0.000000000000000000, -1.000000000000000000, -5.145227585319922065E-49 ) ) ;
#25028 = ORIENTED_EDGE ( 'NONE', *, *, #16538, .F. ) ;
#25029 = CIRCLE ( 'NONE', #23964, 4.306175033202026547 ) ;
#25030 = CARTESIAN_POINT ( 'NONE',  ( -414.0000000000000568, -105.0000000000000142, -77.99999999999997158 ) ) ;
#25031 = CARTESIAN_POINT ( 'NONE',  ( 7.700000000000001954, 0.000000000000000000, -9.999999999999994671 ) ) ;
#25032 = VECTOR ( 'NONE', #15628, 1000.000000000000000 ) ;
#25033 = ORIENTED_EDGE ( 'NONE', *, *, #27882, .T. ) ;
#25034 = DIRECTION ( 'NONE',  ( 0.000000000000000000, 0.000000000000000000, -1.000000000000000000 ) ) ;
#25035 = CARTESIAN_POINT ( 'NONE',  ( -119.9999999999997726, 0.000000000000000000, 0.000000000000000000 ) ) ;
#25036 = CARTESIAN_POINT ( 'NONE',  ( 0.02407890056655738464, -29.68817180695669578, -9.232883799364548949 ) ) ;
#25037 = ORIENTED_EDGE ( 'NONE', *, *, #25438, .F. ) ;
#25038 = AXIS2_PLACEMENT_3D ( 'NONE', #6106, #33350, #8971 ) ;
#25039 = CARTESIAN_POINT ( 'NONE',  ( 838.1282206682737979, 1151.466682316647393, 1753.598338701303419 ) ) ;
#25040 = AXIS2_PLACEMENT_3D ( 'NONE', #29997, #26445, #32307 ) ;
#25041 = VECTOR ( 'NONE', #14910, 1000.000000000000227 ) ;
#25042 = DIRECTION ( 'NONE',  ( 0.000000000000000000, 0.000000000000000000, -1.000000000000000000 ) ) ;
#25043 = ORIENTED_EDGE ( 'NONE', *, *, #11464, .T. ) ;
#25044 = LINE ( 'NONE', #25405, #23517 ) ;
#25045 = EDGE_CURVE ( 'NONE', #2161, #2852, #8491, .T. ) ;
#25046 = EDGE_CURVE ( 'NONE', #13531, #5849, #25528, .T. ) ;
#25047 = FACE_BOUND ( 'NONE', #19848, .T. ) ;
#25048 = CARTESIAN_POINT ( 'NONE',  ( 187.4264068711928530, -12.50000000000001066, 1.224646799147353217E-14 ) ) ;
#25049 = ORIENTED_EDGE ( 'NONE', *, *, #9092, .T. ) ;
#25050 = EDGE_LOOP ( 'NONE', ( #15831, #34643 ) ) ;
#25051 = ORIENTED_EDGE ( 'NONE', *, *, #559, .T. ) ;
#25052 = VECTOR ( 'NONE', #15947, 1000.000000000000114 ) ;
#25053 = SURFACE_SIDE_STYLE ('',( #33430 ) ) ;
#25055 = VECTOR ( 'NONE', #28403, 1000.000000000000000 ) ;
#25054 = FACE_OUTER_BOUND ( 'NONE', #26181, .T. ) ;
#25056 = CYLINDRICAL_SURFACE ( 'NONE', #5949, 5.738084889453667792 ) ;
#25057 = ORIENTED_EDGE ( 'NONE', *, *, #17632, .F. ) ;
#25058 = VERTEX_POINT ( 'NONE', #33400 ) ;
#25059 = CARTESIAN_POINT ( 'NONE',  ( 2.783128938602190683, -17.88422427744433207, -25.16112242373455032 ) ) ;
#25060 = ORIENTED_EDGE ( 'NONE', *, *, #26759, .T. ) ;
#25061 = EDGE_CURVE ( 'NONE', #13784, #31329, #20069, .T. ) ;
#25062 = FACE_OUTER_BOUND ( 'NONE', #16582, .T. ) ;
#25063 = FACE_OUTER_BOUND ( 'NONE', #18253, .T. ) ;
#25064 = ORIENTED_EDGE ( 'NONE', *, *, #24126, .T. ) ;
#25065 = ORIENTED_EDGE ( 'NONE', *, *, #28804, .T. ) ;
#25066 = DIRECTION ( 'NONE',  ( 1.000000000000000000, 0.000000000000000000, 0.000000000000000000 ) ) ;
#25067 = VECTOR ( 'NONE', #19401, 1000.000000000000000 ) ;
#25068 = VECTOR ( 'NONE', #23340, 1000.000000000000000 ) ;
#25070 = AXIS2_PLACEMENT_3D ( 'NONE', #4161, #15050, #7177 ) ;
#25069 = CARTESIAN_POINT ( 'NONE',  ( 2.765921099433442443, 29.44518845714779332, -9.980709654879110104 ) ) ;
#25071 = ORIENTED_EDGE ( 'NONE', *, *, #14727, .F. ) ;
#25072 = VECTOR ( 'NONE', #24773, 1000.000000000000000 ) ;
#25073 = DIRECTION ( 'NONE',  ( -0.000000000000000000, -1.000000000000000000, -0.000000000000000000 ) ) ;
#25074 = CARTESIAN_POINT ( 'NONE',  ( 0.000000000000000000, 1.974842713994612024E-15, 76.74945698428001606 ) ) ;
#25075 = CARTESIAN_POINT ( 'NONE',  ( 2.789999999999999147, 18.92047747027389448, -23.84508255125831866 ) ) ;
#25076 = CARTESIAN_POINT ( 'NONE',  ( -34.04247984038124031, 16.56841925338180488, 68.31122994652405112 ) ) ;
#25077 = CARTESIAN_POINT ( 'NONE',  ( -110.1067333817248226, -0.3368495349214609136, 12.49660185505138976 ) ) ;
#25078 = DIRECTION ( 'NONE',  ( 0.000000000000000000, -1.000000000000000000, 6.123233995736766036E-17 ) ) ;
#25080 = ADVANCED_FACE ( 'NONE', ( #17586 ), #9197, .F. ) ;
#25079 = VECTOR ( 'NONE', #18751, 1000.000000000000000 ) ;
#25081 = CARTESIAN_POINT ( 'NONE',  ( -445.9999999999999432, 105.0000000000000142, 187.0000000000000000 ) ) ;
#25082 = ORIENTED_EDGE ( 'NONE', *, *, #3366, .T. ) ;
#25083 = AXIS2_PLACEMENT_3D ( 'NONE', #4825, #2996, #14232 ) ;
#25084 = EDGE_LOOP ( 'NONE', ( #10440, #17064, #14441, #27299 ) ) ;
#25085 = DIRECTION ( 'NONE',  ( 0.1063910735368947813, -0.9943243633099144718, -3.335902418024520312E-15 ) ) ;
#25086 = ORIENTED_EDGE ( 'NONE', *, *, #21210, .T. ) ;
#25087 = ORIENTED_EDGE ( 'NONE', *, *, #26719, .T. ) ;
#25088 = EDGE_CURVE ( 'NONE', #11373, #1125, #17417, .T. ) ;
#25089 = ADVANCED_FACE ( 'NONE', ( #1186 ), #9024, .F. ) ;
#25090 = CYLINDRICAL_SURFACE ( 'NONE', #27758, 11.22499999999999787 ) ;
#25091 = EDGE_CURVE ( 'NONE', #17595, #22671, #12241, .T. ) ;
#25092 = CIRCLE ( 'NONE', #34200, 7.999999999999979572 ) ;
#25093 = CARTESIAN_POINT ( 'NONE',  ( 106.5405508486335293, 5.530628908288163004, 5.066456342206738128 ) ) ;
#25094 = PRODUCT_CONTEXT ( 'NONE', #7809, 'mechanical' ) ;
#25095 = ORIENTED_EDGE ( 'NONE', *, *, #8840, .T. ) ;
#25096 = VECTOR ( 'NONE', #4574, 1000.000000000000000 ) ;
#25097 = DIRECTION ( 'NONE',  ( 1.000000000000000000, 0.000000000000000000, 0.000000000000000000 ) ) ;
#25098 = CARTESIAN_POINT ( 'NONE',  ( -110.1150203881707483, -0.3417625387765728107, -12.49999999999999822 ) ) ;
#25100 = CARTESIAN_POINT ( 'NONE',  ( 19.99999999999998224, -115.0000000000000000, -158.9999999999999716 ) ) ;
#25099 = CARTESIAN_POINT ( 'NONE',  ( 0.02407890056655608360, 29.44518845714779332, -9.980709654879110104 ) ) ;
#25101 = VERTEX_POINT ( 'NONE', #14738 ) ;
#25102 = VERTEX_POINT ( 'NONE', #12409 ) ;
#25103 = DIRECTION ( 'NONE',  ( 0.000000000000000000, 1.836970198721029441E-16, -1.000000000000000000 ) ) ;
#25104 = CARTESIAN_POINT ( 'NONE',  ( -442.0000000000000000, 137.0000000000000000, -175.0000000000000000 ) ) ;
#25105 = CARTESIAN_POINT ( 'NONE',  ( -499.9999999999999432, 144.9999999999999716, -187.0000000000000000 ) ) ;
#25106 = DIRECTION ( 'NONE',  ( 0.000000000000000000, 0.000000000000000000, 1.000000000000000000 ) ) ;
#25107 = ORIENTED_EDGE ( 'NONE', *, *, #35084, .F. ) ;
#25108 = AXIS2_PLACEMENT_3D ( 'NONE', #29140, #9750, #23634 ) ;
#25109 = DIRECTION ( 'NONE',  ( 0.02866416272524433678, 0.5286793732840951998, 0.8483374835754913246 ) ) ;
#25110 = LINE ( 'NONE', #3574, #11167 ) ;
#25111 = CYLINDRICAL_SURFACE ( 'NONE', #10618, 10.00000000000000000 ) ;
#25112 =( REPRESENTATION_RELATIONSHIP ('NONE','NONE', #23037, #15767 ) REPRESENTATION_RELATIONSHIP_WITH_TRANSFORMATION ( #16021 )SHAPE_REPRESENTATION_RELATIONSHIP( ) );
#25113 = PRODUCT_DEFINITION_SHAPE ( 'NONE', 'NONE',  #764 ) ;
#25114 = ORIENTED_EDGE ( 'NONE', *, *, #30669, .F. ) ;
#25115 = DIRECTION ( 'NONE',  ( 0.1081190184239433222, 0.9941379571543594862, 1.826201800709962632E-16 ) ) ;
#25116 = CARTESIAN_POINT ( 'NONE',  ( -499.9999999999999432, 112.9999999999999574, 187.0000000000000000 ) ) ;
#25117 = FACE_BOUND ( 'NONE', #26661, .T. ) ;
#25120 = LINE ( 'NONE', #9291, #14564 ) ;
#25119 = DIRECTION ( 'NONE',  ( 1.000000000000000000, 0.000000000000000000, 0.000000000000000000 ) ) ;
#25118 = VECTOR ( 'NONE', #4065, 1000.000000000000000 ) ;
#25121 = AXIS2_PLACEMENT_3D ( 'NONE', #10862, #24016, #18545 ) ;
#25122 = AXIS2_PLACEMENT_3D ( 'NONE', #25643, #10285, #1272 ) ;
#25123 = FACE_OUTER_BOUND ( 'NONE', #9517, .T. ) ;
#25124 = VERTEX_POINT ( 'NONE', #14558 ) ;
#25125 = LINE ( 'NONE', #4107, #15066 ) ;
#25126 = DIRECTION ( 'NONE',  ( 1.000000000000000000, 0.000000000000000000, -1.232595164407831220E-32 ) ) ;
#25127 = ORIENTED_EDGE ( 'NONE', *, *, #25267, .F. ) ;
#25128 = ADVANCED_FACE ( 'NONE', ( #9380, #25560 ), #25924, .T. ) ;
#25129 = ORIENTED_EDGE ( 'NONE', *, *, #32215, .F. ) ;
#25130 = ADVANCED_FACE ( 'NONE', ( #9715 ), #30734, .F. ) ;
#25131 = EDGE_CURVE ( 'NONE', #32765, #34117, #33756, .T. ) ;
#25132 = ORIENTED_EDGE ( 'NONE', *, *, #11713, .T. ) ;
#25133 = PLANE ( 'NONE',  #9344 ) ;
#25134 = EDGE_LOOP ( 'NONE', ( #19512, #31816, #3939, #30174, #2192, #17431, #28047, #4795 ) ) ;
#25135 = EDGE_LOOP ( 'NONE', ( #7064, #31363, #16416, #532, #20904 ) ) ;
#25136 = EDGE_CURVE ( 'NONE', #1617, #23519, #20245, .T. ) ;
#25137 = DIRECTION ( 'NONE',  ( 1.000000000000000000, 0.000000000000000000, -1.848892746611746966E-32 ) ) ;
#25138 = B_SPLINE_CURVE_WITH_KNOTS ( 'NONE', 3,
 ( #674, #19725, #28071, #14746, #16890, #14567 ),
 .UNSPECIFIED., .F., .F.,
 ( 4, 2, 4 ),
 ( 4.404817011119805222E-07, 0.001874269612720299216, 0.003748098743739486718 ),
 .UNSPECIFIED. ) ;
#25140 = AXIS2_PLACEMENT_3D ( 'NONE', #1198, #12076, #33770 ) ;
#25139 = ITEM_DEFINED_TRANSFORMATION ( 'NONE', 'NONE', #185,  #28566 ) ;
#25141 = ORIENTED_EDGE ( 'NONE', *, *, #17734, .F. ) ;
#25142 = LINE ( 'NONE', #4641, #23767 ) ;
#25143 = AXIS2_PLACEMENT_3D ( 'NONE', #6738, #28110, #31297 ) ;
#25144 = LINE ( 'NONE', #19478, #12583 ) ;
#25145 = EDGE_LOOP ( 'NONE', ( #3166, #517, #27673, #6896, #12431, #27043 ) ) ;
#25146 = AXIS2_PLACEMENT_3D ( 'NONE', #51, #10917, #32611 ) ;
#25147 = ORIENTED_EDGE ( 'NONE', *, *, #12125, .T. ) ;
#25148 = VECTOR ( 'NONE', #31944, 1000.000000000000000 ) ;
#25149 = DIRECTION ( 'NONE',  ( 0.000000000000000000, 0.000000000000000000, 1.000000000000000000 ) ) ;
#25150 = CARTESIAN_POINT ( 'NONE',  ( 3.235562306570555532E-30, 18.16264470403145381, -87.50000000000000000 ) ) ;
#25151 = ADVANCED_FACE ( 'NONE', ( #23260 ), #34099, .F. ) ;
#25152 = CARTESIAN_POINT ( 'NONE',  ( 108.5055490898496373, -4.557852096327890123, -11.64155778436300182 ) ) ;
#25153 = FACE_OUTER_BOUND ( 'NONE', #3192, .T. ) ;
#25154 = CYLINDRICAL_SURFACE ( 'NONE', #9748, 4.000000000000003553 ) ;
#25155 = VERTEX_POINT ( 'NONE', #11887 ) ;
#25156 = EDGE_CURVE ( 'NONE', #34303, #12264, #30565, .T. ) ;
#25157 = DIRECTION ( 'NONE',  ( 0.000000000000000000, 0.000000000000000000, 1.000000000000000000 ) ) ;
#25158 = DIRECTION ( 'NONE',  ( -1.000000000000000000, 0.000000000000000000, 0.000000000000000000 ) ) ;
#25159 = EDGE_LOOP ( 'NONE', ( #29120, #12469, #24222, #26229 ) ) ;
#25160 = CARTESIAN_POINT ( 'NONE',  ( 145.0000000000000568, -12.50000000000001066, 1.224646799147353217E-14 ) ) ;
#25161 = CARTESIAN_POINT ( 'NONE',  ( 2.789999999999999147, -29.69698570178027808, 11.75786841620004175 ) ) ;
#25162 = FACE_OUTER_BOUND ( 'NONE', #34011, .T. ) ;
#25163 = LINE ( 'NONE', #17546, #17263 ) ;
#25164 = CARTESIAN_POINT ( 'NONE',  ( -10.00000000000000000, 0.000000000000000000, 0.000000000000000000 ) ) ;
#25165 = FACE_OUTER_BOUND ( 'NONE', #8343, .T. ) ;
#25166 = ORIENTED_EDGE ( 'NONE', *, *, #30283, .F. ) ;
#25167 = CARTESIAN_POINT ( 'NONE',  ( -15.99999999999998579, 4.559999999999908127, -177.7400000000000091 ) ) ;
#25169 = DIRECTION ( 'NONE',  ( -0.000000000000000000, 1.000000000000000000, -0.000000000000000000 ) ) ;
#25168 = FACE_OUTER_BOUND ( 'NONE', #4336, .T. ) ;
#25170 = AXIS2_PLACEMENT_3D ( 'NONE', #15310, #1595, #25618 ) ;
#25172 = VERTEX_POINT ( 'NONE', #14381 ) ;
#25171 = AXIS2_PLACEMENT_3D ( 'NONE', #30737, #21458, #29112 ) ;
#25173 = AXIS2_PLACEMENT_3D ( 'NONE', #30300, #11438, #19643 ) ;
#25174 = AXIS2_PLACEMENT_3D ( 'NONE', #29425, #4846, #34237 ) ;
#25175 = LINE ( 'NONE', #14351, #31956 ) ;
#25176 = DIRECTION ( 'NONE',  ( -1.000000000000000000, -0.000000000000000000, -0.000000000000000000 ) ) ;
#25177 = ORIENTED_EDGE ( 'NONE', *, *, #19622, .F. ) ;
#25178 = ORIENTED_EDGE ( 'NONE', *, *, #30977, .F. ) ;
#25179 = CARTESIAN_POINT ( 'NONE',  ( -26.18205399241666953, -19.33143609808337615, 68.31122994652405112 ) ) ;
#25180 = ORIENTED_EDGE ( 'NONE', *, *, #33044, .T. ) ;
#25181 = ORIENTED_EDGE ( 'NONE', *, *, #14842, .F. ) ;
#25182 = CARTESIAN_POINT ( 'NONE',  ( 3.235562306570555532E-30, 1.325223266901699007E-14, -67.50000000000000000 ) ) ;
#25183 = ADVANCED_FACE ( 'NONE', ( #14905 ), #25384, .T. ) ;
#25184 = DIRECTION ( 'NONE',  ( 0.000000000000000000, 0.000000000000000000, 1.000000000000000000 ) ) ;
#25185 = AXIS2_PLACEMENT_3D ( 'NONE', #9329, #1323, #25879 ) ;
#25186 = DIRECTION ( 'NONE',  ( 0.000000000000000000, 0.000000000000000000, 1.000000000000000000 ) ) ;
#25187 = DIRECTION ( 'NONE',  ( -1.848892746611746966E-32, 6.842277657836020854E-49, -1.000000000000000000 ) ) ;
#25188 = EDGE_CURVE ( 'NONE', #20076, #20682, #28570, .T. ) ;
#25189 = ORIENTED_EDGE ( 'NONE', *, *, #23466, .T. ) ;
#25190 = ADVANCED_FACE ( 'NONE', ( #25740 ), #33571, .F. ) ;
#25191 = EDGE_LOOP ( 'NONE', ( #13247, #1953, #3292, #16726, #14127, #24014, #21539, #11604 ) ) ;
#25192 = DIRECTION ( 'NONE',  ( 0.000000000000000000, 0.000000000000000000, -1.000000000000000000 ) ) ;
#25193 = CARTESIAN_POINT ( 'NONE',  ( 2.719051678778256154, 12.21437217961392818, -29.24586132675238304 ) ) ;
#25194 = DIRECTION ( 'NONE',  ( -0.7621620551276359068, 0.6473862847818281363, 0.000000000000000000 ) ) ;
#25195 = DIRECTION ( 'NONE',  ( 0.000000000000000000, 1.836970198721029441E-16, -1.000000000000000000 ) ) ;
#25196 = DIRECTION ( 'NONE',  ( -1.000000000000000000, 0.000000000000000000, 0.000000000000000000 ) ) ;
#25197 = AXIS2_PLACEMENT_3D ( 'NONE', #859, #32712, #6353 ) ;
#25198 = DIRECTION ( 'NONE',  ( 0.000000000000000000, 0.000000000000000000, 1.000000000000000000 ) ) ;
#25199 = VECTOR ( 'NONE', #1329, 1000.000000000000000 ) ;
#25200 = VECTOR ( 'NONE', #12846, 1000.000000000000000 ) ;
#25201 = CARTESIAN_POINT ( 'NONE',  ( 2.765921099433442443, 7.350529080603967813, -30.20932655202929595 ) ) ;
#25202 = ORIENTED_EDGE ( 'NONE', *, *, #12158, .T. ) ;
#25203 = DIRECTION ( 'NONE',  ( 0.000000000000000000, 2.309213040847544338E-50, 1.000000000000000000 ) ) ;
#25204 = CARTESIAN_POINT ( 'NONE',  ( -418.0000000000000000, 105.0000000000000142, 194.9999999999999716 ) ) ;
#25205 = EDGE_CURVE ( 'NONE', #27282, #23416, #7381, .T. ) ;
#25206 = DIRECTION ( 'NONE',  ( 1.000000000000000000, 0.000000000000000000, 0.000000000000000000 ) ) ;
#25207 = ORIENTED_EDGE ( 'NONE', *, *, #25061, .F. ) ;
#25208 = CARTESIAN_POINT ( 'NONE',  ( -143.0000000000000568, -97.49999999999998579, 63.00000000000000000 ) ) ;
#25209 = ORIENTED_EDGE ( 'NONE', *, *, #10348, .T. ) ;
#25210 = DIRECTION ( 'NONE',  ( 1.000000000000000000, 3.040835319149746090E-31, 1.232595164407830946E-32 ) ) ;
#25211 = DIRECTION ( 'NONE',  ( 1.000000000000000000, 0.000000000000000000, 0.000000000000000000 ) ) ;
#25212 = ADVANCED_FACE ( 'NONE', ( #1708 ), #29110, .T. ) ;
#25213 = AXIS2_PLACEMENT_3D ( 'NONE', #18580, #14640, #8742 ) ;
#25214 = EDGE_CURVE ( 'NONE', #32572, #23243, #9811, .T. ) ;
#25215 = VERTEX_POINT ( 'NONE', #15957 ) ;
#25216 = DIRECTION ( 'NONE',  ( -0.000000000000000000, -0.000000000000000000, 1.000000000000000000 ) ) ;
#25217 = DIRECTION ( 'NONE',  ( 0.000000000000000000, 1.836970198721029688E-16, -1.000000000000000000 ) ) ;
#25218 = CARTESIAN_POINT ( 'NONE',  ( -20.02113311122488781, 6.201984591278717041, -67.50000000000000000 ) ) ;
#25219 = EDGE_LOOP ( 'NONE', ( #665, #19253, #15979 ) ) ;
#25220 = PRODUCT_DEFINITION_FORMATION_WITH_SPECIFIED_SOURCE ( 'ANY', '', #32778, .NOT_KNOWN. ) ;
#25221 = VECTOR ( 'NONE', #33895, 1000.000000000000000 ) ;
#25222 = DIRECTION ( 'NONE',  ( 2.631201909438060585E-14, -5.396010391056496978E-16, 1.000000000000000000 ) ) ;
#25223 = AXIS2_PLACEMENT_3D ( 'NONE', #33716, #12203, #15044 ) ;
#25224 = CARTESIAN_POINT ( 'NONE',  ( -418.0000000000000000, -125.0000000000000000, 107.9999999999999858 ) ) ;
#25225 = ORIENTED_EDGE ( 'NONE', *, *, #3162, .T. ) ;
#25226 = CARTESIAN_POINT ( 'NONE',  ( -9.978866888775733912, -15.68591377522703390, -87.50000000000000000 ) ) ;
#25227 = CARTESIAN_POINT ( 'NONE',  ( 19.99999999999998934, 75.55999999999990280, -177.7400000000000091 ) ) ;
#25228 = PLANE ( 'NONE',  #33242 ) ;
#25229 = CARTESIAN_POINT ( 'NONE',  ( -6.500000000000000000, 0.000000000000000000, 0.000000000000000000 ) ) ;
#25230 = EDGE_CURVE ( 'NONE', #27211, #13630, #12575, .T. ) ;
#25231 = ORIENTED_EDGE ( 'NONE', *, *, #32141, .T. ) ;
#25232 = EDGE_CURVE ( 'NONE', #16675, #33409, #16083, .T. ) ;
#25233 = ORIENTED_EDGE ( 'NONE', *, *, #11055, .F. ) ;
#25234 = EDGE_LOOP ( 'NONE', ( #16965, #19513, #32451, #1141 ) ) ;
#25235 = ADVANCED_FACE ( 'NONE', ( #29293, #20757, #31603 ), #18273, .T. ) ;
#25236 = LINE ( 'NONE', #19746, #23942 ) ;
#25237 = B_SPLINE_CURVE_WITH_KNOTS ( 'NONE', 3,
 ( #8546, #9056, #30765, #30598 ),
 .UNSPECIFIED., .F., .F.,
 ( 4, 4 ),
 ( 2.010610498844524495E-07, 0.0006879367828356808224 ),
 .UNSPECIFIED. ) ;
#25238 = CARTESIAN_POINT ( 'NONE',  ( -355.0000000000000000, 118.9999999999999716, 113.9999999999999858 ) ) ;
#25239 = CARTESIAN_POINT ( 'NONE',  ( 3.235562306570555532E-30, -15.68591377522703390, -87.50000000000000000 ) ) ;
#25240 = ORIENTED_EDGE ( 'NONE', *, *, #13051, .F. ) ;
#25241 = ORIENTED_EDGE ( 'NONE', *, *, #24939, .F. ) ;
#25242 = FACE_OUTER_BOUND ( 'NONE', #13988, .T. ) ;
#25243 = ORIENTED_EDGE ( 'NONE', *, *, #6012, .F. ) ;
#25244 = AXIS2_PLACEMENT_3D ( 'NONE', #734, #28138, #33472 ) ;
#25245 = CARTESIAN_POINT ( 'NONE',  ( -442.0000000000000000, 141.0000000000000000, 154.9999999999999716 ) ) ;
#25246 = CARTESIAN_POINT ( 'NONE',  ( 107.5583909155902802, 5.149687040066284638, 11.39104704602384466 ) ) ;
#25247 = ORIENTED_EDGE ( 'NONE', *, *, #29604, .T. ) ;
#25248 = ORIENTED_EDGE ( 'NONE', *, *, #15022, .F. ) ;
#25249 = ORIENTED_EDGE ( 'NONE', *, *, #18902, .F. ) ;
#25250 = VECTOR ( 'NONE', #20538, 1000.000000000000000 ) ;
#25251 = VECTOR ( 'NONE', #32566, 1000.000000000000000 ) ;
#25252 = CARTESIAN_POINT ( 'NONE',  ( -414.0000000000000568, 105.0000000000000142, 107.9999999999999858 ) ) ;
#25253 = VERTEX_POINT ( 'NONE', #26437 ) ;
#25254 = DIRECTION ( 'NONE',  ( -1.000000000000000000, 0.000000000000000000, 0.000000000000000000 ) ) ;
#25256 = AXIS2_PLACEMENT_3D ( 'NONE', #32620, #13598, #10925 ) ;
#25255 = DIRECTION ( 'NONE',  ( -0.9766205557100871015, -0.2149704402110223789, -0.000000000000000000 ) ) ;
#25257 = CARTESIAN_POINT ( 'NONE',  ( -418.0000000000000000, -124.9999999999999716, 135.9999999999999716 ) ) ;
#25258 = EDGE_CURVE ( 'NONE', #14266, #7431, #34634, .T. ) ;
#25259 = CARTESIAN_POINT ( 'NONE',  ( -442.0000000000000000, -112.9999999999999858, 155.0000000000000000 ) ) ;
#25260 = EDGE_CURVE ( 'NONE', #20441, #14635, #13278, .T. ) ;
#25261 = CARTESIAN_POINT ( 'NONE',  ( -106.3407376400858055, -4.947629808455843659, 11.47938275244241524 ) ) ;
#25262 = DIRECTION ( 'NONE',  ( -1.000000000000000000, -3.469446951953834515E-18, 0.000000000000000000 ) ) ;
#25263 = CARTESIAN_POINT ( 'NONE',  ( -499.9999999999999432, 140.9999999999999716, -162.9999999999999716 ) ) ;
#25264 = EDGE_CURVE ( 'NONE', #17516, #19142, #18627, .T. ) ;
#25265 = VERTEX_POINT ( 'NONE', #10071 ) ;
#25266 = VECTOR ( 'NONE', #16634, 999.9999999999998863 ) ;
#25267 = EDGE_CURVE ( 'NONE', #6559, #29898, #34993, .T. ) ;
#25268 = ORIENTED_EDGE ( 'NONE', *, *, #26747, .T. ) ;
#25269 = DIRECTION ( 'NONE',  ( 2.631201909438060269E-14, -5.396010391056495992E-16, 0.9999999999999998890 ) ) ;
#25270 = EDGE_CURVE ( 'NONE', #3925, #17170, #21098, .T. ) ;
#25271 = ORIENTED_EDGE ( 'NONE', *, *, #5243, .F. ) ;
#25272 = VECTOR ( 'NONE', #1397, 1000.000000000000000 ) ;
#25273 = VERTEX_POINT ( 'NONE', #5064 ) ;
#25274 = DIRECTION ( 'NONE',  ( 0.7071067811865512365, 0.000000000000000000, -0.7071067811865439090 ) ) ;
#25275 = LINE ( 'NONE', #3741, #20383 ) ;
#25276 = CIRCLE ( 'NONE', #1979, 7.999999999999979572 ) ;
#25277 = DIRECTION ( 'NONE',  ( 0.000000000000000000, 0.000000000000000000, 1.000000000000000000 ) ) ;
#25278 = VECTOR ( 'NONE', #32521, 1000.000000000000000 ) ;
#25279 = EDGE_LOOP ( 'NONE', ( #26965, #15079, #8419, #3568, #26186, #17994, #28664, #18815, #11898, #16958, #26786, #27394 ) ) ;
#25280 = PRODUCT_DEFINITION_SHAPE ( 'NONE', 'NONE',  #35232 ) ;
#25281 = CARTESIAN_POINT ( 'NONE',  ( 8.000000000000000000, 0.000000000000000000, 0.000000000000000000 ) ) ;
#25283 = CARTESIAN_POINT ( 'NONE',  ( -499.9999999999999432, 112.9999999999999574, 159.0000000000000000 ) ) ;
#25282 = DIRECTION ( 'NONE',  ( 0.000000000000000000, 1.131431318426415506E-52, 1.000000000000000000 ) ) ;
#25284 = VERTEX_POINT ( 'NONE', #7559 ) ;
#25285 = ORIENTED_EDGE ( 'NONE', *, *, #626, .F. ) ;
#25286 = CYLINDRICAL_SURFACE ( 'NONE', #33329, 7.999999999999979572 ) ;
#25287 = EDGE_CURVE ( 'NONE', #5322, #20352, #18452, .T. ) ;
#25288 = CARTESIAN_POINT ( 'NONE',  ( 11.99999999999999645, 144.9999999999999716, 162.9999999999999716 ) ) ;
#25289 = LINE ( 'NONE', #32772, #13123 ) ;
#25290 = CARTESIAN_POINT ( 'NONE',  ( -418.0000000000000000, 113.0000000000000000, 154.9999999999999716 ) ) ;
#25291 = ORIENTED_EDGE ( 'NONE', *, *, #3094, .T. ) ;
#25292 = CARTESIAN_POINT ( 'NONE',  ( 2.033589661826324946, 31.72524275137189065, 11.99054900124222200 ) ) ;
#25293 = CIRCLE ( 'NONE', #15662, 10.00000000000000000 ) ;
#25294 = LINE ( 'NONE', #927, #6634 ) ;
#25295 = B_SPLINE_CURVE_WITH_KNOTS ( 'NONE', 3,
 ( #9938, #31640, #30381, #10529 ),
 .UNSPECIFIED., .F., .F.,
 ( 4, 4 ),
 ( 2.702373194995073782E-07, 0.0006880065385067164448 ),
 .UNSPECIFIED. ) ;
#25296 = ORIENTED_EDGE ( 'NONE', *, *, #25258, .T. ) ;
#25297 = VECTOR ( 'NONE', #8309, 1000.000000000000000 ) ;
#25298 = DIRECTION ( 'NONE',  ( 1.000000000000000000, 0.000000000000000000, 0.000000000000000000 ) ) ;
#25299 = ADVANCED_FACE ( 'NONE', ( #12759 ), #29469, .F. ) ;
#25300 = LINE ( 'NONE', #11430, #32465 ) ;
#25301 = PLANE ( 'NONE',  #5298 ) ;
#25302 = EDGE_CURVE ( 'NONE', #32722, #31704, #31430, .T. ) ;
#25304 = DIRECTION ( 'NONE',  ( 0.000000000000000000, 1.000000000000000000, 1.224646799147353207E-16 ) ) ;
#25303 = FACE_OUTER_BOUND ( 'NONE', #30884, .T. ) ;
#25305 = EDGE_CURVE ( 'NONE', #31468, #23190, #15515, .T. ) ;
#25306 = VECTOR ( 'NONE', #14747, 1000.000000000000227 ) ;
#25307 = UNCERTAINTY_MEASURE_WITH_UNIT (LENGTH_MEASURE( 1.000000000000000082E-05 ), #22116, 'distance_accuracy_value', 'NONE');
#25308 = CARTESIAN_POINT ( 'NONE',  ( -12.00000000000001066, -137.0000000000000000, 174.9999999999999432 ) ) ;
#25309 = CARTESIAN_POINT ( 'NONE',  ( -345.0000000000000000, -135.0000000000000000, 113.9999999999999858 ) ) ;
#25310 = ORIENTED_EDGE ( 'NONE', *, *, #13303, .F. ) ;
#25311 = LINE ( 'NONE', #6079, #22422 ) ;
#25312 = FACE_OUTER_BOUND ( 'NONE', #3721, .T. ) ;
#25313 = PRESENTATION_LAYER_ASSIGNMENT (  '', '', ( #5405 ) ) ;
#25314 = ORIENTED_EDGE ( 'NONE', *, *, #17997, .T. ) ;
#25315 = ORIENTED_EDGE ( 'NONE', *, *, #23910, .F. ) ;
#25316 = CIRCLE ( 'NONE', #27024, 34.41491905851385269 ) ;
#25317 = EDGE_LOOP ( 'NONE', ( #6466, #7848, #24458, #9031 ) ) ;
#25318 = CARTESIAN_POINT ( 'NONE',  ( -37.12776225901827587, -7.411627343331159246, 15.81122994652406355 ) ) ;
#25319 = ORIENTED_EDGE ( 'NONE', *, *, #234, .T. ) ;
#25320 = ORIENTED_EDGE ( 'NONE', *, *, #11761, .T. ) ;
#25321 = FACE_OUTER_BOUND ( 'NONE', #4295, .T. ) ;
#25322 = VECTOR ( 'NONE', #3617, 999.9999999999998863 ) ;
#25323 = EDGE_LOOP ( 'NONE', ( #30314, #34497, #21668, #2296 ) ) ;
#25324 = DIRECTION ( 'NONE',  ( 0.000000000000000000, -1.000000000000000000, -2.132064625830773463E-16 ) ) ;
#25325 = CARTESIAN_POINT ( 'NONE',  ( -32.32899628990712415, -3.747048406849366131, 68.31122994652405112 ) ) ;
#25326 = ORIENTED_EDGE ( 'NONE', *, *, #32034, .T. ) ;
#25327 = ORIENTED_EDGE ( 'NONE', *, *, #33828, .T. ) ;
#25328 = CARTESIAN_POINT ( 'NONE',  ( -0.7181323043387224381, -1.866624223957557671, 4.679999999999999716 ) ) ;
#25329 = LINE ( 'NONE', #32810, #18669 ) ;
#25330 = AXIS2_PLACEMENT_3D ( 'NONE', #11804, #11434, #3930 ) ;
#25331 = DIRECTION ( 'NONE',  ( 0.000000000000000000, 1.836970198721029934E-16, -1.000000000000000000 ) ) ;
#25332 = CYLINDRICAL_SURFACE ( 'NONE', #19376, 2.524999999999999467 ) ;
#25333 = DIRECTION ( 'NONE',  ( -1.000000000000000000, 0.000000000000000000, -5.546364386991661285E-52 ) ) ;
#25334 = ORIENTED_EDGE ( 'NONE', *, *, #5437, .F. ) ;
#25335 = FACE_OUTER_BOUND ( 'NONE', #15009, .T. ) ;
#25336 = LINE ( 'NONE', #12009, #19860 ) ;
#25337 = VERTEX_POINT ( 'NONE', #15251 ) ;
#25338 = PLANE ( 'NONE',  #25892 ) ;
#25339 = CARTESIAN_POINT ( 'NONE',  ( -8.000000000000000000, 1.809415645740213944E-15, 14.77499999999999858 ) ) ;
#25340 = EDGE_CURVE ( 'NONE', #17624, #7371, #26091, .T. ) ;
#25341 = LINE ( 'NONE', #9674, #20652 ) ;
#25342 = CARTESIAN_POINT ( 'NONE',  ( 99.46174900952425446, 1.550744593849150865, -7.348056298371736794 ) ) ;
#25343 = CARTESIAN_POINT ( 'NONE',  ( 11.99999999999999645, 124.9999999999999716, 162.9999999999999716 ) ) ;
#25344 = CIRCLE ( 'NONE', #23103, 3.999999999999989786 ) ;
#25345 = EDGE_CURVE ( 'NONE', #19221, #22410, #34277, .T. ) ;
#25346 = DIRECTION ( 'NONE',  ( -1.000000000000000000, 0.000000000000000000, -0.000000000000000000 ) ) ;
#25347 = ORIENTED_EDGE ( 'NONE', *, *, #2512, .F. ) ;
#25348 = EDGE_CURVE ( 'NONE', #34651, #34913, #26782, .T. ) ;
#25349 = CARTESIAN_POINT ( 'NONE',  ( 0.000000000000000000, 20.79173593595294633, -22.27454621808743340 ) ) ;
#25351 = DIRECTION ( 'NONE',  ( 1.000000000000000000, -0.000000000000000000, -0.000000000000000000 ) ) ;
#25350 = CARTESIAN_POINT ( 'NONE',  ( 10.00000000000000000, 0.000000000000000000, 0.000000000000000000 ) ) ;
#25352 = AXIS2_PLACEMENT_3D ( 'NONE', #27090, #3402, #11425 ) ;
#25353 = EDGE_LOOP ( 'NONE', ( #6431, #812, #6247, #24213, #7032, #3522, #12107 ) ) ;
#25354 = LINE ( 'NONE', #17204, #24504 ) ;
#25355 = VECTOR ( 'NONE', #7566, 1000.000000000000000 ) ;
#25356 = EDGE_CURVE ( 'NONE', #22871, #5175, #32540, .T. ) ;
#25357 = VERTEX_POINT ( 'NONE', #2923 ) ;
#25358 = VERTEX_POINT ( 'NONE', #24628 ) ;
#25359 = B_SPLINE_CURVE_WITH_KNOTS ( 'NONE', 3,
 ( #15867, #2662, #9975, #31674 ),
 .UNSPECIFIED., .F., .F.,
 ( 4, 4 ),
 ( 2.250995564674948756E-07, 0.0006879610227481868607 ),
 .UNSPECIFIED. ) ;
#25360 = ORIENTED_EDGE ( 'NONE', *, *, #3910, .T. ) ;
#25361 = LINE ( 'NONE', #993, #29307 ) ;
#25362 = ORIENTED_EDGE ( 'NONE', *, *, #20336, .T. ) ;
#25363 = ORIENTED_EDGE ( 'NONE', *, *, #20498, .F. ) ;
#25364 = CARTESIAN_POINT ( 'NONE',  ( -430.0000000000000000, 114.9999999999999716, 126.0000000000000000 ) ) ;
#25365 = PRODUCT_DEFINITION_SHAPE ( 'NONE', 'NONE',  #35168 ) ;
#25366 = LINE ( 'NONE', #27511, #2776 ) ;
#25367 = CIRCLE ( 'NONE', #31075, 1.999999999999999112 ) ;
#25368 = CARTESIAN_POINT ( 'NONE',  ( 1.749999999999999778, 21.72796464722008380, 26.68861566460903489 ) ) ;
#25369 = DIRECTION ( 'NONE',  ( 0.000000000000000000, 0.000000000000000000, 1.000000000000000000 ) ) ;
#25370 = ORIENTED_EDGE ( 'NONE', *, *, #17441, .F. ) ;
#25371 = ORIENTED_EDGE ( 'NONE', *, *, #1250, .F. ) ;
#25372 = DIRECTION ( 'NONE',  ( 0.000000000000000000, 0.000000000000000000, 1.000000000000000000 ) ) ;
#25373 = FACE_OUTER_BOUND ( 'NONE', #31487, .T. ) ;
#25374 = DIRECTION ( 'NONE',  ( 0.000000000000000000, 0.8486862100397269959, -0.5288966977476834419 ) ) ;
#25375 = AXIS2_PLACEMENT_3D ( 'NONE', #24980, #24624, #17187 ) ;
#25376 = CYLINDRICAL_SURFACE ( 'NONE', #5044, 7.999999999999979572 ) ;
#25377 = DIRECTION ( 'NONE',  ( 0.000000000000000000, -1.000000000000000000, -2.465190328815662439E-32 ) ) ;
#25378 = PLANE ( 'NONE',  #21899 ) ;
#25379 = LINE ( 'NONE', #17230, #11886 ) ;
#25380 = ORIENTED_EDGE ( 'NONE', *, *, #31080, .F. ) ;
#25381 = FACE_OUTER_BOUND ( 'NONE', #3996, .T. ) ;
#25382 = CARTESIAN_POINT ( 'NONE',  ( 9.199999999999999289, -15.58845726811992627, 0.000000000000000000 ) ) ;
#25383 = ADVANCED_FACE ( 'NONE', ( #2750 ), #22159, .F. ) ;
#25384 = CYLINDRICAL_SURFACE ( 'NONE', #161, 1.999999999999999556 ) ;
#25385 = ORIENTED_EDGE ( 'NONE', *, *, #3408, .F. ) ;
#25386 = DIRECTION ( 'NONE',  ( -0.000000000000000000, 1.000000000000000000, -0.000000000000000000 ) ) ;
#25387 = VERTEX_POINT ( 'NONE', #24450 ) ;
#25388 = EDGE_CURVE ( 'NONE', #6490, #29803, #17240, .T. ) ;
#25389 = DIRECTION ( 'NONE',  ( 1.000000000000000000, 0.000000000000000000, 0.000000000000000000 ) ) ;
#25390 = CARTESIAN_POINT ( 'NONE',  ( -103.1830246108492162, 4.784316299155410235, 11.54838096230724176 ) ) ;
#25391 = ADVANCED_FACE ( 'NONE', ( #89 ), #21455, .F. ) ;
#25392 = VECTOR ( 'NONE', #22937, 1000.000000000000000 ) ;
#25393 = EDGE_LOOP ( 'NONE', ( #5395, #14679, #25049, #18840 ) ) ;
#25394 = ADVANCED_FACE ( 'NONE', ( #11306 ), #27664, .F. ) ;
#25395 = EDGE_CURVE ( 'NONE', #10505, #5999, #31985, .T. ) ;
#25396 = CARTESIAN_POINT ( 'NONE',  ( -500.0000000000000000, -105.0000000000000142, 187.0000000000000000 ) ) ;
#25397 = FACE_OUTER_BOUND ( 'NONE', #8898, .T. ) ;
#25398 = PLANE ( 'NONE',  #14380 ) ;
#25399 = EDGE_CURVE ( 'NONE', #18391, #25708, #30154, .T. ) ;
#25400 = ORIENTED_EDGE ( 'NONE', *, *, #20487, .F. ) ;
#25401 = CARTESIAN_POINT ( 'NONE',  ( 784.3543876670810278, 1081.231670447986289, 1753.598338701303419 ) ) ;
#25402 = CIRCLE ( 'NONE', #17493, 30.47050528711512030 ) ;
#25403 = LINE ( 'NONE', #4027, #31795 ) ;
#25404 = ORIENTED_EDGE ( 'NONE', *, *, #34834, .F. ) ;
#25405 = CARTESIAN_POINT ( 'NONE',  ( 4.815661544189684840, -32.18716788982703747, -36.68877005347593467 ) ) ;
#25406 = CARTESIAN_POINT ( 'NONE',  ( -110.1150203881707910, -7.176976838982289656E-16, -12.50000000000000000 ) ) ;
#25407 = DIRECTION ( 'NONE',  ( -0.000000000000000000, -0.000000000000000000, 1.000000000000000000 ) ) ;
#25408 = DIRECTION ( 'NONE',  ( 0.000000000000000000, 1.000000000000000000, 1.934419779023891545E-16 ) ) ;
#25409 = CONTEXT_DEPENDENT_SHAPE_REPRESENTATION ( #16046, #29082 ) ;
#25410 = ORIENTED_EDGE ( 'NONE', *, *, #30215, .T. ) ;
#25411 = VERTEX_POINT ( 'NONE', #16841 ) ;
#25412 = VERTEX_POINT ( 'NONE', #18795 ) ;
#25413 = PRODUCT_DEFINITION_SHAPE ( 'NONE', 'NONE',  #35103 ) ;
#25414 = B_SPLINE_CURVE_WITH_KNOTS ( 'NONE', 3,
 ( #34480, #28962, #31627, #23799, #34300, #34658 ),
 .UNSPECIFIED., .F., .F.,
 ( 4, 2, 4 ),
 ( 4.404817051637942833E-07, 0.001874269637237883143, 0.003748098792770602258 ),
 .UNSPECIFIED. ) ;
#25415 = SURFACE_STYLE_USAGE ( .BOTH. , #25053 ) ;
#25416 = AXIS2_PLACEMENT_3D ( 'NONE', #14425, #11569, #14062 ) ;
#25417 = DIRECTION ( 'NONE',  ( 5.546364386991661285E-52, 0.000000000000000000, -1.000000000000000000 ) ) ;
#25418 = VECTOR ( 'NONE', #2958, 1000.000000000000000 ) ;
#25419 = AXIS2_PLACEMENT_3D ( 'NONE', #9468, #20153, #25823 ) ;
#25420 = DIRECTION ( 'NONE',  ( 0.000000000000000000, 1.000000000000000000, 5.145227585319922065E-49 ) ) ;
#25421 = CARTESIAN_POINT ( 'NONE',  ( 143.0000000000000568, -173.5121282296299796, -41.09364177412887642 ) ) ;
#25422 = ORIENTED_EDGE ( 'NONE', *, *, #17997, .F. ) ;
#25423 = DIRECTION ( 'NONE',  ( 3.697785493223492838E-32, 1.934419779023891545E-16, -1.000000000000000000 ) ) ;
#25424 = DIRECTION ( 'NONE',  ( 0.000000000000000000, 0.000000000000000000, -1.000000000000000000 ) ) ;
#25425 = ORIENTED_EDGE ( 'NONE', *, *, #10650, .F. ) ;
#25426 = CYLINDRICAL_SURFACE ( 'NONE', #10093, 13.50000000000000178 ) ;
#25427 = CARTESIAN_POINT ( 'NONE',  ( 0.1859802676143585964, 30.43784769162285997, -10.75394592869476895 ) ) ;
#25428 = ORIENTED_EDGE ( 'NONE', *, *, #1294, .T. ) ;
#25429 = ORIENTED_EDGE ( 'NONE', *, *, #565, .F. ) ;
#25430 = FACE_OUTER_BOUND ( 'NONE', #16039, .T. ) ;
#25431 = DIRECTION ( 'NONE',  ( 0.000000000000000000, 1.131431318426415506E-52, 1.000000000000000000 ) ) ;
#25432 = VERTEX_POINT ( 'NONE', #5757 ) ;
#25433 = DIRECTION ( 'NONE',  ( -0.000000000000000000, -0.000000000000000000, 1.000000000000000000 ) ) ;
#25434 = CARTESIAN_POINT ( 'NONE',  ( -430.0000000000000000, -131.0000000000000000, 130.0000000000000000 ) ) ;
#25435 = DIRECTION ( 'NONE',  ( -1.000000000000000000, 0.000000000000000000, 0.000000000000000000 ) ) ;
#25436 = CIRCLE ( 'NONE', #8950, 7.999999999999979572 ) ;
#25437 = ADVANCED_FACE ( 'NONE', ( #29637 ), #5233, .F. ) ;
#25438 = EDGE_CURVE ( 'NONE', #2751, #7906, #13450, .T. ) ;
#25439 = CARTESIAN_POINT ( 'NONE',  ( -101.6198087930189757, -3.853301823223607592, 11.89378582241138993 ) ) ;
#25440 = CARTESIAN_POINT ( 'NONE',  ( 21.17270648470164218, -7.613573412837960852, 20.00000000000000000 ) ) ;
#25441 = ORIENTED_EDGE ( 'NONE', *, *, #4199, .F. ) ;
#25442 = AXIS2_PLACEMENT_3D ( 'NONE', #32598, #21748, #403 ) ;
#25443 = VECTOR ( 'NONE', #29910, 1000.000000000000000 ) ;
#25444 = ORIENTED_EDGE ( 'NONE', *, *, #16448, .F. ) ;
#25445 = DIRECTION ( 'NONE',  ( 2.631201909438060269E-14, -5.396010391056495992E-16, 0.9999999999999998890 ) ) ;
#25446 = ORIENTED_EDGE ( 'NONE', *, *, #28202, .F. ) ;
#25447 = ORIENTED_EDGE ( 'NONE', *, *, #5715, .F. ) ;
#25448 = EDGE_CURVE ( 'NONE', #22312, #33375, #27464, .T. ) ;
#25449 = VECTOR ( 'NONE', #9370, 1000.000000000000000 ) ;
#25450 = DIRECTION ( 'NONE',  ( -1.000000000000000000, -0.000000000000000000, -0.000000000000000000 ) ) ;
#25451 = LINE ( 'NONE', #11776, #29002 ) ;
#25452 = ORIENTED_EDGE ( 'NONE', *, *, #16963, .F. ) ;
#25453 = DIRECTION ( 'NONE',  ( 0.000000000000000000, -1.131431318426415506E-52, -1.000000000000000000 ) ) ;
#25454 = EDGE_CURVE ( 'NONE', #32497, #797, #18739, .T. ) ;
#25455 = EDGE_CURVE ( 'NONE', #30400, #14739, #34281, .T. ) ;
#25456 = EDGE_CURVE ( 'NONE', #30822, #20910, #29815, .T. ) ;
#25458 = CYLINDRICAL_SURFACE ( 'NONE', #6139, 16.19999999999999218 ) ;
#25457 = CARTESIAN_POINT ( 'NONE',  ( 2.765921099433441999, -17.95514392185434360, 25.38201125280350468 ) ) ;
#25459 = AXIS2_PLACEMENT_3D ( 'NONE', #2379, #24086, #21436 ) ;
#25460 = ORIENTED_EDGE ( 'NONE', *, *, #17386, .F. ) ;
#25461 = VERTEX_POINT ( 'NONE', #13797 ) ;
#25462 = DIRECTION ( 'NONE',  ( -1.000000000000000000, -0.000000000000000000, -0.000000000000000000 ) ) ;
#25463 = EDGE_CURVE ( 'NONE', #22350, #31793, #25163, .T. ) ;
#25464 = LINE ( 'NONE', #12137, #14790 ) ;
#25465 = CARTESIAN_POINT ( 'NONE',  ( 129.3530333899765594, 6.000000000000000000, 62.49999999999999289 ) ) ;
#25466 = CARTESIAN_POINT ( 'NONE',  ( -418.0000000000000000, 137.0000000000000000, -175.0000000000000000 ) ) ;
#25467 = EDGE_LOOP ( 'NONE', ( #27501, #13975, #26841, #1066 ) ) ;
#25469 = CARTESIAN_POINT ( 'NONE',  ( 44.94043929807611448, -32.65143121711728469, 20.00000000000000000 ) ) ;
#25468 = VECTOR ( 'NONE', #23834, 1000.000000000000000 ) ;
#25470 = CARTESIAN_POINT ( 'NONE',  ( 9.199999999999999289, 13.50000000000000178, 0.000000000000000000 ) ) ;
#25471 = CIRCLE ( 'NONE', #8421, 30.47050528711512030 ) ;
#25472 = ORIENTED_EDGE ( 'NONE', *, *, #13945, .T. ) ;
#25473 = PLANE ( 'NONE',  #22027 ) ;
#25474 = DIRECTION ( 'NONE',  ( 0.000000000000000000, 0.000000000000000000, 1.000000000000000000 ) ) ;
#25475 = DIRECTION ( 'NONE',  ( 0.000000000000000000, 0.000000000000000000, 1.000000000000000000 ) ) ;
#25476 = CIRCLE ( 'NONE', #18121, 32.54542015209055705 ) ;
#25478 = DIRECTION ( 'NONE',  ( 0.000000000000000000, 1.836970198721029441E-16, -1.000000000000000000 ) ) ;
#25477 = LINE ( 'NONE', #12150, #262 ) ;
#25479 = EDGE_CURVE ( 'NONE', #19022, #26110, #3577, .T. ) ;
#25480 = FACE_OUTER_BOUND ( 'NONE', #10990, .T. ) ;
#25481 = CARTESIAN_POINT ( 'NONE',  ( -361.0000000000000000, -135.0000000000000000, 110.0000000000000000 ) ) ;
#25482 = EDGE_LOOP ( 'NONE', ( #32728, #15133, #31973, #5839 ) ) ;
#25483 = B_SPLINE_CURVE_WITH_KNOTS ( 'NONE', 3,
 ( #28262, #3689, #33057, #1206 ),
 .UNSPECIFIED., .F., .F.,
 ( 4, 4 ),
 ( 4.077050493238060077E-07, 0.0006881451559005274379 ),
 .UNSPECIFIED. ) ;
#25484 = DIRECTION ( 'NONE',  ( 0.000000000000000000, 0.000000000000000000, 1.000000000000000000 ) ) ;
#25485 = CARTESIAN_POINT ( 'NONE',  ( 0.000000000000000000, -29.91351748324100512, -5.799410679710955030 ) ) ;
#25486 = AXIS2_PLACEMENT_3D ( 'NONE', #5495, #3186, #14058 ) ;
#25487 = VECTOR ( 'NONE', #33304, 1000.000000000000000 ) ;
#25488 = VERTEX_POINT ( 'NONE', #8981 ) ;
#25489 = VERTEX_POINT ( 'NONE', #11481 ) ;
#25490 = AXIS2_PLACEMENT_3D ( 'NONE', #18134, #7402, #26114 ) ;
#25491 = ORIENTED_EDGE ( 'NONE', *, *, #6773, .T. ) ;
#25492 = DIRECTION ( 'NONE',  ( 1.000000000000000000, 0.000000000000000000, 0.000000000000000000 ) ) ;
#25493 = ORIENTED_EDGE ( 'NONE', *, *, #15005, .F. ) ;
#25494 = ORIENTED_EDGE ( 'NONE', *, *, #25008, .T. ) ;
#25495 = DIRECTION ( 'NONE',  ( -0.000000000000000000, 1.000000000000000000, -0.000000000000000000 ) ) ;
#25496 = VECTOR ( 'NONE', #34490, 1000.000000000000000 ) ;
#25497 = EDGE_CURVE ( 'NONE', #28134, #34702, #31387, .T. ) ;
#25498 = CONTEXT_DEPENDENT_SHAPE_REPRESENTATION ( #11517, #8177 ) ;
#25499 = EDGE_CURVE ( 'NONE', #29646, #22648, #20205, .T. ) ;
#25500 = ORIENTED_EDGE ( 'NONE', *, *, #29938, .T. ) ;
#25501 = DIRECTION ( 'NONE',  ( 0.000000000000000000, 0.000000000000000000, 1.000000000000000000 ) ) ;
#25502 = DIRECTION ( 'NONE',  ( 0.9868265225415260300, 0.1617819965527648174, 0.000000000000000000 ) ) ;
#25503 = ORIENTED_EDGE ( 'NONE', *, *, #20323, .F. ) ;
#25504 = ORIENTED_EDGE ( 'NONE', *, *, #5822, .T. ) ;
#25505 = CARTESIAN_POINT ( 'NONE',  ( 0.000000000000000000, 3.214697847761802057E-14, -87.50000000000000000 ) ) ;
#25506 = DIRECTION ( 'NONE',  ( 0.000000000000000000, 5.053935297177146739E-49, 1.000000000000000000 ) ) ;
#25507 = CARTESIAN_POINT ( 'NONE',  ( -418.0000000000000000, -105.0000000000000142, 155.0000000000000568 ) ) ;
#25508 = LINE ( 'NONE', #17877, #2888 ) ;
#25509 = DIRECTION ( 'NONE',  ( 0.000000000000000000, 0.000000000000000000, 1.000000000000000000 ) ) ;
#25510 = EDGE_LOOP ( 'NONE', ( #5705, #4680, #24096, #12139 ) ) ;
#25511 = CARTESIAN_POINT ( 'NONE',  ( 10.00000000000000000, 15.58845726811990673, -2.400813222210650817E-15 ) ) ;
#25512 = CARTESIAN_POINT ( 'NONE',  ( 11.99999999999999645, -124.9999999999999432, -190.9999999999999432 ) ) ;
#25513 = CIRCLE ( 'NONE', #19846, 3.999999999999976019 ) ;
#25514 = CARTESIAN_POINT ( 'NONE',  ( 17.27856612038528894, 33.69708579775584667, -36.68877005347592757 ) ) ;
#25515 = ORIENTED_EDGE ( 'NONE', *, *, #25550, .T. ) ;
#25516 = DIRECTION ( 'NONE',  ( 0.000000000000000000, -1.224646799147353207E-16, 1.000000000000000000 ) ) ;
#25517 = CARTESIAN_POINT ( 'NONE',  ( -442.0000000000000000, 104.9999999999999858, 154.9999999999999716 ) ) ;
#25518 = DIRECTION ( 'NONE',  ( 0.7621620551276362399, 0.6473862847818278032, 0.000000000000000000 ) ) ;
#25519 = CARTESIAN_POINT ( 'NONE',  ( 103.6432141880921876, 5.578687132273540961, -5.013157219915588492 ) ) ;
#25521 = LINE ( 'NONE', #9515, #31013 ) ;
#25520 = DIRECTION ( 'NONE',  ( 0.000000000000000000, 0.000000000000000000, 1.000000000000000000 ) ) ;
#25522 = COLOUR_RGB ( '',0.7921568627450980005, 0.8196078431372548767, 0.9333333333333333481 ) ;
#25523 = CARTESIAN_POINT ( 'NONE',  ( -37.12776225901827587, -7.411627343331159246, 68.31122994652405112 ) ) ;
#25524 = VERTEX_POINT ( 'NONE', #9513 ) ;
#25525 = CARTESIAN_POINT ( 'NONE',  ( -19.99999999999998934, -145.0000000000000000, 187.0000000000000000 ) ) ;
#25527 = DIRECTION ( 'NONE',  ( 0.000000000000000000, -0.000000000000000000, -1.000000000000000000 ) ) ;
#25526 = DIRECTION ( 'NONE',  ( -0.6876994588534234287, 0.7259954919231307313, 1.333632083068605180E-16 ) ) ;
#25528 = B_SPLINE_CURVE_WITH_KNOTS ( 'NONE', 3,
 ( #10500, #10818, #5799, #21665, #16351, #27181, #13657, #1018 ),
 .UNSPECIFIED., .F., .F.,
 ( 4, 2, 2, 4 ),
 ( 0.03601148258275851249, 0.03996050705323227203, 0.04193501928846914834, 0.04390953152370602464 ),
 .UNSPECIFIED. ) ;
#25529 = ORIENTED_EDGE ( 'NONE', *, *, #4581, .T. ) ;
#25530 = DIRECTION ( 'NONE',  ( -0.8854131517428555087, 0.2458337514780908895, -0.3944734685057937895 ) ) ;
#25531 = VERTEX_POINT ( 'NONE', #20372 ) ;
#25532 = CIRCLE ( 'NONE', #32923, 1.155000000000000027 ) ;
#25533 =( REPRESENTATION_RELATIONSHIP ('NONE','NONE', #23037, #29156 ) REPRESENTATION_RELATIONSHIP_WITH_TRANSFORMATION ( #909 )SHAPE_REPRESENTATION_RELATIONSHIP( ) );
#25534 = ORIENTED_EDGE ( 'NONE', *, *, #19098, .F. ) ;
#25535 = CARTESIAN_POINT ( 'NONE',  ( 105.3932757502030881, -5.728011724833245388, -4.841576811596270069 ) ) ;
#25536 = ORIENTED_EDGE ( 'NONE', *, *, #20015, .F. ) ;
#25537 = ORIENTED_EDGE ( 'NONE', *, *, #13618, .T. ) ;
#25538 = CARTESIAN_POINT ( 'NONE',  ( 1.040000000000000258, -18.66807150955433769, 28.91175816027496381 ) ) ;
#25539 = EDGE_CURVE ( 'NONE', #18640, #2780, #8130, .T. ) ;
#25540 = DIRECTION ( 'NONE',  ( -1.000000000000000000, 0.000000000000000000, 0.000000000000000000 ) ) ;
#25541 = ADVANCED_FACE ( 'NONE', ( #4146 ), #1325, .F. ) ;
#25542 = VECTOR ( 'NONE', #10887, 1000.000000000000000 ) ;
#25543 = EDGE_CURVE ( 'NONE', #10892, #30842, #793, .T. ) ;
#25544 = CARTESIAN_POINT ( 'NONE',  ( 0.000000000000000000, 0.000000000000000000, 3.931000000000000494 ) ) ;
#25545 = CARTESIAN_POINT ( 'NONE',  ( 0.000000000000000000, 11.30192140231274500, -28.29696565125059493 ) ) ;
#25546 = ORIENTED_EDGE ( 'NONE', *, *, #12675, .F. ) ;
#25547 = VERTEX_POINT ( 'NONE', #3803 ) ;
#25548 = LINE ( 'NONE', #1174, #23624 ) ;
#25549 = CARTESIAN_POINT ( 'NONE',  ( 37.55078559520313775, -4.831299144296470338, 49.43553178847298568 ) ) ;
#25550 = EDGE_CURVE ( 'NONE', #4601, #14930, #22511, .T. ) ;
#25551 = PLANE ( 'NONE',  #3272 ) ;
#25552 = DIRECTION ( 'NONE',  ( 1.000000000000000000, 0.000000000000000000, 0.000000000000000000 ) ) ;
#25553 = DIRECTION ( 'NONE',  ( 0.9289767198167914186, 0.3701381553399144542, -0.000000000000000000 ) ) ;
#25554 = CIRCLE ( 'NONE', #12507, 32.54542015209054995 ) ;
#25555 = CARTESIAN_POINT ( 'NONE',  ( -19.99999999999998934, -112.9999999999999858, 174.9999999999999432 ) ) ;
#25556 = DIRECTION ( 'NONE',  ( 0.000000000000000000, 0.000000000000000000, 1.000000000000000000 ) ) ;
#25557 = ORIENTED_EDGE ( 'NONE', *, *, #6056, .T. ) ;
#25558 = CYLINDRICAL_SURFACE ( 'NONE', #24809, 10.00000000000000888 ) ;
#25559 = DIRECTION ( 'NONE',  ( 1.232595164407830946E-32, 0.000000000000000000, 1.000000000000000000 ) ) ;
#25560 = FACE_OUTER_BOUND ( 'NONE', #21438, .T. ) ;
#25561 = VERTEX_POINT ( 'NONE', #30866 ) ;
#25562 = AXIS2_PLACEMENT_3D ( 'NONE', #14982, #16961, #31169 ) ;
#25563 = FACE_OUTER_BOUND ( 'NONE', #17033, .T. ) ;
#25564 = ORIENTED_EDGE ( 'NONE', *, *, #2127, .T. ) ;
#25565 = CARTESIAN_POINT ( 'NONE',  ( -418.0000000000000000, 105.0000000000000000, 139.9999999999999716 ) ) ;
#25566 = DIRECTION ( 'NONE',  ( 0.000000000000000000, 1.836970198721029441E-16, -1.000000000000000000 ) ) ;
#25567 = ORIENTED_EDGE ( 'NONE', *, *, #1927, .F. ) ;
#25568 = CARTESIAN_POINT ( 'NONE',  ( 11.99999999999999645, -137.0000000000000000, -155.0000000000000284 ) ) ;
#25569 = FACE_OUTER_BOUND ( 'NONE', #8357, .T. ) ;
#25570 = CYLINDRICAL_SURFACE ( 'NONE', #25140, 1.999999999999999556 ) ;
#25571 = ORIENTED_EDGE ( 'NONE', *, *, #13240, .T. ) ;
#25572 = AXIS2_PLACEMENT_3D ( 'NONE', #23317, #12825, #26681 ) ;
#25573 = CARTESIAN_POINT ( 'NONE',  ( 853.3421358984206790, 1009.278375800347362, 1753.598338701303419 ) ) ;
#25574 = EDGE_CURVE ( 'NONE', #33545, #15936, #30290, .T. ) ;
#25575 = DIRECTION ( 'NONE',  ( 0.000000000000000000, 1.000000000000000000, 0.000000000000000000 ) ) ;
#25576 = ORIENTED_EDGE ( 'NONE', *, *, #22232, .T. ) ;
#25577 = PLANE ( 'NONE',  #17882 ) ;
#25578 = B_SPLINE_CURVE_WITH_KNOTS ( 'NONE', 3,
 ( #13315, #28794, #34486, #4741 ),
 .UNSPECIFIED., .F., .F.,
 ( 4, 4 ),
 ( 2.013258991796062060E-07, 0.0006879370499043869483 ),
 .UNSPECIFIED. ) ;
#25579 = ADVANCED_FACE ( 'NONE', ( #3625 ), #977, .T. ) ;
#25580 = DIRECTION ( 'NONE',  ( 0.000000000000000000, 0.000000000000000000, 1.000000000000000000 ) ) ;
#25581 = LINE ( 'NONE', #1039, #16214 ) ;
#25582 = CARTESIAN_POINT ( 'NONE',  ( 2.765921099435497243, 28.29688452313399338, 12.88099432405614309 ) ) ;
#25583 = CONTEXT_DEPENDENT_SHAPE_REPRESENTATION ( #11260, #18316 ) ;
#25584 = VERTEX_POINT ( 'NONE', #30523 ) ;
#25586 = ORIENTED_EDGE ( 'NONE', *, *, #32847, .T. ) ;
#25585 =( REPRESENTATION_RELATIONSHIP ('NONE','NONE', #23037, #28231 ) REPRESENTATION_RELATIONSHIP_WITH_TRANSFORMATION ( #389 )SHAPE_REPRESENTATION_RELATIONSHIP( ) );
#25587 = ORIENTED_EDGE ( 'NONE', *, *, #7985, .T. ) ;
#25588 = EDGE_CURVE ( 'NONE', #13528, #14561, #11477, .T. ) ;
#25589 = SURFACE_SIDE_STYLE ('',( #14762 ) ) ;
#25590 = DIRECTION ( 'NONE',  ( 0.000000000000000000, 7.888609052210118054E-31, 1.000000000000000000 ) ) ;
#25591 = LINE ( 'NONE', #4042, #19048 ) ;
#25592 = CARTESIAN_POINT ( 'NONE',  ( -500.0000000000000000, -137.0000000000000000, 187.0000000000000000 ) ) ;
#25593 = ORIENTED_EDGE ( 'NONE', *, *, #13880, .F. ) ;
#25594 = ADVANCED_FACE ( 'NONE', ( #26394 ), #29175, .T. ) ;
#25595 = DIRECTION ( 'NONE',  ( 0.000000000000000000, 1.000000000000000000, -1.131431318426415506E-52 ) ) ;
#25596 = CARTESIAN_POINT ( 'NONE',  ( 15.99999999999998579, -56.99999999999997868, 154.9999999999999716 ) ) ;
#25597 = ORIENTED_EDGE ( 'NONE', *, *, #27817, .T. ) ;
#25598 = LINE ( 'NONE', #22768, #23238 ) ;
#25599 = ADVANCED_FACE ( 'NONE', ( #34414 ), #7514, .T. ) ;
#25600 = CARTESIAN_POINT ( 'NONE',  ( 0.07094832525803791701, 29.95509811880046058, -10.35390711157451449 ) ) ;
#25601 = AXIS2_PLACEMENT_3D ( 'NONE', #32322, #2601, #8298 ) ;
#25602 = EDGE_CURVE ( 'NONE', #16746, #20411, #14412, .T. ) ;
#25603 = EDGE_LOOP ( 'NONE', ( #33113, #27940, #3521, #11929, #14664, #29113, #30270, #33317, #28647, #26288, #11216, #10841 ) ) ;
#25604 = CARTESIAN_POINT ( 'NONE',  ( 11.99999999999999645, -137.0000000000000000, 174.9999999999999432 ) ) ;
#25605 = DIRECTION ( 'NONE',  ( 0.000000000000000000, -1.000000000000000000, -5.145227585319922065E-49 ) ) ;
#25606 = ORIENTED_EDGE ( 'NONE', *, *, #24115, .F. ) ;
#25607 = CARTESIAN_POINT ( 'NONE',  ( -19.99999999999998934, 144.9999999999999716, -162.9999999999999432 ) ) ;
#25608 = DIRECTION ( 'NONE',  ( 0.000000000000000000, -1.000000000000000000, 0.000000000000000000 ) ) ;
#25609 = DIRECTION ( 'NONE',  ( 2.891205793294675861E-16, 0.000000000000000000, -1.000000000000000000 ) ) ;
#25610 = CIRCLE ( 'NONE', #17103, 15.00000000000000000 ) ;
#25611 = VECTOR ( 'NONE', #1024, 1000.000000000000000 ) ;
#25612 = CARTESIAN_POINT ( 'NONE',  ( -100.4106824525208168, -2.283823867687215348, 12.29365298152801955 ) ) ;
#25613 = UNCERTAINTY_MEASURE_WITH_UNIT (LENGTH_MEASURE( 1.000000000000000082E-05 ), #8063, 'distance_accuracy_value', 'NONE');
#25614 = CARTESIAN_POINT ( 'NONE',  ( 12.00000000000003730, -55.00000000000000711, -154.9999999999999716 ) ) ;
#25615 = LINE ( 'NONE', #18850, #18319 ) ;
#25616 = ORIENTED_EDGE ( 'NONE', *, *, #12403, .F. ) ;
#25617 = EDGE_LOOP ( 'NONE', ( #22162, #22082, #19603, #10401, #27279, #18200 ) ) ;
#25618 = DIRECTION ( 'NONE',  ( -0.9160645104870098754, -0.4010309372432440123, -3.055891501721649571E-14 ) ) ;
#25619 = AXIS2_PLACEMENT_3D ( 'NONE', #30903, #33744, #4003 ) ;
#25620 = ORIENTED_EDGE ( 'NONE', *, *, #30090, .F. ) ;
#25621 = AXIS2_PLACEMENT_3D ( 'NONE', #16110, #34792, #19134 ) ;
#25622 = DIRECTION ( 'NONE',  ( -0.000000000000000000, 1.000000000000000000, 3.017235169886638201E-16 ) ) ;
#25623 = CARTESIAN_POINT ( 'NONE',  ( -10.00000000000000000, 0.000000000000000000, 0.000000000000000000 ) ) ;
#25624 = CONTEXT_DEPENDENT_SHAPE_REPRESENTATION ( #5307, #1568 ) ;
#25625 = ORIENTED_EDGE ( 'NONE', *, *, #5206, .F. ) ;
#25626 = PLANE ( 'NONE',  #3693 ) ;
#25627 = CARTESIAN_POINT ( 'NONE',  ( -109.1548934309756049, -2.987912174852651148, -12.13846169321889512 ) ) ;
#25628 = EDGE_CURVE ( 'NONE', #14577, #26553, #23215, .T. ) ;
#25630 = DIRECTION ( 'NONE',  ( 0.000000000000000000, 0.000000000000000000, 1.000000000000000000 ) ) ;
#25629 = CARTESIAN_POINT ( 'NONE',  ( -365.0000000000000000, -119.0000000000000000, 126.0000000000000000 ) ) ;
#25632 = VERTEX_POINT ( 'NONE', #10202 ) ;
#25631 = VECTOR ( 'NONE', #29673, 1000.000000000000114 ) ;
#25633 = EDGE_LOOP ( 'NONE', ( #29435, #15839, #17958, #8492, #1978, #23959 ) ) ;
#25634 = EDGE_CURVE ( 'NONE', #11675, #24819, #3019, .T. ) ;
#25635 = EDGE_CURVE ( 'NONE', #6283, #3779, #23552, .T. ) ;
#25636 = CARTESIAN_POINT ( 'NONE',  ( 0.000000000000000000, 0.000000000000000000, 0.000000000000000000 ) ) ;
#25637 = VECTOR ( 'NONE', #1625, 1000.000000000000000 ) ;
#25638 = AXIS2_PLACEMENT_3D ( 'NONE', #4195, #7388, #31607 ) ;
#25639 = DIRECTION ( 'NONE',  ( 0.000000000000000000, 5.145227585319922065E-49, 1.000000000000000000 ) ) ;
#25640 = CARTESIAN_POINT ( 'NONE',  ( 7.700000000000000178, 0.000000000000000000, 0.000000000000000000 ) ) ;
#25641 = ORIENTED_EDGE ( 'NONE', *, *, #603, .T. ) ;
#25642 = CARTESIAN_POINT ( 'NONE',  ( 11.99999999999999645, -145.0000000000000000, 187.0000000000000000 ) ) ;
#25643 = CARTESIAN_POINT ( 'NONE',  ( 0.000000000000000000, 3.524919873834583163E-15, 68.31122994652405112 ) ) ;
#25644 = ORIENTED_EDGE ( 'NONE', *, *, #19990, .F. ) ;
#25645 = AXIS2_PLACEMENT_3D ( 'NONE', #23721, #31886, #26038 ) ;
#25646 = CARTESIAN_POINT ( 'NONE',  ( 0.000000000000000000, 3.524919873834583163E-15, 68.31122994652405112 ) ) ;
#25647 = DIRECTION ( 'NONE',  ( 0.000000000000000000, 0.000000000000000000, -1.000000000000000000 ) ) ;
#25648 = EDGE_CURVE ( 'NONE', #21251, #12415, #31391, .T. ) ;
#25649 = VECTOR ( 'NONE', #34394, 1000.000000000000000 ) ;
#25650 = DIRECTION ( 'NONE',  ( -1.000000000000000000, -0.000000000000000000, 0.000000000000000000 ) ) ;
#25652 = LINE ( 'NONE', #17325, #17977 ) ;
#25651 = LINE ( 'NONE', #1452, #1426 ) ;
#25653 = CARTESIAN_POINT ( 'NONE',  ( 1.040000000000001146, 6.183021911002323456, -33.85493898757056286 ) ) ;
#25654 = DIRECTION ( 'NONE',  ( 0.000000000000000000, 0.000000000000000000, 1.000000000000000000 ) ) ;
#25655 = VERTEX_POINT ( 'NONE', #28721 ) ;
#25656 = DIRECTION ( 'NONE',  ( -1.000000000000000000, -0.000000000000000000, -0.000000000000000000 ) ) ;
#25657 = CARTESIAN_POINT ( 'NONE',  ( 0.5344654698446028585, -14.30876692738956457, 2.216488688100102689 ) ) ;
#25658 = PRODUCT_DEFINITION_SHAPE ( 'NONE', 'NONE',  #35147 ) ;
#25659 = EDGE_CURVE ( 'NONE', #15297, #750, #7164, .T. ) ;
#25660 = ADVANCED_FACE ( 'NONE', ( #21054, #15738, #31896 ), #13060, .F. ) ;
#25661 = ORIENTED_EDGE ( 'NONE', *, *, #25853, .F. ) ;
#25662 = EDGE_CURVE ( 'NONE', #16454, #9586, #18945, .T. ) ;
#25663 = CIRCLE ( 'NONE', #4023, 7.999999999999979572 ) ;
#25664 =( LENGTH_UNIT ( ) NAMED_UNIT ( * ) SI_UNIT ( .MILLI., .METRE. ) );
#25665 = AXIS2_PLACEMENT_3D ( 'NONE', #16669, #14170, #30166 ) ;
#25666 = AXIS2_PLACEMENT_3D ( 'NONE', #25116, #6241, #3580 ) ;
#25667 = EDGE_CURVE ( 'NONE', #6969, #6974, #27451, .T. ) ;
#25668 = ORIENTED_EDGE ( 'NONE', *, *, #25156, .T. ) ;
#25669 = LINE ( 'NONE', #17683, #1700 ) ;
#25670 = ORIENTED_EDGE ( 'NONE', *, *, #3225, .F. ) ;
#25671 = ORIENTED_EDGE ( 'NONE', *, *, #20389, .T. ) ;
#25672 = ORIENTED_EDGE ( 'NONE', *, *, #34636, .T. ) ;
#25673 = CARTESIAN_POINT ( 'NONE',  ( 212.5000000000000000, 0.000000000000000000, 0.000000000000000000 ) ) ;
#25674 = ORIENTED_EDGE ( 'NONE', *, *, #23148, .T. ) ;
#25675 = CARTESIAN_POINT ( 'NONE',  ( -15.99999999999998579, 144.9999999999999716, -186.9999999999999716 ) ) ;
#25676 = DIRECTION ( 'NONE',  ( 1.000000000000000000, 0.000000000000000000, -0.000000000000000000 ) ) ;
#25677 = ORIENTED_EDGE ( 'NONE', *, *, #8948, .T. ) ;
#25678 = EDGE_LOOP ( 'NONE', ( #15320, #4066, #16523, #6120 ) ) ;
#25679 = ADVANCED_FACE ( 'NONE', ( #15919 ), #30294, .F. ) ;
#25680 = EDGE_CURVE ( 'NONE', #33855, #9756, #24587, .T. ) ;
#25681 = CARTESIAN_POINT ( 'NONE',  ( -30.91434716440808117, 10.17386417614053684, 68.31122994652405112 ) ) ;
#25682 = CARTESIAN_POINT ( 'NONE',  ( -355.0000000000000000, -114.9999999999999858, 126.0000000000000000 ) ) ;
#25683 = LINE ( 'NONE', #17175, #3379 ) ;
#25684 = LINE ( 'NONE', #6636, #26755 ) ;
#25685 = CARTESIAN_POINT ( 'NONE',  ( -349.0000000000000000, -125.0000000000000284, 113.9999999999999858 ) ) ;
#25686 = VERTEX_POINT ( 'NONE', #13236 ) ;
#25687 = AXIS2_PLACEMENT_3D ( 'NONE', #2113, #32000, #18513 ) ;
#25688 = PLANE ( 'NONE',  #24857 ) ;
#25689 = LINE ( 'NONE', #28193, #25322 ) ;
#25690 = VECTOR ( 'NONE', #15643, 1000.000000000000000 ) ;
#25691 = CARTESIAN_POINT ( 'NONE',  ( -145.0000000000000568, -87.50000000000000000, 65.00000000000000000 ) ) ;
#25692 = VERTEX_POINT ( 'NONE', #11266 ) ;
#25693 = AXIS2_PLACEMENT_3D ( 'NONE', #8626, #5947, #27851 ) ;
#25694 = VECTOR ( 'NONE', #13192, 1000.000000000000000 ) ;
#25695 = CARTESIAN_POINT ( 'NONE',  ( 11.99999999999999645, -28.99999999999999645, -154.9999999999999716 ) ) ;
#25696 = CARTESIAN_POINT ( 'NONE',  ( 1.395000000000002238, 31.89769921722987434, 12.91988538846969803 ) ) ;
#25697 = CARTESIAN_POINT ( 'NONE',  ( -26.18205399241665177, -19.33143609808336549, 68.31122994652405112 ) ) ;
#25698 = CARTESIAN_POINT ( 'NONE',  ( 102.9230630902097374, 5.352195967840122748, -5.254935570228769670 ) ) ;
#25700 = DIRECTION ( 'NONE',  ( 0.000000000000000000, 0.000000000000000000, 1.000000000000000000 ) ) ;
#25699 = LINE ( 'NONE', #29060, #5932 ) ;
#25701 = CARTESIAN_POINT ( 'NONE',  ( -12.00000000000001066, -105.0000000000000142, 155.0000000000000000 ) ) ;
#25702 = ORIENTED_EDGE ( 'NONE', *, *, #23530, .F. ) ;
#25703 = DIRECTION ( 'NONE',  ( -1.000000000000000000, 0.000000000000000000, 0.000000000000000000 ) ) ;
#25705 = CARTESIAN_POINT ( 'NONE',  ( 2.765921099433441555, 11.80989368511502846, -28.76039115933972923 ) ) ;
#25704 = CARTESIAN_POINT ( 'NONE',  ( -500.0000000000000000, -145.0000000000000000, 162.9999999999999716 ) ) ;
#25706 = EDGE_CURVE ( 'NONE', #30641, #14675, #12144, .T. ) ;
#25707 = EDGE_CURVE ( 'NONE', #18645, #30046, #28596, .T. ) ;
#25708 = VERTEX_POINT ( 'NONE', #26918 ) ;
#25709 = PRODUCT_DEFINITION_SHAPE ( 'NONE', 'NONE',  #35106 ) ;
#25710 = CARTESIAN_POINT ( 'NONE',  ( 0.02407890056655651728, 11.80989368511502846, -28.76039115933972923 ) ) ;
#25711 = ADVANCED_FACE ( 'NONE', ( #5541 ), #21589, .F. ) ;
#25712 = VERTEX_POINT ( 'NONE', #16439 ) ;
#25713 = VECTOR ( 'NONE', #17600, 1000.000000000000000 ) ;
#25714 = VECTOR ( 'NONE', #21185, 1000.000000000000114 ) ;
#25715 = VECTOR ( 'NONE', #31397, 1000.000000000000000 ) ;
#25716 = VECTOR ( 'NONE', #21796, 1000.000000000000000 ) ;
#25717 = EDGE_CURVE ( 'NONE', #22621, #32005, #3059, .T. ) ;
#25718 = EDGE_LOOP ( 'NONE', ( #4635, #22267, #26226, #4035 ) ) ;
#25719 = LINE ( 'NONE', #9170, #31009 ) ;
#25720 = ORIENTED_EDGE ( 'NONE', *, *, #1121, .T. ) ;
#25721 = ORIENTED_EDGE ( 'NONE', *, *, #12239, .T. ) ;
#25722 = CYLINDRICAL_SURFACE ( 'NONE', #25803, 8.000000000000000000 ) ;
#25723 = CARTESIAN_POINT ( 'NONE',  ( -12.00000000000001066, -124.9999999999999432, -194.9999999999999432 ) ) ;
#25724 = CARTESIAN_POINT ( 'NONE',  ( -449.9999999999999432, -104.9999999999999858, -162.9999999999999716 ) ) ;
#25725 = CARTESIAN_POINT ( 'NONE',  ( 0.7561992258976059089, 33.57713782924224688, -4.776499238012502424 ) ) ;
#25726 = ORIENTED_EDGE ( 'NONE', *, *, #22881, .T. ) ;
#25727 = VERTEX_POINT ( 'NONE', #24064 ) ;
#25728 = DIRECTION ( 'NONE',  ( 0.000000000000000000, 1.000000000000000000, 0.000000000000000000 ) ) ;
#25729 = LINE ( 'NONE', #22545, #19208 ) ;
#25730 = LINE ( 'NONE', #1356, #19225 ) ;
#25731 = LINE ( 'NONE', #1357, #1081 ) ;
#25732 = DIRECTION ( 'NONE',  ( 0.000000000000000000, 1.000000000000000000, -3.374343856708137958E-53 ) ) ;
#25733 = DIRECTION ( 'NONE',  ( 0.000000000000000000, -0.000000000000000000, 1.000000000000000000 ) ) ;
#25734 = CARTESIAN_POINT ( 'NONE',  ( 0.8386200322165722199, -8.430153398135434628, 12.39854599882999864 ) ) ;
#25735 = VERTEX_POINT ( 'NONE', #2879 ) ;
#25736 = B_SPLINE_CURVE_WITH_KNOTS ( 'NONE', 3,
 ( #27743, #25059, #32730, #11563 ),
 .UNSPECIFIED., .F., .F.,
 ( 4, 4 ),
 ( 2.075676022607250875E-07, 0.0006879433439099810017 ),
 .UNSPECIFIED. ) ;
#25737 = EDGE_CURVE ( 'NONE', #23862, #13509, #10563, .T. ) ;
#25738 = DIRECTION ( 'NONE',  ( -1.000000000000000000, 0.000000000000000000, 0.000000000000000000 ) ) ;
#25739 = DIRECTION ( 'NONE',  ( 0.000000000000000000, 0.000000000000000000, 1.000000000000000000 ) ) ;
#25740 = FACE_OUTER_BOUND ( 'NONE', #26622, .T. ) ;
#25741 = ORIENTED_EDGE ( 'NONE', *, *, #30697, .F. ) ;
#25742 = AXIS2_PLACEMENT_3D ( 'NONE', #31691, #15171, #7302 ) ;
#25743 = VECTOR ( 'NONE', #23421, 1000.000000000000000 ) ;
#25744 = FACE_BOUND ( 'NONE', #17800, .T. ) ;
#25745 = EDGE_LOOP ( 'NONE', ( #29818, #6175, #19778, #3634 ) ) ;
#25746 = LINE ( 'NONE', #26095, #25041 ) ;
#25747 = DIRECTION ( 'NONE',  ( -0.5155538571770220679, -0.8568571761675890519, 0.000000000000000000 ) ) ;
#25748 = EDGE_CURVE ( 'NONE', #6202, #8267, #5190, .T. ) ;
#25749 = EDGE_CURVE ( 'NONE', #27971, #1594, #5858, .T. ) ;
#25750 = ADVANCED_FACE ( 'NONE', ( #13582 ), #2709, .T. ) ;
#25751 = ORIENTED_EDGE ( 'NONE', *, *, #7535, .F. ) ;
#25752 = CARTESIAN_POINT ( 'NONE',  ( 10.17231796313411429, 17.63622956525712482, -87.50000000000000000 ) ) ;
#25753 = LINE ( 'NONE', #23271, #4057 ) ;
#25754 = VERTEX_POINT ( 'NONE', #34948 ) ;
#25755 = COLOUR_RGB ( '',0.7921568627450980005, 0.8196078431372548767, 0.9333333333333333481 ) ;
#25756 = DIRECTION ( 'NONE',  ( -0.1063910735369225230, 0.9943243633099118073, -1.000770725407345128E-14 ) ) ;
#25757 = CARTESIAN_POINT ( 'NONE',  ( -130.6469666100234406, -6.000000000000000000, -62.49999999999999289 ) ) ;
#25758 = VERTEX_POINT ( 'NONE', #29270 ) ;
#25759 = CARTESIAN_POINT ( 'NONE',  ( -19.99999999999998934, 112.9999999999999574, 155.0000000000000000 ) ) ;
#25760 = AXIS2_PLACEMENT_3D ( 'NONE', #20301, #17642, #31155 ) ;
#25761 = DIRECTION ( 'NONE',  ( -0.000000000000000000, 1.000000000000000000, -0.000000000000000000 ) ) ;
#25762 = CIRCLE ( 'NONE', #1877, 30.47050528711511674 ) ;
#25763 = CARTESIAN_POINT ( 'NONE',  ( -442.0000000000000000, -124.9999999999999858, -69.99999999999998579 ) ) ;
#25764 = FACE_OUTER_BOUND ( 'NONE', #4159, .T. ) ;
#25765 = EDGE_LOOP ( 'NONE', ( #23582, #11439, #11592, #26858 ) ) ;
#25766 = VERTEX_POINT ( 'NONE', #44 ) ;
#25767 = AXIS2_PLACEMENT_3D ( 'NONE', #28552, #14515, #28199 ) ;
#25768 = ORIENTED_EDGE ( 'NONE', *, *, #19165, .F. ) ;
#25769 = CARTESIAN_POINT ( 'NONE',  ( 0.07098927069927472855, 26.43944202223353201, 17.47857661787128691 ) ) ;
#25770 = PLANE ( 'NONE',  #14878 ) ;
#25771 = DIRECTION ( 'NONE',  ( 0.000000000000000000, 1.000000000000000000, -6.123233995736766036E-17 ) ) ;
#25772 = CARTESIAN_POINT ( 'NONE',  ( -3.250000000000000000, -5.838643359331793015, -0.7500000000000000000 ) ) ;
#25773 = DIRECTION ( 'NONE',  ( 0.000000000000000000, 0.000000000000000000, 1.000000000000000000 ) ) ;
#25774 = DIRECTION ( 'NONE',  ( 0.000000000000000000, 0.000000000000000000, 1.000000000000000000 ) ) ;
#25775 = EDGE_LOOP ( 'NONE', ( #4565, #8697, #12786 ) ) ;
#25776 = CARTESIAN_POINT ( 'NONE',  ( -42.55956070192387841, -20.15143121711728469, 20.00000000000000000 ) ) ;
#25777 = ORIENTED_EDGE ( 'NONE', *, *, #34359, .F. ) ;
#25778 = DIRECTION ( 'NONE',  ( 0.000000000000000000, 1.000000000000000000, 1.224646799147353207E-16 ) ) ;
#25779 = CIRCLE ( 'NONE', #30329, 3.999999999999976019 ) ;
#25780 = EDGE_CURVE ( 'NONE', #34395, #24520, #4708, .T. ) ;
#25781 = CARTESIAN_POINT ( 'NONE',  ( 3.235562306570555532E-30, 28.08988295778447508, -87.50000000000000000 ) ) ;
#25782 = VERTEX_POINT ( 'NONE', #32782 ) ;
#25783 = DIRECTION ( 'NONE',  ( -0.000000000000000000, -0.000000000000000000, 1.000000000000000000 ) ) ;
#25784 = LINE ( 'NONE', #31140, #32491 ) ;
#25785 = EDGE_CURVE ( 'NONE', #32015, #10470, #8575, .T. ) ;
#25786 = PLANE ( 'NONE',  #10480 ) ;
#25787 = AXIS2_PLACEMENT_3D ( 'NONE', #7668, #32053, #1985 ) ;
#25788 = EDGE_CURVE ( 'NONE', #15103, #25895, #4131, .T. ) ;
#25789 = VECTOR ( 'NONE', #31054, 1000.000000000000000 ) ;
#25790 = VECTOR ( 'NONE', #22778, 1000.000000000000000 ) ;
#25791 = CARTESIAN_POINT ( 'NONE',  ( -100.5687310144427045, -2.576157761670764934, 12.23490486094944174 ) ) ;
#25792 = DIRECTION ( 'NONE',  ( 0.000000000000000000, -3.374343856708137958E-53, 1.000000000000000000 ) ) ;
#25794 = EDGE_CURVE ( 'NONE', #10781, #7013, #19454, .T. ) ;
#25793 = FACE_OUTER_BOUND ( 'NONE', #29638, .T. ) ;
#25795 = ORIENTED_EDGE ( 'NONE', *, *, #24497, .T. ) ;
#25796 = ORIENTED_EDGE ( 'NONE', *, *, #12163, .F. ) ;
#25797 = DIRECTION ( 'NONE',  ( -5.468750338526374368E-14, -4.379194488110368475E-14, 0.9999999999999998890 ) ) ;
#25798 =( REPRESENTATION_RELATIONSHIP ('NONE','NONE', #23037, #15767 ) REPRESENTATION_RELATIONSHIP_WITH_TRANSFORMATION ( #24182 )SHAPE_REPRESENTATION_RELATIONSHIP( ) );
#25799 = B_SPLINE_CURVE_WITH_KNOTS ( 'NONE', 3,
 ( #4645, #24230, #21041, #29233, #20868, #2340 ),
 .UNSPECIFIED., .F., .F.,
 ( 4, 2, 4 ),
 ( 2.185847997383155607E-07, 0.001873416899431755130, 0.003746615214063771931 ),
 .UNSPECIFIED. ) ;
#25800 = EDGE_LOOP ( 'NONE', ( #1859, #34785, #34337, #20690 ) ) ;
#25801 = ADVANCED_FACE ( 'NONE', ( #21414 ), #753, .F. ) ;
#25802 = DIRECTION ( 'NONE',  ( 1.000000000000000000, 0.000000000000000000, 0.000000000000000000 ) ) ;
#25803 = AXIS2_PLACEMENT_3D ( 'NONE', #1347, #9695, #17566 ) ;
#25804 = CARTESIAN_POINT ( 'NONE',  ( -15.99999999999998579, -112.9999999999999858, 174.9999999999999432 ) ) ;
#25805 = ITEM_DEFINED_TRANSFORMATION ( 'NONE', 'NONE', #22337,  #28566 ) ;
#25806 = VERTEX_POINT ( 'NONE', #19809 ) ;
#25807 = DIRECTION ( 'NONE',  ( -1.000000000000000000, -0.000000000000000000, -0.000000000000000000 ) ) ;
#25808 = FACE_OUTER_BOUND ( 'NONE', #23907, .T. ) ;
#25809 = EDGE_LOOP ( 'NONE', ( #17042, #29482, #9961, #19304 ) ) ;
#25811 = FACE_OUTER_BOUND ( 'NONE', #19879, .T. ) ;
#25810 = CARTESIAN_POINT ( 'NONE',  ( 32.05156013847309993, -20.15193397489277771, 68.31122994652405112 ) ) ;
#25812 = VECTOR ( 'NONE', #18369, 1000.000000000000000 ) ;
#25813 = ORIENTED_EDGE ( 'NONE', *, *, #1696, .F. ) ;
#25814 = ORIENTED_EDGE ( 'NONE', *, *, #6672, .T. ) ;
#25815 = CIRCLE ( 'NONE', #17860, 7.999999999999992895 ) ;
#25816 = DIRECTION ( 'NONE',  ( 0.000000000000000000, 0.000000000000000000, 1.000000000000000000 ) ) ;
#25817 = VECTOR ( 'NONE', #27813, 1000.000000000000000 ) ;
#25818 = FACE_OUTER_BOUND ( 'NONE', #28385, .T. ) ;
#25819 = LINE ( 'NONE', #17832, #34734 ) ;
#25820 = ORIENTED_EDGE ( 'NONE', *, *, #8623, .T. ) ;
#25821 = CARTESIAN_POINT ( 'NONE',  ( 2.765921099433442887, -21.56796757982795043, -22.39322359481629476 ) ) ;
#25822 = ORIENTED_EDGE ( 'NONE', *, *, #17443, .F. ) ;
#25823 = DIRECTION ( 'NONE',  ( 0.000000000000000000, 0.000000000000000000, -1.000000000000000000 ) ) ;
#25824 = CARTESIAN_POINT ( 'NONE',  ( 0.000000000000000000, 2.005524111408653720, -29.35189292423236296 ) ) ;
#25825 = EDGE_CURVE ( 'NONE', #3836, #20902, #33490, .T. ) ;
#25826 = CARTESIAN_POINT ( 'NONE',  ( 2.789999999999999147, -13.59935610937951900, -28.90010281771846223 ) ) ;
#25828 = DIRECTION ( 'NONE',  ( -1.000000000000000000, 0.000000000000000000, 0.000000000000000000 ) ) ;
#25827 = CARTESIAN_POINT ( 'NONE',  ( 11.99999999999999645, -145.0000000000000000, 187.0000000000000000 ) ) ;
#25829 = AXIS2_PLACEMENT_3D ( 'NONE', #13601, #13958, #24794 ) ;
#25830 = DIRECTION ( 'NONE',  ( 0.9941379571543595972, 0.1081190184239419622, 1.986114147597513362E-17 ) ) ;
#25831 = DIRECTION ( 'NONE',  ( -1.000000000000000000, 0.000000000000000000, 0.000000000000000000 ) ) ;
#25832 = ORIENTED_EDGE ( 'NONE', *, *, #1754, .F. ) ;
#25833 = DIRECTION ( 'NONE',  ( 0.000000000000000000, 0.000000000000000000, 1.000000000000000000 ) ) ;
#25835 = EDGE_CURVE ( 'NONE', #196, #20661, #6071, .T. ) ;
#25834 = SURFACE_STYLE_USAGE ( .BOTH. , #20335 ) ;
#25836 = CIRCLE ( 'NONE', #32074, 7.999999999999979572 ) ;
#25837 = EDGE_CURVE ( 'NONE', #4182, #3468, #28155, .T. ) ;
#25838 = CIRCLE ( 'NONE', #19802, 7.999999999999979572 ) ;
#25840 = ORIENTED_EDGE ( 'NONE', *, *, #14604, .F. ) ;
#25839 = AXIS2_PLACEMENT_3D ( 'NONE', #1326, #9514, #23553 ) ;
#25841 = EDGE_CURVE ( 'NONE', #9222, #17861, #12741, .T. ) ;
#25842 = EDGE_CURVE ( 'NONE', #34696, #22911, #33321, .T. ) ;
#25843 = VECTOR ( 'NONE', #229, 1000.000000000000000 ) ;
#25844 =( LENGTH_UNIT ( ) NAMED_UNIT ( * ) SI_UNIT ( .MILLI., .METRE. ) );
#25845 = ORIENTED_EDGE ( 'NONE', *, *, #28168, .T. ) ;
#25846 = VECTOR ( 'NONE', #4386, 1000.000000000000000 ) ;
#25847 = EDGE_LOOP ( 'NONE', ( #22133, #2839, #11685, #29044, #22715, #5343 ) ) ;
#25848 = FACE_OUTER_BOUND ( 'NONE', #136, .T. ) ;
#25849 = VERTEX_POINT ( 'NONE', #33136 ) ;
#25850 = ORIENTED_EDGE ( 'NONE', *, *, #23244, .F. ) ;
#25851 = ORIENTED_EDGE ( 'NONE', *, *, #17871, .F. ) ;
#25852 = CARTESIAN_POINT ( 'NONE',  ( -442.0000000000000000, 104.9999999999999858, -159.0000000000000000 ) ) ;
#25853 = EDGE_CURVE ( 'NONE', #23878, #17976, #16693, .T. ) ;
#25854 = AXIS2_PLACEMENT_3D ( 'NONE', #5870, #27600, #3216 ) ;
#25855 = EDGE_LOOP ( 'NONE', ( #8549, #28096 ) ) ;
#25856 = DIRECTION ( 'NONE',  ( -1.000000000000000000, 0.000000000000000000, -0.000000000000000000 ) ) ;
#25857 = CARTESIAN_POINT ( 'NONE',  ( 11.99999999999999645, 124.9999999999999716, 155.0000000000000000 ) ) ;
#25858 = B_SPLINE_CURVE_WITH_KNOTS ( 'NONE', 3,
 ( #11728, #30405, #27552, #22045, #9045, #33061 ),
 .UNSPECIFIED., .F., .F.,
 ( 4, 2, 4 ),
 ( 4.404817020086782935E-07, 0.001874269619297521056, 0.003748098756893033113 ),
 .UNSPECIFIED. ) ;
#25859 = ORIENTED_EDGE ( 'NONE', *, *, #33547, .T. ) ;
#25860 = ORIENTED_EDGE ( 'NONE', *, *, #6464, .T. ) ;
#25861 = CYLINDRICAL_SURFACE ( 'NONE', #21369, 1.649999999999999467 ) ;
#25862 = FACE_OUTER_BOUND ( 'NONE', #18422, .T. ) ;
#25863 = AXIS2_PLACEMENT_3D ( 'NONE', #27740, #3353, #4224 ) ;
#25864 = FACE_BOUND ( 'NONE', #4382, .T. ) ;
#25865 = DIRECTION ( 'NONE',  ( -1.000000000000000000, -0.000000000000000000, -0.000000000000000000 ) ) ;
#25866 = DIRECTION ( 'NONE',  ( 1.000000000000000000, 0.000000000000000000, 0.000000000000000000 ) ) ;
#25867 = ORIENTED_EDGE ( 'NONE', *, *, #23641, .T. ) ;
#25868 = EDGE_CURVE ( 'NONE', #17311, #21561, #8690, .T. ) ;
#25869 = CARTESIAN_POINT ( 'NONE',  ( 0.000000000000000000, 11.69134295108991140, -6.750000000000015987 ) ) ;
#25870 = DIRECTION ( 'NONE',  ( 1.232595164407831220E-32, -3.421138828918010427E-49, 1.000000000000000000 ) ) ;
#25871 = AXIS2_PLACEMENT_3D ( 'NONE', #3674, #3330, #668 ) ;
#25872 = EDGE_CURVE ( 'NONE', #16741, #11336, #22290, .T. ) ;
#25873 = VECTOR ( 'NONE', #19074, 1000.000000000000000 ) ;
#25874 = LINE ( 'NONE', #12362, #285 ) ;
#25875 = ORIENTED_EDGE ( 'NONE', *, *, #277, .F. ) ;
#25876 = MECHANICAL_DESIGN_GEOMETRIC_PRESENTATION_REPRESENTATION (  '', ( #5405 ), #9964 ) ;
#25877 = CARTESIAN_POINT ( 'NONE',  ( -1.155000000000000027, 0.000000000000000000, -0.7500000000000000000 ) ) ;
#25878 = FACE_OUTER_BOUND ( 'NONE', #29900, .T. ) ;
#25879 = DIRECTION ( 'NONE',  ( 0.000000000000000000, 0.000000000000000000, 1.000000000000000000 ) ) ;
#25880 = DIRECTION ( 'NONE',  ( 1.000000000000000000, 0.000000000000000000, 1.300283923313630633E-47 ) ) ;
#25882 = CARTESIAN_POINT ( 'NONE',  ( -20.02113311122509032, -13.65249191622732461, -87.50000000000000000 ) ) ;
#25881 = DIRECTION ( 'NONE',  ( 1.000000000000000000, 0.000000000000000000, 0.000000000000000000 ) ) ;
#25883 = CARTESIAN_POINT ( 'NONE',  ( -499.9999999999999432, 144.9999999999999716, -187.0000000000000000 ) ) ;
#25884 = ORIENTED_EDGE ( 'NONE', *, *, #16293, .T. ) ;
#25885 = CARTESIAN_POINT ( 'NONE',  ( 2.789999999999999147, -20.35927063852789232, -24.61013060777193218 ) ) ;
#25887 = CARTESIAN_POINT ( 'NONE',  ( 8.000000000000000000, 0.000000000000000000, 0.000000000000000000 ) ) ;
#25886 = DIRECTION ( 'NONE',  ( -1.000000000000000000, 0.000000000000000000, 0.000000000000000000 ) ) ;
#25888 = VECTOR ( 'NONE', #15239, 1000.000000000000000 ) ;
#25889 = ORIENTED_EDGE ( 'NONE', *, *, #25131, .T. ) ;
#25890 = ADVANCED_FACE ( 'NONE', ( #8935 ), #16974, .F. ) ;
#25891 = ADVANCED_FACE ( 'NONE', ( #25117, #3237 ), #25301, .T. ) ;
#25892 = AXIS2_PLACEMENT_3D ( 'NONE', #23040, #9510, #1492 ) ;
#25893 = DIRECTION ( 'NONE',  ( 1.000000000000000000, 0.000000000000000000, 0.000000000000000000 ) ) ;
#25894 = VECTOR ( 'NONE', #10980, 1000.000000000000000 ) ;
#25895 = VERTEX_POINT ( 'NONE', #577 ) ;
#25896 = ORIENTED_EDGE ( 'NONE', *, *, #14773, .F. ) ;
#25897 = DIRECTION ( 'NONE',  ( 0.000000000000000000, 2.465190328815661892E-32, 1.000000000000000000 ) ) ;
#25898 = ORIENTED_EDGE ( 'NONE', *, *, #19256, .F. ) ;
#25899 = VERTEX_POINT ( 'NONE', #9108 ) ;
#25900 = DIRECTION ( 'NONE',  ( -1.000000000000000000, -0.000000000000000000, -0.000000000000000000 ) ) ;
#25901 = VECTOR ( 'NONE', #33139, 1000.000000000000000 ) ;
#25902 = CARTESIAN_POINT ( 'NONE',  ( 32.54460952423469422, 0.2297037030477300235, 49.43553178847298568 ) ) ;
#25903 = DIRECTION ( 'NONE',  ( -3.040835319149746528E-31, -1.000000000000000000, 0.000000000000000000 ) ) ;
#25904 = CARTESIAN_POINT ( 'NONE',  ( -410.0000000000000568, -124.9999999999999858, -77.99999999999997158 ) ) ;
#25905 = ORIENTED_EDGE ( 'NONE', *, *, #15122, .T. ) ;
#25906 = EDGE_LOOP ( 'NONE', ( #17707, #31418, #29612, #16466 ) ) ;
#25907 = CARTESIAN_POINT ( 'NONE',  ( 2.765921099433442887, -21.56796757982795043, -22.39322359481629476 ) ) ;
#25908 = DIRECTION ( 'NONE',  ( -1.000000000000000000, 0.000000000000000000, -0.000000000000000000 ) ) ;
#25909 = DIRECTION ( 'NONE',  ( -0.000000000000000000, -0.000000000000000000, -1.000000000000000000 ) ) ;
#25910 = ADVANCED_FACE ( 'NONE', ( #11802 ), #22652, .F. ) ;
#25911 = CARTESIAN_POINT ( 'NONE',  ( -20.00000000000004619, -141.0000000000000000, -187.0000000000000000 ) ) ;
#25912 = CARTESIAN_POINT ( 'NONE',  ( 2.789999999999999147, -31.68806325674609781, 4.003133335385473224 ) ) ;
#25913 = VERTEX_POINT ( 'NONE', #30480 ) ;
#25914 = ADVANCED_FACE ( 'NONE', ( #14818 ), #22471, .F. ) ;
#25915 = EDGE_CURVE ( 'NONE', #8469, #2370, #30339, .T. ) ;
#25916 = VECTOR ( 'NONE', #33518, 1000.000000000000000 ) ;
#25917 = DIRECTION ( 'NONE',  ( -1.000000000000000000, -0.000000000000000000, -0.000000000000000000 ) ) ;
#25918 = DIRECTION ( 'NONE',  ( -0.000000000000000000, -0.000000000000000000, 1.000000000000000000 ) ) ;
#25919 = EDGE_LOOP ( 'NONE', ( #24301, #6172, #3069, #34256 ) ) ;
#25920 = CIRCLE ( 'NONE', #2583, 4.000000000000003553 ) ;
#25921 = CARTESIAN_POINT ( 'NONE',  ( 1.749999999999999778, -10.89151784028265624, -32.64600270996228204 ) ) ;
#25922 = EDGE_CURVE ( 'NONE', #28173, #22010, #22992, .T. ) ;
#25923 = DIRECTION ( 'NONE',  ( 0.000000000000000000, -1.000000000000000000, -2.465190328815662439E-32 ) ) ;
#25924 = PLANE ( 'NONE',  #4677 ) ;
#25925 = ORIENTED_EDGE ( 'NONE', *, *, #23529, .F. ) ;
#25926 = FACE_OUTER_BOUND ( 'NONE', #34431, .T. ) ;
#25927 = EDGE_LOOP ( 'NONE', ( #16022, #25557, #3467, #14658 ) ) ;
#25929 = CARTESIAN_POINT ( 'NONE',  ( -12.00000000000001066, -105.0000000000000142, 155.0000000000000000 ) ) ;
#25928 = PRESENTATION_STYLE_ASSIGNMENT (( #28942 ) ) ;
#25931 = VECTOR ( 'NONE', #4895, 1000.000000000000000 ) ;
#25930 = CARTESIAN_POINT ( 'NONE',  ( 0.000000000000000000, 23.53611639059712601, 19.35207786518996897 ) ) ;
#25932 = ORIENTED_EDGE ( 'NONE', *, *, #32657, .F. ) ;
#25933 = FACE_OUTER_BOUND ( 'NONE', #22347, .T. ) ;
#25934 = FACE_OUTER_BOUND ( 'NONE', #9113, .T. ) ;
#25935 = B_SPLINE_CURVE_WITH_KNOTS ( 'NONE', 3,
 ( #24850, #22370, #22731, #25201 ),
 .UNSPECIFIED., .F., .F.,
 ( 4, 4 ),
 ( 0.005298458409503515980, 0.005985325590332025991 ),
 .UNSPECIFIED. ) ;
#25936 = ORIENTED_EDGE ( 'NONE', *, *, #2767, .F. ) ;
#25937 = AXIS2_PLACEMENT_3D ( 'NONE', #17830, #15150, #25990 ) ;
#25938 = DIRECTION ( 'NONE',  ( -0.1063910735369225230, 0.9943243633099118073, -1.000770725407345128E-14 ) ) ;
#25939 = CARTESIAN_POINT ( 'NONE',  ( 101.4944509101503911, -4.557852096327890123, 11.64155778436300182 ) ) ;
#25940 = EDGE_LOOP ( 'NONE', ( #33557, #29972, #27766, #1384 ) ) ;
#25941 = AXIS2_PLACEMENT_3D ( 'NONE', #8043, #32947, #11258 ) ;
#25942 = LINE ( 'NONE', #34118, #20158 ) ;
#25943 = CARTESIAN_POINT ( 'NONE',  ( -10.84269519964070305, -36.27449394610879096, 68.31122994652405112 ) ) ;
#25944 = DIRECTION ( 'NONE',  ( -0.8568571761675893850, -0.5155538571770214018, 0.000000000000000000 ) ) ;
#25945 = CARTESIAN_POINT ( 'NONE',  ( -23.93921925319781963, 29.33115633223345142, 68.31122994652405112 ) ) ;
#25946 = ORIENTED_EDGE ( 'NONE', *, *, #33747, .T. ) ;
#25947 = ORIENTED_EDGE ( 'NONE', *, *, #19614, .F. ) ;
#25948 = EDGE_LOOP ( 'NONE', ( #3744, #31669, #18138, #20345 ) ) ;
#25949 = FACE_OUTER_BOUND ( 'NONE', #9386, .T. ) ;
#25950 = VECTOR ( 'NONE', #5201, 1000.000000000000000 ) ;
#25951 = FACE_OUTER_BOUND ( 'NONE', #17869, .T. ) ;
#25952 = EDGE_CURVE ( 'NONE', #21269, #12372, #26903, .T. ) ;
#25953 = EDGE_CURVE ( 'NONE', #23746, #26863, #11028, .T. ) ;
#25954 = FACE_OUTER_BOUND ( 'NONE', #23331, .T. ) ;
#25955 = CARTESIAN_POINT ( 'NONE',  ( 20.62763069236413926, -31.74750072459299588, 49.43553178847298568 ) ) ;
#25956 = CARTESIAN_POINT ( 'NONE',  ( -442.0000000000000000, -125.0000000000000000, 187.0000000000000000 ) ) ;
#25957 = DIRECTION ( 'NONE',  ( 1.000000000000000000, 0.000000000000000000, 1.300283923313630633E-47 ) ) ;
#25958 = EDGE_LOOP ( 'NONE', ( #23928, #19481 ) ) ;
#25959 = PRODUCT_DEFINITION_SHAPE ( 'NONE', 'NONE',  #35144 ) ;
#25960 = VECTOR ( 'NONE', #18544, 1000.000000000000000 ) ;
#25961 = CARTESIAN_POINT ( 'NONE',  ( 100.1328585621623120, 3.044914778013036116, 12.12453154756074802 ) ) ;
#25962 = ORIENTED_EDGE ( 'NONE', *, *, #13519, .F. ) ;
#25963 = VECTOR ( 'NONE', #24527, 1000.000000000000000 ) ;
#25964 = DIRECTION ( 'NONE',  ( -1.000000000000000000, 0.000000000000000000, 0.000000000000000000 ) ) ;
#25965 = VERTEX_POINT ( 'NONE', #26168 ) ;
#25966 = DIRECTION ( 'NONE',  ( -1.000000000000000000, 0.000000000000000000, -5.546364386991661285E-52 ) ) ;
#25967 = CARTESIAN_POINT ( 'NONE',  ( 0.7564103347627352258, -17.72288109958190816, -28.91649664306142142 ) ) ;
#25968 = CARTESIAN_POINT ( 'NONE',  ( 0.000000000000000000, -25.77598557799263901, 16.24962337825793313 ) ) ;
#25969 = DIRECTION ( 'NONE',  ( 0.000000000000000000, 0.000000000000000000, -1.000000000000000000 ) ) ;
#25970 = DIRECTION ( 'NONE',  ( 0.000000000000000000, 1.000000000000000000, 0.000000000000000000 ) ) ;
#25971 = ORIENTED_EDGE ( 'NONE', *, *, #15080, .T. ) ;
#25972 = ORIENTED_EDGE ( 'NONE', *, *, #9533, .F. ) ;
#25973 = DIRECTION ( 'NONE',  ( -7.893605728314050488E-14, 1.618803117314786135E-15, 0.9999999999999998890 ) ) ;
#25974 = ORIENTED_EDGE ( 'NONE', *, *, #6250, .T. ) ;
#25975 = AXIS2_PLACEMENT_3D ( 'NONE', #6383, #17095, #3719 ) ;
#25976 = CARTESIAN_POINT ( 'NONE',  ( -21.41424479178918361, -24.50784553716280101, 68.31122994652405112 ) ) ;
#25977 = VECTOR ( 'NONE', #9106, 1000.000000000000000 ) ;
#25978 = LINE ( 'NONE', #1083, #31275 ) ;
#25979 = CONTEXT_DEPENDENT_SHAPE_REPRESENTATION ( #8494, #25709 ) ;
#25980 = VERTEX_POINT ( 'NONE', #7470 ) ;
#25981 = DIRECTION ( 'NONE',  ( 0.000000000000000000, -1.000000000000000000, -1.836970198721029934E-16 ) ) ;
#25982 = DIRECTION ( 'NONE',  ( -1.000000000000000000, 0.000000000000000000, 0.000000000000000000 ) ) ;
#25983 = EDGE_CURVE ( 'NONE', #13790, #20178, #11008, .T. ) ;
#25984 = AXIS2_PLACEMENT_3D ( 'NONE', #22013, #30555, #829 ) ;
#25985 = EDGE_CURVE ( 'NONE', #12821, #24969, #28847, .T. ) ;
#25987 = CARTESIAN_POINT ( 'NONE',  ( -37.69926482250235722, 3.578808500140865156, 68.31122994652405112 ) ) ;
#25986 = LINE ( 'NONE', #26332, #20164 ) ;
#25988 = EDGE_LOOP ( 'NONE', ( #25644, #18017, #35074, #14445 ) ) ;
#25989 = VERTEX_POINT ( 'NONE', #4097 ) ;
#25990 = DIRECTION ( 'NONE',  ( 0.000000000000000000, 0.000000000000000000, -1.000000000000000000 ) ) ;
#25991 = VECTOR ( 'NONE', #27160, 1000.000000000000000 ) ;
#25992 = PRODUCT_DEFINITION ( 'UNKNOWN', '', #33179, #26712 ) ;
#25993 = CARTESIAN_POINT ( 'NONE',  ( -5.021133111224989953, -1.691831803474591833, -67.50000000000000000 ) ) ;
#25994 = CARTESIAN_POINT ( 'NONE',  ( -145.0000000000000568, -97.49999999999998579, 51.88904920397793319 ) ) ;
#25995 = ORIENTED_EDGE ( 'NONE', *, *, #2911, .T. ) ;
#25996 = CARTESIAN_POINT ( 'NONE',  ( -361.0000000000000000, -125.0000000000000284, 181.0000000000000000 ) ) ;
#25997 = VECTOR ( 'NONE', #11747, 1000.000000000000000 ) ;
#25998 = PRODUCT_DEFINITION_SHAPE ( 'NONE', 'NONE',  #35127 ) ;
#25999 = AXIS2_PLACEMENT_3D ( 'NONE', #10053, #23757, #13259 ) ;
#26000 = ORIENTED_EDGE ( 'NONE', *, *, #29805, .F. ) ;
#26001 = LINE ( 'NONE', #3762, #25977 ) ;
#26002 = DIRECTION ( 'NONE',  ( 0.000000000000000000, -1.000000000000000000, 0.000000000000000000 ) ) ;
#26003 = DIRECTION ( 'NONE',  ( 1.000000000000000000, 0.000000000000000000, 0.000000000000000000 ) ) ;
#26005 = CARTESIAN_POINT ( 'NONE',  ( 2.788639899212288054, -26.04763539363528579, -16.24881338200996694 ) ) ;
#26004 = FACE_BOUND ( 'NONE', #34335, .T. ) ;
#26006 = VECTOR ( 'NONE', #4923, 1000.000000000000000 ) ;
#26007 = CIRCLE ( 'NONE', #991, 1.154999999999999805 ) ;
#26008 =( REPRESENTATION_RELATIONSHIP ('NONE','NONE', #23037, #15767 ) REPRESENTATION_RELATIONSHIP_WITH_TRANSFORMATION ( #31318 )SHAPE_REPRESENTATION_RELATIONSHIP( ) );
#26009 = CARTESIAN_POINT ( 'NONE',  ( -12.00000000000001066, -137.0000000000000000, 174.9999999999999432 ) ) ;
#26010 = CARTESIAN_POINT ( 'NONE',  ( -1.035074261544755014E-14, 12.35529564071042330, -5.600000207755282844 ) ) ;
#26011 = CARTESIAN_POINT ( 'NONE',  ( 2.658817013151218312E-15, -10.87635688602997597, 87.50000000000000000 ) ) ;
#26012 = LINE ( 'NONE', #29024, #14329 ) ;
#26013 = AXIS2_PLACEMENT_3D ( 'NONE', #30509, #6104, #3089 ) ;
#26014 = VERTEX_POINT ( 'NONE', #7122 ) ;
#26015 = VERTEX_POINT ( 'NONE', #4448 ) ;
#26016 = EDGE_LOOP ( 'NONE', ( #12633, #32085, #29170, #30018 ) ) ;
#26017 = AXIS2_PLACEMENT_3D ( 'NONE', #19476, #33160, #249 ) ;
#26018 = DIRECTION ( 'NONE',  ( 1.000000000000000000, 0.000000000000000000, -0.000000000000000000 ) ) ;
#26019 = VERTEX_POINT ( 'NONE', #23854 ) ;
#26020 = ORIENTED_EDGE ( 'NONE', *, *, #15107, .T. ) ;
#26021 = VERTEX_POINT ( 'NONE', #1620 ) ;
#26022 = FACE_OUTER_BOUND ( 'NONE', #23225, .T. ) ;
#26023 = ADVANCED_FACE ( 'NONE', ( #28505 ), #28676, .F. ) ;
#26024 = ITEM_DEFINED_TRANSFORMATION ( 'NONE', 'NONE', #21241,  #28566 ) ;
#26025 = VECTOR ( 'NONE', #32361, 1000.000000000000000 ) ;
#26026 = VECTOR ( 'NONE', #19003, 1000.000000000000000 ) ;
#26027 = ORIENTED_EDGE ( 'NONE', *, *, #34717, .F. ) ;
#26028 = DIRECTION ( 'NONE',  ( 0.000000000000000000, 0.000000000000000000, -1.000000000000000000 ) ) ;
#26029 = CARTESIAN_POINT ( 'NONE',  ( -35.00000000000000000, 45.00000000000000711, -36.68877005347592757 ) ) ;
#26030 = ORIENTED_EDGE ( 'NONE', *, *, #13947, .F. ) ;
#26031 = ORIENTED_EDGE ( 'NONE', *, *, #5916, .F. ) ;
#26032 = FACE_OUTER_BOUND ( 'NONE', #5006, .T. ) ;
#26033 = CARTESIAN_POINT ( 'NONE',  ( -5.210000000000000853, 0.000000000000000000, 0.000000000000000000 ) ) ;
#26034 = EDGE_CURVE ( 'NONE', #1780, #31407, #4277, .T. ) ;
#26035 = EDGE_CURVE ( 'NONE', #7776, #15307, #34189, .T. ) ;
#26036 = DIRECTION ( 'NONE',  ( -0.000000000000000000, -1.000000000000000000, -0.000000000000000000 ) ) ;
#26037 = LINE ( 'NONE', #14852, #3449 ) ;
#26038 = DIRECTION ( 'NONE',  ( 0.9289767198167915296, 0.3701381553399144542, 0.000000000000000000 ) ) ;
#26039 = ORIENTED_EDGE ( 'NONE', *, *, #10922, .T. ) ;
#26040 = TOROIDAL_SURFACE ( 'NONE', #6109, 30.47050528711512030, 8.000000000000000000 ) ;
#26041 = PLANE ( 'NONE',  #8373 ) ;
#26042 = LINE ( 'NONE', #23033, #27029 ) ;
#26043 = EDGE_CURVE ( 'NONE', #1246, #17344, #6779, .T. ) ;
#26044 = DIRECTION ( 'NONE',  ( 1.000000000000000000, 0.000000000000000000, 0.000000000000000000 ) ) ;
#26045 = ORIENTED_EDGE ( 'NONE', *, *, #17948, .T. ) ;
#26046 = DIRECTION ( 'NONE',  ( 0.000000000000000000, -6.123233995736766036E-17, -1.000000000000000000 ) ) ;
#26047 = DIRECTION ( 'NONE',  ( 1.000000000000000000, 0.000000000000000000, -1.848892746611746966E-32 ) ) ;
#26048 = SURFACE_STYLE_FILL_AREA ( #4319 ) ;
#26049 = EDGE_CURVE ( 'NONE', #35075, #30822, #18418, .T. ) ;
#26050 = CARTESIAN_POINT ( 'NONE',  ( 5.021133111224162171, -25.61315202898006049, -67.50000000000000000 ) ) ;
#26052 = CARTESIAN_POINT ( 'NONE',  ( -102.7041492557062128, 4.573766672917669140, -5.944761500833685375 ) ) ;
#26051 = CARTESIAN_POINT ( 'NONE',  ( 12.00000000000001066, -32.99999999999997158, 154.9999999999999716 ) ) ;
#26053 = CIRCLE ( 'NONE', #1062, 1.999999999999999556 ) ;
#26054 = CARTESIAN_POINT ( 'NONE',  ( 28.11866956577617316, 16.38733641342590985, 68.31122994652405112 ) ) ;
#26055 = VERTEX_POINT ( 'NONE', #6947 ) ;
#26056 = CARTESIAN_POINT ( 'NONE',  ( 110.7380848894536456, 0.3793982372081800558, -12.50000000000000178 ) ) ;
#26058 = LINE ( 'NONE', #29070, #2091 ) ;
#26057 = DIRECTION ( 'NONE',  ( 0.000000000000000000, 0.000000000000000000, 1.000000000000000000 ) ) ;
#26059 = AXIS2_PLACEMENT_3D ( 'NONE', #29359, #13511, #8338 ) ;
#26060 = ORIENTED_EDGE ( 'NONE', *, *, #25356, .T. ) ;
#26061 = AXIS2_PLACEMENT_3D ( 'NONE', #15493, #15143, #7632 ) ;
#26062 = CYLINDRICAL_SURFACE ( 'NONE', #25070, 22.50000000000000355 ) ;
#26063 = B_SPLINE_CURVE_WITH_KNOTS ( 'NONE', 3,
 ( #34889, #10502, #16025, #11695, #5137, #21695 ),
 .UNSPECIFIED., .F., .F.,
 ( 4, 2, 4 ),
 ( 1.978042196652697246E-07, 0.001873396096185926674, 0.003746594388152188135 ),
 .UNSPECIFIED. ) ;
#26064 = ORIENTED_EDGE ( 'NONE', *, *, #29248, .T. ) ;
#26065 = AXIS2_PLACEMENT_3D ( 'NONE', #14769, #28283, #21924 ) ;
#26066 = EDGE_LOOP ( 'NONE', ( #21544, #30387, #22963, #3275 ) ) ;
#26067 = DIRECTION ( 'NONE',  ( 0.000000000000000000, 0.000000000000000000, 1.000000000000000000 ) ) ;
#26068 = ORIENTED_EDGE ( 'NONE', *, *, #22257, .T. ) ;
#26069 = ORIENTED_EDGE ( 'NONE', *, *, #1253, .T. ) ;
#26070 = FACE_OUTER_BOUND ( 'NONE', #20949, .T. ) ;
#26071 = AXIS2_PLACEMENT_3D ( 'NONE', #32370, #22365, #3486 ) ;
#26072 = CARTESIAN_POINT ( 'NONE',  ( 23.31255882915078814, -22.70966696615089830, 68.31122994652405112 ) ) ;
#26073 = LINE ( 'NONE', #23241, #4587 ) ;
#26074 = ORIENTED_EDGE ( 'NONE', *, *, #20590, .F. ) ;
#26075 = ORIENTED_EDGE ( 'NONE', *, *, #34321, .T. ) ;
#26076 = CARTESIAN_POINT ( 'NONE',  ( -12.00000000000001066, 108.9999999999999858, 155.0000000000000000 ) ) ;
#26077 = CARTESIAN_POINT ( 'NONE',  ( 2.789999999999999147, 20.99477179376858871, -22.93149026599722617 ) ) ;
#26078 = PLANE ( 'NONE',  #33381 ) ;
#26079 = EDGE_CURVE ( 'NONE', #31010, #19356, #9983, .T. ) ;
#26080 = DIRECTION ( 'NONE',  ( -3.469446951953832974E-18, -1.000000000000000000, -7.888609052210116302E-31 ) ) ;
#26081 = DIRECTION ( 'NONE',  ( 0.000000000000000000, 0.000000000000000000, -1.000000000000000000 ) ) ;
#26082 = EDGE_LOOP ( 'NONE', ( #31096, #21758, #25037, #15252 ) ) ;
#26083 = VECTOR ( 'NONE', #11907, 1000.000000000000000 ) ;
#26084 = DIRECTION ( 'NONE',  ( -0.000000000000000000, -0.000000000000000000, -1.000000000000000000 ) ) ;
#26085 = EDGE_CURVE ( 'NONE', #16011, #29267, #10452, .T. ) ;
#26086 = EDGE_CURVE ( 'NONE', #24757, #17376, #3045, .T. ) ;
#26087 = CARTESIAN_POINT ( 'NONE',  ( -15.99999999999998579, -56.99999999999997868, -154.9999999999999716 ) ) ;
#26088 = ORIENTED_EDGE ( 'NONE', *, *, #418, .T. ) ;
#26089 = CARTESIAN_POINT ( 'NONE',  ( 1.040000000000001590, 34.10861917999616111, 4.581348211832199091 ) ) ;
#26090 = DIRECTION ( 'NONE',  ( 0.000000000000000000, 0.000000000000000000, 1.000000000000000000 ) ) ;
#26091 = LINE ( 'NONE', #15424, #25743 ) ;
#26092 = ORIENTED_EDGE ( 'NONE', *, *, #31883, .T. ) ;
#26093 = DIRECTION ( 'NONE',  ( 3.697785493223492838E-32, 1.934419779023891545E-16, -1.000000000000000000 ) ) ;
#26094 = VERTEX_POINT ( 'NONE', #10333 ) ;
#26096 = CARTESIAN_POINT ( 'NONE',  ( 1.039999999999999369, -18.21166265554768060, -29.20140402659759360 ) ) ;
#26095 = CARTESIAN_POINT ( 'NONE',  ( -34.04247984038124031, 16.56841925338182619, -36.68877005347593467 ) ) ;
#26097 = CARTESIAN_POINT ( 'NONE',  ( 0.02407890056655868569, 24.20451283648829133, 19.51346322004938827 ) ) ;
#26098 = EDGE_CURVE ( 'NONE', #30076, #7133, #21244, .T. ) ;
#26099 = AXIS2_PLACEMENT_3D ( 'NONE', #33166, #13788, #24438 ) ;
#26100 = ORIENTED_EDGE ( 'NONE', *, *, #34140, .F. ) ;
#26101 = DIRECTION ( 'NONE',  ( 0.000000000000000000, 0.000000000000000000, 1.000000000000000000 ) ) ;
#26102 = DIRECTION ( 'NONE',  ( 0.000000000000000000, 1.836970198721029441E-16, -1.000000000000000000 ) ) ;
#26103 = EDGE_CURVE ( 'NONE', #20721, #19820, #29017, .T. ) ;
#26104 = VERTEX_POINT ( 'NONE', #20494 ) ;
#26105 = AXIS2_PLACEMENT_3D ( 'NONE', #29226, #17733, #15715 ) ;
#26106 = ADVANCED_FACE ( 'NONE', ( #29205 ), #14991, .F. ) ;
#26107 = DIRECTION ( 'NONE',  ( 0.1063910735369155841, -0.9943243633099125844, -3.335902418025060287E-15 ) ) ;
#26108 = VERTEX_POINT ( 'NONE', #18362 ) ;
#26109 = CARTESIAN_POINT ( 'NONE',  ( 104.0474366975612526, -5.661646449284259752, 11.14439484353663090 ) ) ;
#26110 = VERTEX_POINT ( 'NONE', #34015 ) ;
#26111 = CARTESIAN_POINT ( 'NONE',  ( -365.0000000000000000, -135.0000000000000000, 113.9999999999999858 ) ) ;
#26112 = ADVANCED_FACE ( 'NONE', ( #9636 ), #17842, .F. ) ;
#26113 = VECTOR ( 'NONE', #787, 1000.000000000000000 ) ;
#26114 = DIRECTION ( 'NONE',  ( 0.000000000000000000, 0.000000000000000000, -1.000000000000000000 ) ) ;
#26115 = CARTESIAN_POINT ( 'NONE',  ( 19.99999999999996092, -134.9999999999999716, 187.0000000000000000 ) ) ;
#26116 = DIRECTION ( 'NONE',  ( 0.000000000000000000, 1.000000000000000000, -3.374343856708137958E-53 ) ) ;
#26117 = VERTEX_POINT ( 'NONE', #8183 ) ;
#26118 = VERTEX_POINT ( 'NONE', #5 ) ;
#26119 = ORIENTED_EDGE ( 'NONE', *, *, #10434, .T. ) ;
#26120 = CARTESIAN_POINT ( 'NONE',  ( -355.0000000000000000, -119.0000000000000000, 109.9999999999999858 ) ) ;
#26121 = CARTESIAN_POINT ( 'NONE',  ( -5.021133111224782120, 16.12922284503173742, -67.50000000000000000 ) ) ;
#26122 = CARTESIAN_POINT ( 'NONE',  ( 0.000000000000000000, 30.40449935640659973, -2.004522720844279959 ) ) ;
#26123 = CIRCLE ( 'NONE', #28971, 4.000000000000003553 ) ;
#26124 = CARTESIAN_POINT ( 'NONE',  ( -11.99999999999998224, -134.9999999999999716, 155.0000000000000000 ) ) ;
#26125 = ADVANCED_FACE ( 'NONE', ( #32037 ), #13370, .T. ) ;
#26126 = CARTESIAN_POINT ( 'NONE',  ( 0.000000000000000000, 23.28319895603611300, -21.86437915510192909 ) ) ;
#26127 = DIRECTION ( 'NONE',  ( 0.000000000000000000, -1.310824597558155437E-49, -1.000000000000000000 ) ) ;
#26128 = ORIENTED_EDGE ( 'NONE', *, *, #27551, .F. ) ;
#26129 = CARTESIAN_POINT ( 'NONE',  ( 2.765921099433444663, 29.44518845714764765, 9.980709654879525772 ) ) ;
#26130 = CARTESIAN_POINT ( 'NONE',  ( -442.0000000000000000, -125.0000000000000000, 100.0000000000000000 ) ) ;
#26131 = VERTEX_POINT ( 'NONE', #35081 ) ;
#26132 = LINE ( 'NONE', #17461, #18922 ) ;
#26133 = EDGE_LOOP ( 'NONE', ( #23355, #14130, #33574, #22130 ) ) ;
#26134 = PLANE ( 'NONE',  #10343 ) ;
#26135 = CARTESIAN_POINT ( 'NONE',  ( 2.789999999999999147, 3.909681563762101852, -30.21863799912378923 ) ) ;
#26136 = AXIS2_PLACEMENT_3D ( 'NONE', #16500, #2247, #30009 ) ;
#26137 = FACE_OUTER_BOUND ( 'NONE', #13972, .T. ) ;
#26138 = DIRECTION ( 'NONE',  ( 1.000000000000000000, 0.000000000000000000, 0.000000000000000000 ) ) ;
#26139 = CARTESIAN_POINT ( 'NONE',  ( -500.0000000000000000, -113.0000000000000000, 187.0000000000000000 ) ) ;
#26140 = EDGE_LOOP ( 'NONE', ( #6159, #13426, #22951, #14619 ) ) ;
#26141 = EDGE_CURVE ( 'NONE', #21605, #14930, #10701, .T. ) ;
#26142 = EDGE_CURVE ( 'NONE', #8847, #19179, #10519, .T. ) ;
#26143 = VERTEX_POINT ( 'NONE', #21376 ) ;
#26144 = DIRECTION ( 'NONE',  ( -0.1063910735369017202, 0.9943243633099136947, -1.000770725407181676E-14 ) ) ;
#26145 = ORIENTED_EDGE ( 'NONE', *, *, #1127, .F. ) ;
#26146 = LINE ( 'NONE', #23479, #9577 ) ;
#26147 = DIRECTION ( 'NONE',  ( 0.000000000000000000, 1.000000000000000000, 1.836970198721029688E-16 ) ) ;
#26148 = PLANE ( 'NONE',  #7372 ) ;
#26150 = EDGE_CURVE ( 'NONE', #30004, #28861, #21550, .T. ) ;
#26149 = ORIENTED_EDGE ( 'NONE', *, *, #19572, .F. ) ;
#26151 = DIRECTION ( 'NONE',  ( 1.000000000000000000, 0.000000000000000000, 0.000000000000000000 ) ) ;
#26152 = VECTOR ( 'NONE', #5128, 1000.000000000000000 ) ;
#26154 = CARTESIAN_POINT ( 'NONE',  ( -20.00000000000004619, 112.9999999999999574, 194.9999999999999716 ) ) ;
#26153 = DIRECTION ( 'NONE',  ( 0.000000000000000000, 1.836970198721029441E-16, -1.000000000000000000 ) ) ;
#26155 = VERTEX_POINT ( 'NONE', #13539 ) ;
#26156 = EDGE_LOOP ( 'NONE', ( #8392, #8160, #24596, #6015 ) ) ;
#26157 = DIRECTION ( 'NONE',  ( 0.000000000000000000, 5.145227585319922065E-49, 1.000000000000000000 ) ) ;
#26158 = VERTEX_POINT ( 'NONE', #10866 ) ;
#26159 = DIRECTION ( 'NONE',  ( 0.000000000000000000, 0.000000000000000000, -1.000000000000000000 ) ) ;
#26160 = DIRECTION ( 'NONE',  ( -1.000000000000000000, 6.792721752314501023E-48, -3.697785493223492838E-32 ) ) ;
#26161 = VERTEX_POINT ( 'NONE', #3015 ) ;
#26162 = CARTESIAN_POINT ( 'NONE',  ( -12.00000000000001066, -56.99999999999997868, -175.0000000000000000 ) ) ;
#26163 = VECTOR ( 'NONE', #28796, 1000.000000000000000 ) ;
#26164 = ORIENTED_EDGE ( 'NONE', *, *, #14527, .F. ) ;
#26165 = ADVANCED_FACE ( 'NONE', ( #18887 ), #18718, .T. ) ;
#26166 = DIRECTION ( 'NONE',  ( 0.000000000000000000, 0.000000000000000000, -1.000000000000000000 ) ) ;
#26167 = DIRECTION ( 'NONE',  ( -0.000000000000000000, -1.836970198721029688E-16, 1.000000000000000000 ) ) ;
#26168 = CARTESIAN_POINT ( 'NONE',  ( -12.00000000000001066, -145.0000000000000000, 194.9999999999999716 ) ) ;
#26170 = FACE_OUTER_BOUND ( 'NONE', #8300, .T. ) ;
#26169 = DIRECTION ( 'NONE',  ( 1.000000000000000000, 0.000000000000000000, -0.000000000000000000 ) ) ;
#26171 = CARTESIAN_POINT ( 'NONE',  ( -5.527271473480783293, -1.747512292859696226, -0.7500000000000000000 ) ) ;
#26172 = CARTESIAN_POINT ( 'NONE',  ( 1.991296462759137853, -32.48444414290483451, 68.31122994652405112 ) ) ;
#26173 = DIRECTION ( 'NONE',  ( 0.000000000000000000, 0.000000000000000000, 1.000000000000000000 ) ) ;
#26174 = VECTOR ( 'NONE', #28369, 1000.000000000000000 ) ;
#26175 = DIRECTION ( 'NONE',  ( 0.000000000000000000, -1.000000000000000000, 0.000000000000000000 ) ) ;
#26176 = ADVANCED_FACE ( 'NONE', ( #13892 ), #19241, .T. ) ;
#26177 = AXIS2_PLACEMENT_3D ( 'NONE', #26814, #2423, #13470 ) ;
#26178 = EDGE_CURVE ( 'NONE', #15752, #21251, #24544, .T. ) ;
#26179 = EDGE_CURVE ( 'NONE', #30076, #32798, #29728, .T. ) ;
#26180 = EDGE_LOOP ( 'NONE', ( #24001, #34305, #17770, #18781, #8055, #1173, #2221, #78, #31528, #25400, #15783, #4686, #13550, #20579, #22533, #8299, #33078, #8845, #33752, #207, #4019, #34568, #8324, #25493, #20363, #8610, #4644, #33159, #7321, #7971, #23535, #23711, #20219, #27768, #5642, #22418, #15, #11319, #4862, #3265, #18378, #597, #25564, #24790, #28695, #31384, #19249, #17695, #21977, #8138, #18948, #1854, #31801, #6234, #20977, #8770, #26581 ) ) ;
#26181 = EDGE_LOOP ( 'NONE', ( #31234, #13339, #2375, #27844, #12905 ) ) ;
#26182 = VERTEX_POINT ( 'NONE', #2671 ) ;
#26183 = DIRECTION ( 'NONE',  ( 0.000000000000000000, 0.000000000000000000, 1.000000000000000000 ) ) ;
#26184 = DIRECTION ( 'NONE',  ( 0.9307115204415121745, -0.3657541055373795258, 1.801445575657210240E-14 ) ) ;
#26185 = VECTOR ( 'NONE', #2237, 1000.000000000000000 ) ;
#26186 = ORIENTED_EDGE ( 'NONE', *, *, #31503, .T. ) ;
#26187 = COLOUR_RGB ( '',0.7921568627450980005, 0.8196078431372548767, 0.9333333333333333481 ) ;
#26188 = ORIENTED_EDGE ( 'NONE', *, *, #10253, .T. ) ;
#26189 = ORIENTED_EDGE ( 'NONE', *, *, #26740, .F. ) ;
#26190 = PLANE ( 'NONE',  #1993 ) ;
#26191 = ITEM_DEFINED_TRANSFORMATION ( 'NONE', 'NONE', #14451,  #28566 ) ;
#26192 = ORIENTED_EDGE ( 'NONE', *, *, #25794, .F. ) ;
#26193 = FACE_OUTER_BOUND ( 'NONE', #33475, .T. ) ;
#26194 = LINE ( 'NONE', #26029, #25649 ) ;
#26195 = ORIENTED_EDGE ( 'NONE', *, *, #34982, .T. ) ;
#26196 = ORIENTED_EDGE ( 'NONE', *, *, #17590, .F. ) ;
#26197 = CYLINDRICAL_SURFACE ( 'NONE', #20803, 1.999999999999999112 ) ;
#26199 = CARTESIAN_POINT ( 'NONE',  ( -442.0000000000000000, -137.0000000000000000, -155.0000000000000000 ) ) ;
#26198 = CIRCLE ( 'NONE', #19972, 2.525000000000000799 ) ;
#26200 = B_SPLINE_CURVE_WITH_KNOTS ( 'NONE', 3,
 ( #15344, #32041, #1626, #15518 ),
 .UNSPECIFIED., .F., .F.,
 ( 4, 4 ),
 ( 0.005679541198217082261, 0.005985272568144436693 ),
 .UNSPECIFIED. ) ;
#26201 = LINE ( 'NONE', #1821, #22137 ) ;
#26202 = DIRECTION ( 'NONE',  ( -1.000000000000000000, 0.000000000000000000, 0.000000000000000000 ) ) ;
#26203 = CARTESIAN_POINT ( 'NONE',  ( 11.99999999999999645, 112.9999999999999574, 155.0000000000000000 ) ) ;
#26204 = ORIENTED_EDGE ( 'NONE', *, *, #18517, .F. ) ;
#26205 = CIRCLE ( 'NONE', #17703, 34.41491905851385269 ) ;
#26206 = DIRECTION ( 'NONE',  ( 0.000000000000000000, 0.000000000000000000, 1.000000000000000000 ) ) ;
#26207 = LINE ( 'NONE', #23886, #21373 ) ;
#26208 = DIRECTION ( 'NONE',  ( 0.000000000000000000, 0.000000000000000000, 1.000000000000000000 ) ) ;
#26209 = VERTEX_POINT ( 'NONE', #29383 ) ;
#26210 = FACE_OUTER_BOUND ( 'NONE', #7491, .T. ) ;
#26211 = CARTESIAN_POINT ( 'NONE',  ( 0.02407890056655695096, -26.45933846664205902, 16.32596387352436551 ) ) ;
#26212 = CARTESIAN_POINT ( 'NONE',  ( 110.4116262905429267, 1.917593826231215770, -7.253178031220425481 ) ) ;
#26214 = CARTESIAN_POINT ( 'NONE',  ( -430.0000000000000000, 132.9999999999999716, 113.9999999999999858 ) ) ;
#26213 = CARTESIAN_POINT ( 'NONE',  ( -18.07349068442141515, -27.06572199953720315, -36.68877005347593467 ) ) ;
#26215 = AXIS2_PLACEMENT_3D ( 'NONE', #6939, #4089, #28144 ) ;
#26216 = AXIS2_PLACEMENT_3D ( 'NONE', #15658, #28812, #29348 ) ;
#26217 = EDGE_CURVE ( 'NONE', #12516, #1340, #19069, .T. ) ;
#26218 = CARTESIAN_POINT ( 'NONE',  ( -30.76765767668601725, -10.60922306139169891, -36.68877005347593467 ) ) ;
#26220 = EDGE_LOOP ( 'NONE', ( #12338, #14666, #34572, #17167, #7531, #15526, #30679, #2862 ) ) ;
#26219 = AXIS2_PLACEMENT_3D ( 'NONE', #5341, #11052, #29740 ) ;
#26222 = CIRCLE ( 'NONE', #25666, 7.999999999999979572 ) ;
#26221 = CARTESIAN_POINT ( 'NONE',  ( 105.7593996005910100, 5.690832488206153172, -11.12946004024182756 ) ) ;
#26223 = CARTESIAN_POINT ( 'NONE',  ( 0.8386200322165693333, 8.430153398135427523, -12.39854599882999509 ) ) ;
#26224 = EDGE_CURVE ( 'NONE', #16525, #19620, #5085, .T. ) ;
#26225 = EDGE_CURVE ( 'NONE', #11787, #28629, #368, .T. ) ;
#26226 = ORIENTED_EDGE ( 'NONE', *, *, #14075, .T. ) ;
#26227 = DIRECTION ( 'NONE',  ( 0.000000000000000000, -0.08715574274765885976, -0.9961946980917454342 ) ) ;
#26228 = ADVANCED_FACE ( 'NONE', ( #16044 ), #16402, .T. ) ;
#26229 = ORIENTED_EDGE ( 'NONE', *, *, #21764, .T. ) ;
#26230 = AXIS2_PLACEMENT_3D ( 'NONE', #9658, #6977, #1996 ) ;
#26231 = ORIENTED_EDGE ( 'NONE', *, *, #22437, .T. ) ;
#26232 = CARTESIAN_POINT ( 'NONE',  ( -37.85301660235036536, 0.7430237821112765095, -36.68877005347593467 ) ) ;
#26233 = ORIENTED_EDGE ( 'NONE', *, *, #7221, .T. ) ;
#26234 = ORIENTED_EDGE ( 'NONE', *, *, #28802, .F. ) ;
#26235 = FACE_OUTER_BOUND ( 'NONE', #12170, .T. ) ;
#26236 = PRODUCT_DEFINITION_SHAPE ( 'NONE', 'NONE',  #35177 ) ;
#26237 = EDGE_CURVE ( 'NONE', #3245, #19221, #21173, .T. ) ;
#26238 = CIRCLE ( 'NONE', #13201, 7.999999999999979572 ) ;
#26239 = DIRECTION ( 'NONE',  ( 0.000000000000000000, 0.000000000000000000, 1.000000000000000000 ) ) ;
#26240 = AXIS2_PLACEMENT_3D ( 'NONE', #23596, #31602, #20924 ) ;
#26241 = FACE_OUTER_BOUND ( 'NONE', #23760, .T. ) ;
#26242 = ORIENTED_EDGE ( 'NONE', *, *, #34966, .T. ) ;
#26243 = ORIENTED_EDGE ( 'NONE', *, *, #31141, .T. ) ;
#26244 = VECTOR ( 'NONE', #12585, 1000.000000000000000 ) ;
#26245 = CARTESIAN_POINT ( 'NONE',  ( 3.235562306570555532E-30, 8.235406450278430768, -87.50000000000000000 ) ) ;
#26246 = FACE_OUTER_BOUND ( 'NONE', #31259, .T. ) ;
#26247 = AXIS2_PLACEMENT_3D ( 'NONE', #24214, #32396, #16232 ) ;
#26248 = VECTOR ( 'NONE', #25966, 1000.000000000000000 ) ;
#26249 = FACE_OUTER_BOUND ( 'NONE', #15990, .T. ) ;
#26250 = FACE_OUTER_BOUND ( 'NONE', #9048, .T. ) ;
#26251 = DIRECTION ( 'NONE',  ( -1.000000000000000000, -0.000000000000000000, -0.000000000000000000 ) ) ;
#26252 = ORIENTED_EDGE ( 'NONE', *, *, #4286, .F. ) ;
#26253 = ORIENTED_EDGE ( 'NONE', *, *, #31961, .F. ) ;
#26254 = CARTESIAN_POINT ( 'NONE',  ( -19.99999999999998934, -124.9999999999999432, -154.9999999999999716 ) ) ;
#26255 = CARTESIAN_POINT ( 'NONE',  ( 0.02849990174190264458, -11.02838903529590198, 7.898269865231986486 ) ) ;
#26256 = ORIENTED_EDGE ( 'NONE', *, *, #8248, .T. ) ;
#26257 = DIRECTION ( 'NONE',  ( 0.000000000000000000, 1.000000000000000000, -6.123233995736766036E-17 ) ) ;
#26258 = DIRECTION ( 'NONE',  ( -1.000000000000000000, -0.000000000000000000, 0.000000000000000000 ) ) ;
#26259 = DIRECTION ( 'NONE',  ( -1.292961597001347186E-16, -0.000000000000000000, 1.000000000000000000 ) ) ;
#26260 = EDGE_LOOP ( 'NONE', ( #1506, #34268, #11700, #9172 ) ) ;
#26261 =( REPRESENTATION_RELATIONSHIP ('NONE','NONE', #23037, #8672 ) REPRESENTATION_RELATIONSHIP_WITH_TRANSFORMATION ( #20478 )SHAPE_REPRESENTATION_RELATIONSHIP( ) );
#26262 = DIRECTION ( 'NONE',  ( 0.000000000000000000, 0.000000000000000000, -1.000000000000000000 ) ) ;
#26263 = ORIENTED_EDGE ( 'NONE', *, *, #9845, .T. ) ;
#26265 = DIRECTION ( 'NONE',  ( -0.9476531711828023452, 0.3193015301359802827, 0.000000000000000000 ) ) ;
#26264 = FILL_AREA_STYLE ('',( #6864 ) ) ;
#26266 = CARTESIAN_POINT ( 'NONE',  ( 11.99999999999999645, -115.0000000000000000, 162.9999999999999716 ) ) ;
#26267 = B_SPLINE_CURVE_WITH_KNOTS ( 'NONE', 3,
 ( #4682, #29081, #10759, #16107 ),
 .UNSPECIFIED., .F., .F.,
 ( 4, 4 ),
 ( 1.991136383990134541E-07, 0.0003071994222346450588 ),
 .UNSPECIFIED. ) ;
#26268 = AXIS2_PLACEMENT_3D ( 'NONE', #29608, #2889, #5203 ) ;
#26270 = ORIENTED_EDGE ( 'NONE', *, *, #18854, .T. ) ;
#26269 = VECTOR ( 'NONE', #2227, 1000.000000000000000 ) ;
#26271 = AXIS2_PLACEMENT_3D ( 'NONE', #19161, #11676, #804 ) ;
#26272 = CYLINDRICAL_SURFACE ( 'NONE', #29092, 1.649999999999999911 ) ;
#26273 = CARTESIAN_POINT ( 'NONE',  ( -6.195103562623470712E-16, -30.61407293071429336, 1.706449706642247932 ) ) ;
#26274 = EDGE_CURVE ( 'NONE', #8875, #34985, #22609, .T. ) ;
#26275 = EDGE_CURVE ( 'NONE', #27741, #7441, #27583, .T. ) ;
#26276 = ORIENTED_EDGE ( 'NONE', *, *, #15048, .F. ) ;
#26277 = EDGE_CURVE ( 'NONE', #392, #9284, #24048, .T. ) ;
#26278 = EDGE_CURVE ( 'NONE', #1290, #18216, #23501, .T. ) ;
#26279 = DIRECTION ( 'NONE',  ( -7.893605728314051750E-14, 1.618803117314786530E-15, 1.000000000000000000 ) ) ;
#26280 = ORIENTED_EDGE ( 'NONE', *, *, #26746, .T. ) ;
#26281 = CARTESIAN_POINT ( 'NONE',  ( 108.5044842081497194, -4.558675695222540902, 11.64123453730966595 ) ) ;
#26282 = ORIENTED_EDGE ( 'NONE', *, *, #26278, .F. ) ;
#26283 = CARTESIAN_POINT ( 'NONE',  ( 1.039999999999999813, -24.90160365674851661, -23.75493189058366994 ) ) ;
#26284 = DIRECTION ( 'NONE',  ( 1.300283923313630633E-47, 0.000000000000000000, 1.000000000000000000 ) ) ;
#26285 = CARTESIAN_POINT ( 'NONE',  ( 1.749999999999999778, -33.39989884085085237, -8.296590337300626672 ) ) ;
#26286 = CARTESIAN_POINT ( 'NONE',  ( -355.0000000000000000, 118.9999999999999858, 128.0000000000000000 ) ) ;
#26287 = ORIENTED_EDGE ( 'NONE', *, *, #15040, .F. ) ;
#26288 = ORIENTED_EDGE ( 'NONE', *, *, #24314, .T. ) ;
#26289 = ORIENTED_EDGE ( 'NONE', *, *, #31304, .F. ) ;
#26290 = PRODUCT_DEFINITION_SHAPE ( 'NONE', 'NONE',  #35115 ) ;
#26291 = CARTESIAN_POINT ( 'NONE',  ( 2.789999999999999147, 23.53611639059738536, -19.35207786518964213 ) ) ;
#26292 = EDGE_CURVE ( 'NONE', #30412, #5400, #17283, .T. ) ;
#26293 = DIRECTION ( 'NONE',  ( -3.040835319149746090E-31, -1.000000000000000000, 0.000000000000000000 ) ) ;
#26294 = VECTOR ( 'NONE', #10576, 1000.000000000000000 ) ;
#26295 = LINE ( 'NONE', #17786, #11085 ) ;
#26296 = DIRECTION ( 'NONE',  ( -0.000000000000000000, -1.000000000000000000, -0.000000000000000000 ) ) ;
#26297 = CIRCLE ( 'NONE', #20072, 2.036051781435510577 ) ;
#26298 = COLOUR_RGB ( '',0.7921568627450980005, 0.8196078431372548767, 0.9333333333333333481 ) ;
#26299 = DIRECTION ( 'NONE',  ( 0.000000000000000000, 0.8443279255020087470, 0.5358267949790064266 ) ) ;
#26300 = VECTOR ( 'NONE', #28244, 1000.000000000000000 ) ;
#26301 = CARTESIAN_POINT ( 'NONE',  ( -35.00000000000000000, 42.49491490430484220, 36.69637551990492597 ) ) ;
#26302 = ORIENTED_EDGE ( 'NONE', *, *, #16795, .F. ) ;
#26303 = DIRECTION ( 'NONE',  ( 1.000000000000000000, 0.000000000000000000, -1.848892746611746966E-32 ) ) ;
#26304 = CARTESIAN_POINT ( 'NONE',  ( 11.99999999999999645, -145.0000000000000000, -194.9999999999999432 ) ) ;
#26305 = CARTESIAN_POINT ( 'NONE',  ( -3.250000000000000000, -5.838643359331793015, -0.7500000000000000000 ) ) ;
#26307 = ADVANCED_FACE ( 'NONE', ( #713 ), #28115, .T. ) ;
#26306 = ORIENTED_EDGE ( 'NONE', *, *, #10436, .F. ) ;
#26308 = EDGE_CURVE ( 'NONE', #16671, #30104, #33627, .T. ) ;
#26309 = CARTESIAN_POINT ( 'NONE',  ( 0.000000000000000000, 1.974842713994612024E-15, 76.74945698428001606 ) ) ;
#26310 = ORIENTED_EDGE ( 'NONE', *, *, #30444, .T. ) ;
#26311 = CARTESIAN_POINT ( 'NONE',  ( -442.0000000000000000, -105.0000000000000142, -174.9999999999999716 ) ) ;
#26312 = CARTESIAN_POINT ( 'NONE',  ( 27.99209646187090783, 25.49206711720158225, 49.43553178847298568 ) ) ;
#26313 = DIRECTION ( 'NONE',  ( 0.000000000000000000, 1.836970198721029688E-16, -1.000000000000000000 ) ) ;
#26314 = DIRECTION ( 'NONE',  ( -0.3193015301359797831, 0.9476531711828025673, 0.000000000000000000 ) ) ;
#26315 = VERTEX_POINT ( 'NONE', #14251 ) ;
#26316 = AXIS2_PLACEMENT_3D ( 'NONE', #26889, #18728, #21725 ) ;
#26317 = ORIENTED_EDGE ( 'NONE', *, *, #10010, .F. ) ;
#26318 = AXIS2_PLACEMENT_3D ( 'NONE', #29736, #10165, #32567 ) ;
#26319 = EDGE_CURVE ( 'NONE', #17362, #9284, #11576, .T. ) ;
#26320 = EDGE_CURVE ( 'NONE', #11743, #2097, #22429, .T. ) ;
#26321 = DIRECTION ( 'NONE',  ( -0.2702158583041252560, 0.9627997662655328748, -1.430125741367718248E-14 ) ) ;
#26322 = AXIS2_PLACEMENT_3D ( 'NONE', #1496, #26568, #9676 ) ;
#26323 = ORIENTED_EDGE ( 'NONE', *, *, #7584, .F. ) ;
#26324 = EDGE_CURVE ( 'NONE', #27638, #30062, #19411, .T. ) ;
#26325 = CARTESIAN_POINT ( 'NONE',  ( -143.0000000000000568, -89.01471862576147487, 43.40376782973931569 ) ) ;
#26326 = CARTESIAN_POINT ( 'NONE',  ( -355.0000000000000000, -131.0000000000000000, 130.0000000000000000 ) ) ;
#26327 = DIRECTION ( 'NONE',  ( -1.000000000000000000, 0.000000000000000000, 0.000000000000000000 ) ) ;
#26328 = ITEM_DEFINED_TRANSFORMATION ( 'NONE', 'NONE', #30875,  #28566 ) ;
#26329 = ORIENTED_EDGE ( 'NONE', *, *, #32646, .T. ) ;
#26330 = CARTESIAN_POINT ( 'NONE',  ( 1.749999999999999778, 0.000000000000000000, 0.000000000000000000 ) ) ;
#26331 = VECTOR ( 'NONE', #5540, 1000.000000000000000 ) ;
#26333 = FACE_OUTER_BOUND ( 'NONE', #23298, .T. ) ;
#26332 = CARTESIAN_POINT ( 'NONE',  ( 99.26191511054632599, 0.000000000000000000, 60.00000000000000000 ) ) ;
#26334 = ORIENTED_EDGE ( 'NONE', *, *, #6303, .T. ) ;
#26335 = ORIENTED_EDGE ( 'NONE', *, *, #28216, .F. ) ;
#26336 = DIRECTION ( 'NONE',  ( 0.000000000000000000, 0.000000000000000000, -1.000000000000000000 ) ) ;
#26337 = ORIENTED_EDGE ( 'NONE', *, *, #21165, .T. ) ;
#26338 = DIRECTION ( 'NONE',  ( 1.000000000000000000, 0.000000000000000000, 1.300283923313630633E-47 ) ) ;
#26339 = DIRECTION ( 'NONE',  ( 0.000000000000000000, 0.000000000000000000, 1.000000000000000000 ) ) ;
#26340 = ORIENTED_EDGE ( 'NONE', *, *, #4485, .F. ) ;
#26341 = ADVANCED_FACE ( 'NONE', ( #11391, #22250, #6388 ), #14783, .T. ) ;
#26342 = AXIS2_PLACEMENT_3D ( 'NONE', #9778, #20811, #12638 ) ;
#26343 = ADVANCED_FACE ( 'NONE', ( #33093 ), #30612, .F. ) ;
#26344 = FACE_OUTER_BOUND ( 'NONE', #8230, .T. ) ;
#26345 = VECTOR ( 'NONE', #27935, 1000.000000000000000 ) ;
#26346 = PRODUCT_DEFINITION_SHAPE ( 'NONE', 'NONE',  #35206 ) ;
#26347 = ORIENTED_EDGE ( 'NONE', *, *, #8059, .F. ) ;
#26348 = CARTESIAN_POINT ( 'NONE',  ( 50.00050000000000239, 0.000000000000000000, 0.000000000000000000 ) ) ;
#26349 = CARTESIAN_POINT ( 'NONE',  ( -349.0000000000000000, -125.0000000000000284, 181.0000000000000000 ) ) ;
#26350 = EDGE_CURVE ( 'NONE', #19234, #19763, #14430, .T. ) ;
#26351 = DIRECTION ( 'NONE',  ( -1.000000000000000000, -0.000000000000000000, 0.000000000000000000 ) ) ;
#26353 = CARTESIAN_POINT ( 'NONE',  ( 22.89764159710613001, 4.274639749586560455, -77.50000000000000000 ) ) ;
#26352 = CARTESIAN_POINT ( 'NONE',  ( -441.9999999999999432, 104.9999999999999858, -190.9999999999999716 ) ) ;
#26354 = EDGE_CURVE ( 'NONE', #6786, #29803, #894, .T. ) ;
#26356 = EDGE_CURVE ( 'NONE', #32541, #8838, #16750, .T. ) ;
#26355 = CARTESIAN_POINT ( 'NONE',  ( 1.991296462759137853, -32.48444414290483451, 68.31122994652405112 ) ) ;
#26357 = PLANE ( 'NONE',  #18293 ) ;
#26358 = LINE ( 'NONE', #34196, #16182 ) ;
#26359 = DIRECTION ( 'NONE',  ( 0.2675283385292205884, 0.9635499925192231307, 1.770012621235684308E-16 ) ) ;
#26360 = CIRCLE ( 'NONE', #32606, 15.00000000000000000 ) ;
#26361 = VERTEX_POINT ( 'NONE', #20115 ) ;
#26362 = SHAPE_REPRESENTATION_RELATIONSHIP ( 'NONE' , 'NONE' ,  #29156, #19498 ) ;
#26363 = ORIENTED_EDGE ( 'NONE', *, *, #6464, .F. ) ;
#26364 = VERTEX_POINT ( 'NONE', #22075 ) ;
#26365 = TOROIDAL_SURFACE ( 'NONE', #9887, 30.47050528711511674, 8.000000000000000000 ) ;
#26366 = CARTESIAN_POINT ( 'NONE',  ( 108.7751028178685431, 4.336304859840375059, 6.126759150192703451 ) ) ;
#26367 = DIRECTION ( 'NONE',  ( 0.000000000000000000, 0.000000000000000000, 1.000000000000000000 ) ) ;
#26368 = VECTOR ( 'NONE', #21335, 1000.000000000000000 ) ;
#26369 = VERTEX_POINT ( 'NONE', #32916 ) ;
#26370 = ORIENTED_EDGE ( 'NONE', *, *, #3463, .T. ) ;
#26371 = EDGE_LOOP ( 'NONE', ( #21384, #21294, #9213, #15756 ) ) ;
#26372 = CARTESIAN_POINT ( 'NONE',  ( -7.700000000000000178, 1.922695474661344271E-15, 15.69999999999999929 ) ) ;
#26373 = AXIS2_PLACEMENT_3D ( 'NONE', #26326, #4779, #18862 ) ;
#26374 = ORIENTED_EDGE ( 'NONE', *, *, #32921, .F. ) ;
#26375 = DIRECTION ( 'NONE',  ( 0.000000000000000000, 0.000000000000000000, -1.000000000000000000 ) ) ;
#26376 = DIRECTION ( 'NONE',  ( -0.000000000000000000, -0.000000000000000000, -1.000000000000000000 ) ) ;
#26377 = VERTEX_POINT ( 'NONE', #16929 ) ;
#26378 = ORIENTED_EDGE ( 'NONE', *, *, #6899, .F. ) ;
#26379 = CARTESIAN_POINT ( 'NONE',  ( -8.203566206536489625E-14, 4.061185680397187525, 30.39260865248091292 ) ) ;
#26380 = DIRECTION ( 'NONE',  ( 1.000000000000000000, 0.000000000000000000, 0.000000000000000000 ) ) ;
#26381 = CARTESIAN_POINT ( 'NONE',  ( -410.0000000000000568, -105.0000000000000142, 162.9999999999999716 ) ) ;
#26382 = DIRECTION ( 'NONE',  ( -1.000000000000000000, 0.000000000000000000, 0.000000000000000000 ) ) ;
#26383 = DIRECTION ( 'NONE',  ( -1.000000000000000000, 0.000000000000000000, 0.000000000000000000 ) ) ;
#26384 = ORIENTED_EDGE ( 'NONE', *, *, #16139, .T. ) ;
#26385 = EDGE_CURVE ( 'NONE', #16134, #34303, #5881, .T. ) ;
#26386 = CARTESIAN_POINT ( 'NONE',  ( 19.99999999999998934, 124.9999999999999716, 187.0000000000000000 ) ) ;
#26387 = LINE ( 'NONE', #29055, #35025 ) ;
#26388 = ADVANCED_FACE ( 'NONE', ( #24903 ), #540, .T. ) ;
#26389 = VECTOR ( 'NONE', #17959, 1000.000000000000000 ) ;
#26390 = VERTEX_POINT ( 'NONE', #15302 ) ;
#26391 = DIRECTION ( 'NONE',  ( 0.000000000000000000, 1.000000000000000000, 1.224646799147353207E-16 ) ) ;
#26392 = DIRECTION ( 'NONE',  ( 1.000000000000000000, 0.000000000000000000, 0.000000000000000000 ) ) ;
#26393 = CIRCLE ( 'NONE', #15758, 2.085824230283342740 ) ;
#26394 = FACE_OUTER_BOUND ( 'NONE', #21776, .T. ) ;
#26396 = CARTESIAN_POINT ( 'NONE',  ( -106.3672936988086235, 4.940661300061105266, -5.643441299694564428 ) ) ;
#26395 = CARTESIAN_POINT ( 'NONE',  ( -30.76765767668601725, -10.60922306139171667, 68.31122994652405112 ) ) ;
#26397 = VECTOR ( 'NONE', #33491, 1000.000000000000000 ) ;
#26398 = AXIS2_PLACEMENT_3D ( 'NONE', #8186, #2846, #32227 ) ;
#26399 = LINE ( 'NONE', #15214, #30338 ) ;
#26400 = VERTEX_POINT ( 'NONE', #26135 ) ;
#26401 = CARTESIAN_POINT ( 'NONE',  ( 99.26191511054632599, -6.978196330887525654E-16, -12.50000000000000000 ) ) ;
#26403 = CARTESIAN_POINT ( 'NONE',  ( 0.006871052814942861346, 30.38119646769583682, 5.469045072945091235 ) ) ;
#26402 = DIRECTION ( 'NONE',  ( 1.000000000000000000, 0.000000000000000000, 0.000000000000000000 ) ) ;
#26404 = ORIENTED_EDGE ( 'NONE', *, *, #33790, .F. ) ;
#26405 = CARTESIAN_POINT ( 'NONE',  ( -4.850000000000000533, 0.000000000000000000, -0.7520000000000004459 ) ) ;
#26406 = ORIENTED_EDGE ( 'NONE', *, *, #16343, .F. ) ;
#26407 = CIRCLE ( 'NONE', #839, 34.41491905851385269 ) ;
#26408 = VERTEX_POINT ( 'NONE', #7429 ) ;
#26409 = DIRECTION ( 'NONE',  ( 0.000000000000000000, 0.000000000000000000, -1.000000000000000000 ) ) ;
#26410 = ORIENTED_EDGE ( 'NONE', *, *, #3211, .F. ) ;
#26411 = ORIENTED_EDGE ( 'NONE', *, *, #11144, .T. ) ;
#26412 = LINE ( 'NONE', #12912, #29262 ) ;
#26413 = CIRCLE ( 'NONE', #15086, 4.000000000000003553 ) ;
#26414 = VERTEX_POINT ( 'NONE', #29072 ) ;
#26415 = AXIS2_PLACEMENT_3D ( 'NONE', #13844, #32223, #34541 ) ;
#26416 = PLANE ( 'NONE',  #7700 ) ;
#26417 = CARTESIAN_POINT ( 'NONE',  ( -414.0000000000000568, -125.0000000000000000, 187.0000000000000000 ) ) ;
#26418 = VERTEX_POINT ( 'NONE', #4410 ) ;
#26419 = ORIENTED_EDGE ( 'NONE', *, *, #3205, .F. ) ;
#26420 = CIRCLE ( 'NONE', #13379, 2.525000000000000799 ) ;
#26421 = DIRECTION ( 'NONE',  ( 0.000000000000000000, -1.000000000000000000, -1.310824597558155437E-49 ) ) ;
#26422 = DIRECTION ( 'NONE',  ( -1.000000000000000000, 0.000000000000000000, -0.000000000000000000 ) ) ;
#26423 = ADVANCED_FACE ( 'NONE', ( #1752 ), #6910, .F. ) ;
#26424 = DIRECTION ( 'NONE',  ( -3.469446951953832974E-18, -1.000000000000000000, -7.888609052210116302E-31 ) ) ;
#26425 = DIRECTION ( 'NONE',  ( 0.000000000000000000, 0.000000000000000000, 1.000000000000000000 ) ) ;
#26426 = VERTEX_POINT ( 'NONE', #15127 ) ;
#26427 = ORIENTED_EDGE ( 'NONE', *, *, #26098, .T. ) ;
#26428 = LINE ( 'NONE', #32459, #33257 ) ;
#26429 = EDGE_CURVE ( 'NONE', #8179, #11374, #21273, .T. ) ;
#26430 = DIRECTION ( 'NONE',  ( -1.000000000000000000, -0.000000000000000000, -0.000000000000000000 ) ) ;
#26431 = VERTEX_POINT ( 'NONE', #28634 ) ;
#26432 = ADVANCED_FACE ( 'NONE', ( #20979, #18328 ), #12811, .T. ) ;
#26433 = CARTESIAN_POINT ( 'NONE',  ( -441.9999999999999432, 109.0000000000000142, 154.9999999999999716 ) ) ;
#26434 = LINE ( 'NONE', #5060, #26269 ) ;
#26435 = CARTESIAN_POINT ( 'NONE',  ( 2.033800797852382658, -17.72251720152513244, -28.91628452940461713 ) ) ;
#26436 = ORIENTED_EDGE ( 'NONE', *, *, #1248, .F. ) ;
#26437 = CARTESIAN_POINT ( 'NONE',  ( -9.978866888775527855, 8.235406450278427215, -67.50000000000000000 ) ) ;
#26438 = ORIENTED_EDGE ( 'NONE', *, *, #14271, .T. ) ;
#26439 = CIRCLE ( 'NONE', #3137, 3.999999999999976019 ) ;
#26440 = AXIS2_PLACEMENT_3D ( 'NONE', #34452, #28589, #33931 ) ;
#26441 = CARTESIAN_POINT ( 'NONE',  ( 27.99209646187092559, 25.49206711720156093, 49.43553178847298568 ) ) ;
#26442 = ORIENTED_EDGE ( 'NONE', *, *, #17027, .F. ) ;
#26443 = DIRECTION ( 'NONE',  ( -1.000000000000000000, -0.000000000000000000, 0.000000000000000000 ) ) ;
#26444 = AXIS2_PLACEMENT_3D ( 'NONE', #29852, #18660, #15820 ) ;
#26445 = DIRECTION ( 'NONE',  ( -0.000000000000000000, -1.000000000000000000, -0.000000000000000000 ) ) ;
#26446 = CARTESIAN_POINT ( 'NONE',  ( 0.006871051457199655287, -11.06504178053304699, 28.81826507853126174 ) ) ;
#26447 = ORIENTED_EDGE ( 'NONE', *, *, #20061, .T. ) ;
#26448 = VECTOR ( 'NONE', #7045, 1000.000000000000114 ) ;
#26449 = DIRECTION ( 'NONE',  ( 0.000000000000000000, -1.000000000000000000, 0.000000000000000000 ) ) ;
#26450 = AXIS2_PLACEMENT_3D ( 'NONE', #2373, #15395, #13254 ) ;
#26451 = DIRECTION ( 'NONE',  ( 0.000000000000000000, 0.000000000000000000, 1.000000000000000000 ) ) ;
#26452 = CLOSED_SHELL ( 'NONE', ( #30065, #18374, #28994, #26106, #12989, #3178, #12503, #5164, #29546, #3725, #21452, #15002, #30685, #9146, #9148, #26543, #16895, #5378, #34389, #278, #28056, #4768, #17789, #20823, #32409, #12027, #28730, #25594, #30894, #33637, #34429, #8789, #27069, #31951, #27832, #6673, #12947, #3892, #23335, #3559, #24695, #14269, #12, #29406, #26125, #26886, #33887, #20258, #21343, #5552, #23828, #14122, #6707, #13473, #23853, #15398, #18771, #34969, #9789, #16767, #6722, #18105, #6281, #28418, #17636, #18582, #11679, #27445, #2913, #14132, #8744, #23111, #33476, #6807, #2368, #10679, #24942, #32143, #7360, #34082, #13876, #30026, #3074, #112, #14313, #12860, #32482, #11250, #1207, #22875, #34379, #19757, #32931, #7842, #9357, #10462, #10461, #13946, #7749, #33100, #19173, #26732, #25391, #27354, #27162, #7010, #4926, #8033, #11442, #26307, #4805, #22460, #13633, #32083, #29029, #23494, #21162, #5018, #8986, #29163, #25130, #16055, #20185, #24042, #11452, #30474, #25914, #21715, #26165, #23043, #28606, #14396, #30772, #3596, #21950, #7175, #3668, #13347, #26991, #14119, #13260, #27751, #5068, #32044, #34023, #30251, #25212, #23577, #12112, #28006, #1057, #3496, #3808, #34360, #1633, #12750, #11827, #14374, #13731, #6132, #2807, #6613, #18232, #8061, #23631, #21324, #602, #24051 ) ) ;
#26453 = ORIENTED_EDGE ( 'NONE', *, *, #11533, .F. ) ;
#26454 = CARTESIAN_POINT ( 'NONE',  ( 770.5235556396739867, 1210.493767280993552, 1753.598338701303646 ) ) ;
#26455 = ORIENTED_EDGE ( 'NONE', *, *, #19569, .T. ) ;
#26456 = CARTESIAN_POINT ( 'NONE',  ( 11.99999999999999645, -141.0000000000000000, 155.0000000000000000 ) ) ;
#26457 = ORIENTED_EDGE ( 'NONE', *, *, #17425, .F. ) ;
#26458 = PLANE ( 'NONE',  #29214 ) ;
#26459 = DIRECTION ( 'NONE',  ( 0.000000000000000000, 2.309213040847544338E-50, 1.000000000000000000 ) ) ;
#26460 = CARTESIAN_POINT ( 'NONE',  ( -12.00000000000001066, 112.9999999999999574, 155.0000000000000000 ) ) ;
#26461 = DIRECTION ( 'NONE',  ( -1.000000000000000000, 0.000000000000000000, 0.000000000000000000 ) ) ;
#26462 = ORIENTED_EDGE ( 'NONE', *, *, #8949, .T. ) ;
#26463 = ORIENTED_EDGE ( 'NONE', *, *, #33298, .F. ) ;
#26464 = EDGE_LOOP ( 'NONE', ( #363, #9295, #29314, #12441 ) ) ;
#26465 = CARTESIAN_POINT ( 'NONE',  ( 0.1835379745812393826, 26.80070150627937053, 17.97639020990316183 ) ) ;
#26466 = VECTOR ( 'NONE', #22856, 1000.000000000000114 ) ;
#26467 = EDGE_CURVE ( 'NONE', #949, #10663, #31748, .T. ) ;
#26468 = DIRECTION ( 'NONE',  ( 0.000000000000000000, -2.312964634635743450E-15, -1.000000000000000000 ) ) ;
#26469 = DIRECTION ( 'NONE',  ( -1.000000000000000000, -0.000000000000000000, -0.000000000000000000 ) ) ;
#26470 = DIRECTION ( 'NONE',  ( 0.000000000000000000, 0.000000000000000000, 1.000000000000000000 ) ) ;
#26472 = DIRECTION ( 'NONE',  ( 0.6051742151937651304, 0.7960930657056438653, -0.000000000000000000 ) ) ;
#26471 =( REPRESENTATION_RELATIONSHIP ('NONE','NONE', #23037, #15767 ) REPRESENTATION_RELATIONSHIP_WITH_TRANSFORMATION ( #8867 )SHAPE_REPRESENTATION_RELATIONSHIP( ) );
#26473 = CARTESIAN_POINT ( 'NONE',  ( 2.789999999999999147, 9.869977788041397915, -30.37666815053925973 ) ) ;
#26474 = ORIENTED_EDGE ( 'NONE', *, *, #20066, .F. ) ;
#26475 = EDGE_CURVE ( 'NONE', #5041, #17164, #28464, .T. ) ;
#26476 = B_SPLINE_CURVE_WITH_KNOTS ( 'NONE', 3,
 ( #20160, #6607, #9474, #20332 ),
 .UNSPECIFIED., .F., .F.,
 ( 4, 4 ),
 ( 1.989389905266797354E-07, 0.002009632881715329999 ),
 .UNSPECIFIED. ) ;
#26477 = FACE_OUTER_BOUND ( 'NONE', #19470, .T. ) ;
#26478 = EDGE_CURVE ( 'NONE', #31238, #19439, #9769, .T. ) ;
#26479 = CARTESIAN_POINT ( 'NONE',  ( 117.4999999999998579, 1.530808498934191521E-15, -12.50000000000000000 ) ) ;
#26480 = CARTESIAN_POINT ( 'NONE',  ( 10.96230482721425403, -14.55883922869198166, -87.50000000000000000 ) ) ;
#26481 = ORIENTED_EDGE ( 'NONE', *, *, #28166, .F. ) ;
#26482 = AXIS2_PLACEMENT_3D ( 'NONE', #1350, #34083, #6840 ) ;
#26483 = EDGE_CURVE ( 'NONE', #27613, #11423, #14388, .T. ) ;
#26484 = EDGE_CURVE ( 'NONE', #1716, #4705, #12752, .T. ) ;
#26485 = CARTESIAN_POINT ( 'NONE',  ( -1.105377996166861548E-15, -1.318430554028759305, -13.49999999999999645 ) ) ;
#26486 = ORIENTED_EDGE ( 'NONE', *, *, #17131, .F. ) ;
#26487 = CARTESIAN_POINT ( 'NONE',  ( 3.235562306570555532E-30, 24.02303923978504940, -67.50000000000000000 ) ) ;
#26488 = ADVANCED_FACE ( 'NONE', ( #23465 ), #23303, .T. ) ;
#26489 = LINE ( 'NONE', #2109, #34925 ) ;
#26490 = VECTOR ( 'NONE', #11462, 1000.000000000000000 ) ;
#26491 = ORIENTED_EDGE ( 'NONE', *, *, #22673, .T. ) ;
#26492 = DIRECTION ( 'NONE',  ( 3.469446951953832974E-18, 1.000000000000000000, 7.888609052210116302E-31 ) ) ;
#26493 = FACE_OUTER_BOUND ( 'NONE', #12355, .T. ) ;
#26494 = LINE ( 'NONE', #34685, #2378 ) ;
#26495 = VECTOR ( 'NONE', #16348, 1000.000000000000227 ) ;
#26496 = VERTEX_POINT ( 'NONE', #1239 ) ;
#26497 = ORIENTED_EDGE ( 'NONE', *, *, #32697, .T. ) ;
#26498 = DIRECTION ( 'NONE',  ( -5.458687100362422193E-14, 4.493539838443968466E-14, 0.9999999999999998890 ) ) ;
#26499 = ORIENTED_EDGE ( 'NONE', *, *, #968, .F. ) ;
#26500 = AXIS2_PLACEMENT_3D ( 'NONE', #7746, #18633, #26265 ) ;
#26501 = CARTESIAN_POINT ( 'NONE',  ( 1.040000000000002256, 27.68252950111368094, -20.44661865013457813 ) ) ;
#26502 = DIRECTION ( 'NONE',  ( -3.469446951953832974E-18, -1.000000000000000000, -7.888609052210116302E-31 ) ) ;
#26503 = CARTESIAN_POINT ( 'NONE',  ( -37.58721499952019940, -4.609089608337735733, -36.68877005347593467 ) ) ;
#26504 = CARTESIAN_POINT ( 'NONE',  ( 0.000000000000000000, 3.214697847761802057E-14, -87.50000000000000000 ) ) ;
#26505 = ITEM_DEFINED_TRANSFORMATION ( 'NONE', 'NONE', #1300,  #28566 ) ;
#26506 = ORIENTED_EDGE ( 'NONE', *, *, #13947, .T. ) ;
#26507 = DIRECTION ( 'NONE',  ( -0.9075754196709575616, 0.4198891015602634891, -0.000000000000000000 ) ) ;
#26508 = AXIS2_PLACEMENT_3D ( 'NONE', #10012, #31716, #13219 ) ;
#26510 = DIRECTION ( 'NONE',  ( 0.000000000000000000, 1.836970198721029688E-16, -1.000000000000000000 ) ) ;
#26509 = DIRECTION ( 'NONE',  ( 0.000000000000000000, 0.000000000000000000, -1.000000000000000000 ) ) ;
#26511 = VERTEX_POINT ( 'NONE', #17802 ) ;
#26512 = VERTEX_POINT ( 'NONE', #22955 ) ;
#26513 = CARTESIAN_POINT ( 'NONE',  ( 2.789999999999999147, 0.000000000000000000, 0.000000000000000000 ) ) ;
#26514 = VERTEX_POINT ( 'NONE', #33807 ) ;
#26515 = VECTOR ( 'NONE', #16654, 1000.000000000000000 ) ;
#26516 = FACE_OUTER_BOUND ( 'NONE', #20, .T. ) ;
#26517 = CARTESIAN_POINT ( 'NONE',  ( 2.719051659807903754, 31.23788557484581574, -5.357780584450596351 ) ) ;
#26518 = ORIENTED_EDGE ( 'NONE', *, *, #12190, .F. ) ;
#26519 = CARTESIAN_POINT ( 'NONE',  ( 145.0000000000000568, -189.5512933739568666, -180.0000000000000284 ) ) ;
#26520 = EDGE_CURVE ( 'NONE', #25461, #19525, #25815, .T. ) ;
#26521 = EDGE_CURVE ( 'NONE', #28106, #19565, #26933, .T. ) ;
#26522 = ORIENTED_EDGE ( 'NONE', *, *, #7420, .T. ) ;
#26523 = VECTOR ( 'NONE', #7521, 1000.000000000000227 ) ;
#26524 = FACE_OUTER_BOUND ( 'NONE', #26180, .T. ) ;
#26525 = CARTESIAN_POINT ( 'NONE',  ( 26.04754872656012310, -19.51229300245306320, 49.43553178847298568 ) ) ;
#26526 = CARTESIAN_POINT ( 'NONE',  ( 22.89764159710611224, 17.63622956525712127, -77.50000000000000000 ) ) ;
#26528 = CARTESIAN_POINT ( 'NONE',  ( -445.9999999999999432, -105.0000000000000142, 107.9999999999999858 ) ) ;
#26527 = DIRECTION ( 'NONE',  ( 0.000000000000000000, 0.000000000000000000, 1.000000000000000000 ) ) ;
#26529 = CARTESIAN_POINT ( 'NONE',  ( -441.9999999999999432, 105.0000000000000000, -73.99999999999998579 ) ) ;
#26530 = CYLINDRICAL_SURFACE ( 'NONE', #9735, 9.999999999999998224 ) ;
#26531 = CYLINDRICAL_SURFACE ( 'NONE', #17335, 16.19999999999999574 ) ;
#26532 = CARTESIAN_POINT ( 'NONE',  ( 2.789999999999999147, 17.11426446101199161, 26.96776559937732642 ) ) ;
#26533 = PRODUCT_DEFINITION_SHAPE ( 'NONE', 'NONE',  #35191 ) ;
#26534 = AXIS2_PLACEMENT_3D ( 'NONE', #34182, #9801, #18188 ) ;
#26535 = ADVANCED_FACE ( 'NONE', ( #12287, #31301 ), #25786, .F. ) ;
#26536 = AXIS2_PLACEMENT_3D ( 'NONE', #13527, #172, #11026 ) ;
#26537 = ORIENTED_EDGE ( 'NONE', *, *, #22567, .T. ) ;
#26538 = CARTESIAN_POINT ( 'NONE',  ( 824.8301442019729848, 989.3487216806448714, 1723.356790487177705 ) ) ;
#26539 = ORIENTED_EDGE ( 'NONE', *, *, #17155, .F. ) ;
#26541 = ORIENTED_EDGE ( 'NONE', *, *, #12162, .T. ) ;
#26540 = ADVANCED_FACE ( 'NONE', ( #20802 ), #31647, .F. ) ;
#26542 = EDGE_CURVE ( 'NONE', #11811, #20392, #1928, .T. ) ;
#26543 = ADVANCED_FACE ( 'NONE', ( #26663 ), #28081, .T. ) ;
#26544 = DIRECTION ( 'NONE',  ( 0.000000000000000000, 7.888609052210118054E-31, 1.000000000000000000 ) ) ;
#26545 =( NAMED_UNIT ( * ) PLANE_ANGLE_UNIT ( ) SI_UNIT ( $, .RADIAN. ) );
#26546 = ORIENTED_EDGE ( 'NONE', *, *, #28719, .F. ) ;
#26547 = ORIENTED_EDGE ( 'NONE', *, *, #28078, .T. ) ;
#26548 = CARTESIAN_POINT ( 'NONE',  ( -5.588430218784975857E-16, 20.82898695786893484, 22.50081875905981121 ) ) ;
#26549 = DIRECTION ( 'NONE',  ( -0.000000000000000000, -0.000000000000000000, -1.000000000000000000 ) ) ;
#26550 = ADVANCED_FACE ( 'NONE', ( #2273 ), #13664, .F. ) ;
#26551 = DIRECTION ( 'NONE',  ( 0.000000000000000000, 0.000000000000000000, -1.000000000000000000 ) ) ;
#26552 = LINE ( 'NONE', #11022, #33037 ) ;
#26553 = VERTEX_POINT ( 'NONE', #7607 ) ;
#26554 = ORIENTED_EDGE ( 'NONE', *, *, #21684, .T. ) ;
#26555 = DIRECTION ( 'NONE',  ( -0.000000000000000000, 1.836970198721029934E-16, -1.000000000000000000 ) ) ;
#26556 = LINE ( 'NONE', #10894, #26621 ) ;
#26557 = CARTESIAN_POINT ( 'NONE',  ( 0.5248941326870452118, 31.31301644755022551, 11.56311898902757385 ) ) ;
#26558 = DIRECTION ( 'NONE',  ( -0.000000000000000000, -0.000000000000000000, -1.000000000000000000 ) ) ;
#26559 = LINE ( 'NONE', #10195, #34749 ) ;
#26560 = ORIENTED_EDGE ( 'NONE', *, *, #2412, .T. ) ;
#26562 = AXIS2_PLACEMENT_3D ( 'NONE', #7508, #31889, #2704 ) ;
#26561 = DIRECTION ( 'NONE',  ( 0.000000000000000000, 1.131431318426415506E-52, 1.000000000000000000 ) ) ;
#26564 = LINE ( 'NONE', #12709, #22492 ) ;
#26563 = CIRCLE ( 'NONE', #24858, 7.999999999999992895 ) ;
#26565 = ADVANCED_FACE ( 'NONE', ( #10290 ), #21152, .T. ) ;
#26566 = DIRECTION ( 'NONE',  ( -1.000000000000000000, 0.000000000000000000, 0.000000000000000000 ) ) ;
#26567 = DIRECTION ( 'NONE',  ( 0.000000000000000000, 0.000000000000000000, 1.000000000000000000 ) ) ;
#26568 = DIRECTION ( 'NONE',  ( 1.000000000000000000, 3.469446951953834515E-18, 0.000000000000000000 ) ) ;
#26569 = AXIS2_PLACEMENT_3D ( 'NONE', #23805, #9927, #34484 ) ;
#26571 = FACE_OUTER_BOUND ( 'NONE', #23570, .T. ) ;
#26570 = DIRECTION ( 'NONE',  ( -0.6473862847818285804, -0.7621620551276356847, -0.000000000000000000 ) ) ;
#26572 = CARTESIAN_POINT ( 'NONE',  ( 2.033589657429622388, 27.12319051591943619, -20.36165095825642979 ) ) ;
#26573 = ORIENTED_EDGE ( 'NONE', *, *, #18712, .F. ) ;
#26574 = DIRECTION ( 'NONE',  ( 0.000000000000000000, 0.000000000000000000, 1.000000000000000000 ) ) ;
#26576 = DIRECTION ( 'NONE',  ( 0.000000000000000000, 0.000000000000000000, -1.000000000000000000 ) ) ;
#26575 = FACE_OUTER_BOUND ( 'NONE', #35007, .T. ) ;
#26577 = VECTOR ( 'NONE', #8637, 1000.000000000000000 ) ;
#26578 = ORIENTED_EDGE ( 'NONE', *, *, #7289, .F. ) ;
#26579 = CARTESIAN_POINT ( 'NONE',  ( 0.000000000000000000, 0.000000000000000000, 0.000000000000000000 ) ) ;
#26580 = ADVANCED_FACE ( 'NONE', ( #13151 ), #18509, .F. ) ;
#26581 = ORIENTED_EDGE ( 'NONE', *, *, #163, .T. ) ;
#26582 = ADVANCED_FACE ( 'NONE', ( #21507, #8812, #18678 ), #24498, .F. ) ;
#26583 = VECTOR ( 'NONE', #2285, 1000.000000000000000 ) ;
#26584 = CIRCLE ( 'NONE', #15819, 9.999999999999998224 ) ;
#26585 = ADVANCED_FACE ( 'NONE', ( #32349 ), #29688, .T. ) ;
#26586 = ORIENTED_EDGE ( 'NONE', *, *, #31544, .T. ) ;
#26587 = CYLINDRICAL_SURFACE ( 'NONE', #19083, 16.19999999999999574 ) ;
#26588 = VERTEX_POINT ( 'NONE', #19200 ) ;
#26589 = EDGE_LOOP ( 'NONE', ( #18272, #25065, #910, #3690 ) ) ;
#26590 = CARTESIAN_POINT ( 'NONE',  ( -445.9999999999999432, -104.9999999999999858, -162.9999999999999716 ) ) ;
#26591 = AXIS2_PLACEMENT_3D ( 'NONE', #8257, #26598, #21615 ) ;
#26592 = FACE_OUTER_BOUND ( 'NONE', #12334, .T. ) ;
#26593 = DIRECTION ( 'NONE',  ( 0.000000000000000000, 0.000000000000000000, -1.000000000000000000 ) ) ;
#26594 = EDGE_LOOP ( 'NONE', ( #1885, #9817, #2696, #30347 ) ) ;
#26595 = ORIENTED_EDGE ( 'NONE', *, *, #10665, .F. ) ;
#26596 = LINE ( 'NONE', #34618, #9455 ) ;
#26597 = DIRECTION ( 'NONE',  ( -1.000000000000000000, 0.000000000000000000, 0.000000000000000000 ) ) ;
#26598 = DIRECTION ( 'NONE',  ( 1.000000000000000000, 0.000000000000000000, 0.000000000000000000 ) ) ;
#26599 = FACE_OUTER_BOUND ( 'NONE', #30584, .T. ) ;
#26600 = DIRECTION ( 'NONE',  ( 0.000000000000000000, -5.053935297177146739E-49, -1.000000000000000000 ) ) ;
#26601 = UNCERTAINTY_MEASURE_WITH_UNIT (LENGTH_MEASURE( 1.000000000000000082E-05 ), #14230, 'distance_accuracy_value', 'NONE');
#26602 = VERTEX_POINT ( 'NONE', #32517 ) ;
#26603 = LINE ( 'NONE', #22417, #3703 ) ;
#26604 = CIRCLE ( 'NONE', #28862, 9.999999999999994671 ) ;
#26605 = DIRECTION ( 'NONE',  ( 0.000000000000000000, 0.000000000000000000, 1.000000000000000000 ) ) ;
#26606 = ORIENTED_EDGE ( 'NONE', *, *, #1635, .F. ) ;
#26607 = CARTESIAN_POINT ( 'NONE',  ( -7.700000000000000178, 0.000000000000000000, -10.30000000000000071 ) ) ;
#26608 = CARTESIAN_POINT ( 'NONE',  ( 12.00000000000001066, -60.99999999999997158, -154.9999999999999716 ) ) ;
#26609 = CARTESIAN_POINT ( 'NONE',  ( 2.606462082920441681, -16.25808774470336715, -27.87656317279346041 ) ) ;
#26610 = EDGE_LOOP ( 'NONE', ( #33426, #14444, #771, #3812, #3254 ) ) ;
#26611 = CARTESIAN_POINT ( 'NONE',  ( 2.789999999999999147, 0.000000000000000000, 0.000000000000000000 ) ) ;
#26612 = ORIENTED_EDGE ( 'NONE', *, *, #1889, .F. ) ;
#26613 = AXIS2_PLACEMENT_3D ( 'NONE', #17645, #28478, #9616 ) ;
#26614 =( GEOMETRIC_REPRESENTATION_CONTEXT ( 3 ) GLOBAL_UNCERTAINTY_ASSIGNED_CONTEXT ( ( #26601 ) ) GLOBAL_UNIT_ASSIGNED_CONTEXT ( ( #14230, #12091, #33787 ) ) REPRESENTATION_CONTEXT ( 'NONE', 'WORKASPACE' ) );
#26615 = DIRECTION ( 'NONE',  ( 0.000000000000000000, -1.000000000000000000, -2.465190328815662439E-32 ) ) ;
#26616 = ORIENTED_EDGE ( 'NONE', *, *, #11341, .T. ) ;
#26617 = EDGE_CURVE ( 'NONE', #22809, #9452, #7964, .T. ) ;
#26619 = CARTESIAN_POINT ( 'NONE',  ( 19.99999999999998934, -55.00000000000000711, 162.9999999999999716 ) ) ;
#26618 = LINE ( 'NONE', #16135, #14278 ) ;
#26620 = LINE ( 'NONE', #95, #29033 ) ;
#26621 = VECTOR ( 'NONE', #29411, 1000.000000000000000 ) ;
#26622 = EDGE_LOOP ( 'NONE', ( #19396, #26287, #21243, #1085 ) ) ;
#26623 = DIRECTION ( 'NONE',  ( -0.000000000000000000, -1.000000000000000000, -0.000000000000000000 ) ) ;
#26624 = CARTESIAN_POINT ( 'NONE',  ( -12.00000000000001066, 108.9999999999999858, 155.0000000000000000 ) ) ;
#26625 = ADVANCED_FACE ( 'NONE', ( #16000 ), #18842, .T. ) ;
#26626 = ORIENTED_EDGE ( 'NONE', *, *, #33988, .T. ) ;
#26627 = CIRCLE ( 'NONE', #6732, 2.500000000000002220 ) ;
#26628 = ADVANCED_FACE ( 'NONE', ( #2448 ), #13330, .T. ) ;
#26629 = EDGE_CURVE ( 'NONE', #27996, #32587, #5111, .T. ) ;
#26630 = VECTOR ( 'NONE', #5005, 1000.000000000000000 ) ;
#26631 = DIRECTION ( 'NONE',  ( -7.893605728314051750E-14, 1.618803117314786530E-15, 1.000000000000000000 ) ) ;
#26632 = ORIENTED_EDGE ( 'NONE', *, *, #12799, .F. ) ;
#26633 = CARTESIAN_POINT ( 'NONE',  ( 110.7380848894536598, 7.027127293105233764E-16, 12.50000000000000000 ) ) ;
#26634 = EDGE_CURVE ( 'NONE', #13451, #34913, #6121, .T. ) ;
#26635 = ORIENTED_EDGE ( 'NONE', *, *, #23149, .T. ) ;
#26636 = DIRECTION ( 'NONE',  ( 1.000000000000000000, 0.000000000000000000, 0.000000000000000000 ) ) ;
#26637 = DIRECTION ( 'NONE',  ( 0.000000000000000000, 2.309213040847544338E-50, 1.000000000000000000 ) ) ;
#26638 = AXIS2_PLACEMENT_3D ( 'NONE', #9218, #19734, #16901 ) ;
#26639 = CARTESIAN_POINT ( 'NONE',  ( -100.1618820091562014, -1.694081942180570177, -7.313267332261218279 ) ) ;
#26640 = LINE ( 'NONE', #15102, #19367 ) ;
#26641 = CONTEXT_DEPENDENT_SHAPE_REPRESENTATION ( #15569, #30771 ) ;
#26642 = ORIENTED_EDGE ( 'NONE', *, *, #27164, .T. ) ;
#26643 = EDGE_LOOP ( 'NONE', ( #13403, #16834, #33786, #20742 ) ) ;
#26644 = PRODUCT_DEFINITION_SHAPE ( 'NONE', 'NONE',  #35234 ) ;
#26645 = ORIENTED_EDGE ( 'NONE', *, *, #25270, .F. ) ;
#26646 = CYLINDRICAL_SURFACE ( 'NONE', #32127, 34.41491905851385269 ) ;
#26647 = CARTESIAN_POINT ( 'NONE',  ( 1.039999999999999813, 21.72796464722045684, -26.68861566460872226 ) ) ;
#26648 = CARTESIAN_POINT ( 'NONE',  ( 11.99999999999995559, -145.0000000000000000, -194.9999999999999432 ) ) ;
#26649 = AXIS2_PLACEMENT_3D ( 'NONE', #20240, #14553, #11699 ) ;
#26650 = PLANE ( 'NONE',  #15667 ) ;
#26651 = FACE_OUTER_BOUND ( 'NONE', #13118, .T. ) ;
#26652 = CARTESIAN_POINT ( 'NONE',  ( -18.07349068442144358, -27.06572199953721736, 68.31122994652405112 ) ) ;
#26653 = LINE ( 'NONE', #9755, #12822 ) ;
#26654 = ORIENTED_EDGE ( 'NONE', *, *, #15255, .F. ) ;
#26655 = DIRECTION ( 'NONE',  ( -3.040835319149746090E-31, -1.000000000000000000, 0.000000000000000000 ) ) ;
#26656 = DIRECTION ( 'NONE',  ( -0.000000000000000000, -0.000000000000000000, -1.000000000000000000 ) ) ;
#26657 = CARTESIAN_POINT ( 'NONE',  ( -20.00000000000004619, -134.9999999999999716, -162.9999999999999432 ) ) ;
#26658 = ORIENTED_EDGE ( 'NONE', *, *, #417, .T. ) ;
#26659 = AXIS2_PLACEMENT_3D ( 'NONE', #4595, #13355, #5312 ) ;
#26660 = FACE_OUTER_BOUND ( 'NONE', #26817, .T. ) ;
#26661 = EDGE_LOOP ( 'NONE', ( #8032, #23493 ) ) ;
#26662 = LINE ( 'NONE', #29519, #6908 ) ;
#26663 = FACE_OUTER_BOUND ( 'NONE', #31581, .T. ) ;
#26664 = VECTOR ( 'NONE', #5693, 1000.000000000000000 ) ;
#26665 = VERTEX_POINT ( 'NONE', #16178 ) ;
#26666 = EDGE_CURVE ( 'NONE', #29934, #1639, #26489, .T. ) ;
#26667 = CYLINDRICAL_SURFACE ( 'NONE', #30779, 10.00000000000000000 ) ;
#26668 = CARTESIAN_POINT ( 'NONE',  ( -414.0000000000000568, -125.0000000000000000, 162.9999999999999716 ) ) ;
#26669 = LINE ( 'NONE', #15482, #27385 ) ;
#26670 = EDGE_CURVE ( 'NONE', #6869, #32274, #8176, .T. ) ;
#26671 = ORIENTED_EDGE ( 'NONE', *, *, #11010, .T. ) ;
#26672 = CIRCLE ( 'NONE', #34070, 1.999999999999999556 ) ;
#26673 = ORIENTED_EDGE ( 'NONE', *, *, #6965, .T. ) ;
#26674 = DIRECTION ( 'NONE',  ( -0.1063910735369017202, 0.9943243633099136947, -1.000770725407181676E-14 ) ) ;
#26675 = EDGE_CURVE ( 'NONE', #9976, #25461, #20379, .T. ) ;
#26676 = ORIENTED_EDGE ( 'NONE', *, *, #5419, .T. ) ;
#26677 = CARTESIAN_POINT ( 'NONE',  ( 1.040000000000001590, 34.10861917999616111, 4.581348211832199091 ) ) ;
#26678 = CYLINDRICAL_SURFACE ( 'NONE', #10748, 1.999999999999999112 ) ;
#26679 = AXIS2_PLACEMENT_3D ( 'NONE', #24802, #436, #8784 ) ;
#26680 = FACE_OUTER_BOUND ( 'NONE', #29224, .T. ) ;
#26681 = DIRECTION ( 'NONE',  ( 1.000000000000000000, 0.000000000000000000, 0.000000000000000000 ) ) ;
#26682 = EDGE_CURVE ( 'NONE', #31475, #21040, #16526, .T. ) ;
#26683 = VERTEX_POINT ( 'NONE', #9158 ) ;
#26684 = B_SPLINE_CURVE_WITH_KNOTS ( 'NONE', 3,
 ( #19881, #11511, #30723, #33022 ),
 .UNSPECIFIED., .F., .F.,
 ( 4, 4 ),
 ( 0.005298347429621244956, 0.005985216133920617451 ),
 .UNSPECIFIED. ) ;
#26685 = CYLINDRICAL_SURFACE ( 'NONE', #21519, 3.999999999999976019 ) ;
#26686 = ADVANCED_FACE ( 'NONE', ( #20209 ), #4208, .T. ) ;
#26687 = EDGE_CURVE ( 'NONE', #31871, #5830, #31056, .T. ) ;
#26689 = DIRECTION ( 'NONE',  ( 0.000000000000000000, 1.836970198721029688E-16, -1.000000000000000000 ) ) ;
#26688 = CARTESIAN_POINT ( 'NONE',  ( 15.44711578872682267, -28.64595934308655600, 68.31122994652405112 ) ) ;
#26690 = ORIENTED_EDGE ( 'NONE', *, *, #26993, .T. ) ;
#26691 = ORIENTED_EDGE ( 'NONE', *, *, #22789, .F. ) ;
#26692 = CARTESIAN_POINT ( 'NONE',  ( 27.99209646187092559, 25.49206711720156093, 68.31122994652405112 ) ) ;
#26693 = ORIENTED_EDGE ( 'NONE', *, *, #32655, .F. ) ;
#26694 = DIRECTION ( 'NONE',  ( 0.000000000000000000, 1.000000000000000000, 1.131431318426415506E-52 ) ) ;
#26695 = CARTESIAN_POINT ( 'NONE',  ( 2.765921099433442443, 30.61125888652969707, -5.439165181698684570 ) ) ;
#26696 = VERTEX_POINT ( 'NONE', #981 ) ;
#26697 = AXIS2_PLACEMENT_3D ( 'NONE', #25224, #30928, #12080 ) ;
#26698 = CARTESIAN_POINT ( 'NONE',  ( -20.00000000000007461, 140.9999999999999432, -162.9999999999999716 ) ) ;
#26699 = DIRECTION ( 'NONE',  ( 0.1617819965527614312, -0.9868265225415265851, -0.000000000000000000 ) ) ;
#26700 = ORIENTED_EDGE ( 'NONE', *, *, #29558, .T. ) ;
#26701 = CARTESIAN_POINT ( 'NONE',  ( -32.71222340678873053, 19.07754906224033675, 68.31122994652405112 ) ) ;
#26702 = CARTESIAN_POINT ( 'NONE',  ( -442.0000000000000000, -125.0000000000000000, 107.9999999999999858 ) ) ;
#26703 = CARTESIAN_POINT ( 'NONE',  ( 2.765921099433442887, -26.45933846664205902, 16.32596387352436551 ) ) ;
#26705 = DIRECTION ( 'NONE',  ( -1.300283923313630633E-47, 0.000000000000000000, -1.000000000000000000 ) ) ;
#26704 = DIRECTION ( 'NONE',  ( 0.000000000000000000, -1.000000000000000000, -1.836970198721029934E-16 ) ) ;
#26706 = LINE ( 'NONE', #21381, #25637 ) ;
#26707 = CARTESIAN_POINT ( 'NONE',  ( 0.006892465017757970838, -0.3207854480229822558, 30.86813304286355475 ) ) ;
#26708 = DIRECTION ( 'NONE',  ( -1.292961597001347186E-16, -0.000000000000000000, 1.000000000000000000 ) ) ;
#26709 = ORIENTED_EDGE ( 'NONE', *, *, #12859, .F. ) ;
#26710 = CARTESIAN_POINT ( 'NONE',  ( -499.9999999999998863, -109.0000000000000142, -187.0000000000000000 ) ) ;
#26711 = CARTESIAN_POINT ( 'NONE',  ( 823.6058462861761882, 1287.191891031011437, 1753.598338701302964 ) ) ;
#26712 = PRODUCT_DEFINITION_CONTEXT ( 'detailed design', #9642, 'design' ) ;
#26713 = ORIENTED_EDGE ( 'NONE', *, *, #3202, .T. ) ;
#26714 = VERTEX_POINT ( 'NONE', #17377 ) ;
#26715 = EDGE_CURVE ( 'NONE', #8985, #32587, #24076, .T. ) ;
#26716 = CIRCLE ( 'NONE', #11384, 34.41491905851385269 ) ;
#26717 = EDGE_CURVE ( 'NONE', #27275, #23058, #20142, .T. ) ;
#26718 = CARTESIAN_POINT ( 'NONE',  ( -430.0000000000000000, 130.9999999999999716, 109.9999999999999858 ) ) ;
#26719 = EDGE_CURVE ( 'NONE', #31417, #18709, #24661, .T. ) ;
#26720 = DIRECTION ( 'NONE',  ( 1.584970850963694453E-14, 3.204900912403111222E-14, 1.000000000000000000 ) ) ;
#26721 = ORIENTED_EDGE ( 'NONE', *, *, #12707, .T. ) ;
#26722 = CARTESIAN_POINT ( 'NONE',  ( 22.89764159710615132, -5.651112684911595352, -87.50000000000000000 ) ) ;
#26723 = CARTESIAN_POINT ( 'NONE',  ( -12.00000000000001066, -32.99999999999997158, -154.9999999999999716 ) ) ;
#26724 = DIRECTION ( 'NONE',  ( 0.000000000000000000, 1.000000000000000000, 1.224646799147353207E-16 ) ) ;
#26725 = ORIENTED_EDGE ( 'NONE', *, *, #26277, .T. ) ;
#26726 = EDGE_LOOP ( 'NONE', ( #24268, #25504, #8965, #548 ) ) ;
#26727 =( REPRESENTATION_RELATIONSHIP ('NONE','NONE', #23037, #28231 ) REPRESENTATION_RELATIONSHIP_WITH_TRANSFORMATION ( #1473 )SHAPE_REPRESENTATION_RELATIONSHIP( ) );
#26728 = CARTESIAN_POINT ( 'NONE',  ( 0.02407890056655608360, 4.286445725888036407, 30.79383171238946204 ) ) ;
#26729 = CARTESIAN_POINT ( 'NONE',  ( 0.000000000000000000, 6.992329373473909019E-15, 49.43553178847298568 ) ) ;
#26730 = CARTESIAN_POINT ( 'NONE',  ( 44.94043929807611448, -20.15143121711728469, 20.00000000000000000 ) ) ;
#26732 = ADVANCED_FACE ( 'NONE', ( #14871 ), #6294, .T. ) ;
#26731 = PLANE ( 'NONE',  #30748 ) ;
#26733 = DIRECTION ( 'NONE',  ( 0.000000000000000000, 0.000000000000000000, 1.000000000000000000 ) ) ;
#26734 = ORIENTED_EDGE ( 'NONE', *, *, #17735, .T. ) ;
#26735 = FACE_OUTER_BOUND ( 'NONE', #13493, .T. ) ;
#26736 = CARTESIAN_POINT ( 'NONE',  ( -499.9999999999999432, -141.0000000000000000, -187.0000000000000000 ) ) ;
#26737 = CARTESIAN_POINT ( 'NONE',  ( 19.99999999999998224, 134.9999999999999432, -162.9999999999999432 ) ) ;
#26738 = VECTOR ( 'NONE', #25553, 1000.000000000000000 ) ;
#26739 = DIRECTION ( 'NONE',  ( -1.000000000000000000, -0.000000000000000000, -0.000000000000000000 ) ) ;
#26740 = EDGE_CURVE ( 'NONE', #26683, #29298, #13309, .T. ) ;
#26741 = CARTESIAN_POINT ( 'NONE',  ( -262.5000000000000000, 0.000000000000000000, 0.000000000000000000 ) ) ;
#26742 = VECTOR ( 'NONE', #21821, 1000.000000000000000 ) ;
#26743 = CARTESIAN_POINT ( 'NONE',  ( -345.0000000000000000, -125.0000000000000284, 181.0000000000000000 ) ) ;
#26745 = DIRECTION ( 'NONE',  ( 0.000000000000000000, 1.836970198721029441E-16, -1.000000000000000000 ) ) ;
#26744 = CARTESIAN_POINT ( 'NONE',  ( 2.789999999999999147, 23.28319895603611300, -19.33937915510192695 ) ) ;
#26746 = EDGE_CURVE ( 'NONE', #29991, #4421, #18444, .T. ) ;
#26747 = EDGE_CURVE ( 'NONE', #2399, #20453, #30703, .T. ) ;
#26748 = CARTESIAN_POINT ( 'NONE',  ( 1.749999999999999778, 14.40815186467820475, -31.25366880301303496 ) ) ;
#26749 = ORIENTED_EDGE ( 'NONE', *, *, #22506, .F. ) ;
#26750 = CARTESIAN_POINT ( 'NONE',  ( 100.3425380856783278, 3.356865266134898995, -12.04189187465341782 ) ) ;
#26752 = DIRECTION ( 'NONE',  ( 0.4684084406997908734, -0.8835120444460226041, -1.622985295858433536E-16 ) ) ;
#26751 = CARTESIAN_POINT ( 'NONE',  ( -35.00000000000000000, 16.36947364650383818, 36.69637551990492597 ) ) ;
#26753 = ADVANCED_FACE ( 'NONE', ( #9341 ), #17197, .T. ) ;
#26754 = VERTEX_POINT ( 'NONE', #25525 ) ;
#26755 = VECTOR ( 'NONE', #31208, 1000.000000000000000 ) ;
#26756 = LINE ( 'NONE', #21951, #26294 ) ;
#26757 = VECTOR ( 'NONE', #34819, 1000.000000000000000 ) ;
#26758 = ORIENTED_EDGE ( 'NONE', *, *, #21101, .T. ) ;
#26759 = EDGE_CURVE ( 'NONE', #9246, #15148, #17024, .T. ) ;
#26760 = EDGE_CURVE ( 'NONE', #2924, #319, #12373, .T. ) ;
#26761 = ORIENTED_EDGE ( 'NONE', *, *, #18464, .F. ) ;
#26762 = DIRECTION ( 'NONE',  ( 0.000000000000000000, 0.000000000000000000, 1.000000000000000000 ) ) ;
#26763 = ORIENTED_EDGE ( 'NONE', *, *, #26319, .F. ) ;
#26764 = ORIENTED_EDGE ( 'NONE', *, *, #31700, .T. ) ;
#26765 = AXIS2_PLACEMENT_3D ( 'NONE', #4181, #22366, #33563 ) ;
#26766 = FACE_OUTER_BOUND ( 'NONE', #15811, .T. ) ;
#26767 = ADVANCED_FACE ( 'NONE', ( #22872 ), #14345, .T. ) ;
#26768 = LINE ( 'NONE', #23912, #34464 ) ;
#26769 = DIRECTION ( 'NONE',  ( -0.000000000000000000, -0.000000000000000000, -1.000000000000000000 ) ) ;
#26770 = ORIENTED_EDGE ( 'NONE', *, *, #5338, .T. ) ;
#26771 = VERTEX_POINT ( 'NONE', #25167 ) ;
#26772 = CARTESIAN_POINT ( 'NONE',  ( 19.99999999999998934, 136.9999999999999716, -155.0000000000000000 ) ) ;
#26773 = CARTESIAN_POINT ( 'NONE',  ( -355.0000000000000000, -119.0000000000000000, 126.0000000000000000 ) ) ;
#26774 = DIRECTION ( 'NONE',  ( -0.000000000000000000, -1.836970198721029688E-16, 1.000000000000000000 ) ) ;
#26775 = EDGE_LOOP ( 'NONE', ( #11530, #9127, #8534, #21626 ) ) ;
#26776 = DIRECTION ( 'NONE',  ( -1.000000000000000000, -0.000000000000000000, -0.000000000000000000 ) ) ;
#26777 = VECTOR ( 'NONE', #21541, 1000.000000000000000 ) ;
#26778 = DIRECTION ( 'NONE',  ( 0.000000000000000000, 0.5000000000000018874, 0.8660254037844374864 ) ) ;
#26779 = ORIENTED_EDGE ( 'NONE', *, *, #31805, .F. ) ;
#26780 = VECTOR ( 'NONE', #13026, 1000.000000000000000 ) ;
#26781 = AXIS2_PLACEMENT_3D ( 'NONE', #33320, #8752, #28334 ) ;
#26782 = B_SPLINE_CURVE_WITH_KNOTS ( 'NONE', 3,
 ( #3281, #26966, #20165, #8450, #3103, #24984 ),
 .UNSPECIFIED., .F., .F.,
 ( 4, 2, 4 ),
 ( 4.404817001606571728E-07, 0.001874269605587681586, 0.003748098729475202520 ),
 .UNSPECIFIED. ) ;
#26783 = FACE_OUTER_BOUND ( 'NONE', #19450, .T. ) ;
#26784 = CARTESIAN_POINT ( 'NONE',  ( -5.344999999999999751, 0.000000000000000000, 0.000000000000000000 ) ) ;
#26785 = PLANE ( 'NONE',  #18053 ) ;
#26786 = ORIENTED_EDGE ( 'NONE', *, *, #19366, .F. ) ;
#26787 = EDGE_CURVE ( 'NONE', #13518, #30135, #11671, .T. ) ;
#26788 = DIRECTION ( 'NONE',  ( 1.000000000000000000, 0.000000000000000000, 0.000000000000000000 ) ) ;
#26789 = ORIENTED_EDGE ( 'NONE', *, *, #22760, .F. ) ;
#26790 = ADVANCED_FACE ( 'NONE', ( #34420 ), #24070, .F. ) ;
#26791 = CARTESIAN_POINT ( 'NONE',  ( 5.021133111224576062, 16.12922284503174097, -87.50000000000000000 ) ) ;
#26792 = ORIENTED_EDGE ( 'NONE', *, *, #2719, .F. ) ;
#26793 = VECTOR ( 'NONE', #26383, 1000.000000000000000 ) ;
#26795 = CARTESIAN_POINT ( 'NONE',  ( 0.000000000000000000, 0.000000000000000000, 0.000000000000000000 ) ) ;
#26794 = DIRECTION ( 'NONE',  ( 0.000000000000000000, -0.9836764282395641379, 0.1799463379062027635 ) ) ;
#26796 = CARTESIAN_POINT ( 'NONE',  ( -418.0000000000000000, 104.9999999999999858, -194.9999999999999716 ) ) ;
#26797 = EDGE_CURVE ( 'NONE', #14082, #10047, #15386, .T. ) ;
#26798 = AXIS2_PLACEMENT_3D ( 'NONE', #28873, #14845, #34215 ) ;
#26799 = ORIENTED_EDGE ( 'NONE', *, *, #11715, .F. ) ;
#26800 = SURFACE_STYLE_USAGE ( .BOTH. , #2587 ) ;
#26801 = EDGE_CURVE ( 'NONE', #14308, #7716, #27092, .T. ) ;
#26802 = LINE ( 'NONE', #34647, #10884 ) ;
#26803 = EDGE_LOOP ( 'NONE', ( #26749, #28284, #25114, #17302, #31339, #26282, #16328, #30969 ) ) ;
#26804 = VECTOR ( 'NONE', #10817, 1000.000000000000000 ) ;
#26805 = DIRECTION ( 'NONE',  ( -0.1063910735369225230, 0.9943243633099118073, -1.000770725407345128E-14 ) ) ;
#26806 = VECTOR ( 'NONE', #30921, 1000.000000000000227 ) ;
#26808 = EDGE_LOOP ( 'NONE', ( #5260, #20691, #4643, #18304 ) ) ;
#26807 = AXIS2_PLACEMENT_3D ( 'NONE', #32479, #5250, #13114 ) ;
#26809 = CARTESIAN_POINT ( 'NONE',  ( -104.1334669544120715, 5.043966910541457516, 5.550724164612918621 ) ) ;
#26810 = VERTEX_POINT ( 'NONE', #34773 ) ;
#26811 = AXIS2_PLACEMENT_3D ( 'NONE', #14024, #3152, #9203 ) ;
#26812 = LINE ( 'NONE', #7937, #8189 ) ;
#26813 = CARTESIAN_POINT ( 'NONE',  ( -109.0391046861367244, -3.142556659824618404, -6.811296903636076649 ) ) ;
#26814 = CARTESIAN_POINT ( 'NONE',  ( -143.0000000000000568, -12.50000000000001066, 1.224646799147353217E-14 ) ) ;
#26815 = ORIENTED_EDGE ( 'NONE', *, *, #31322, .F. ) ;
#26816 = VERTEX_POINT ( 'NONE', #4326 ) ;
#26817 = EDGE_LOOP ( 'NONE', ( #3206, #26030, #7796, #15010 ) ) ;
#26818 = DIRECTION ( 'NONE',  ( 1.000000000000000000, 0.000000000000000000, 0.000000000000000000 ) ) ;
#26819 = EDGE_CURVE ( 'NONE', #1154, #32678, #23736, .T. ) ;
#26820 = FACE_OUTER_BOUND ( 'NONE', #10584, .T. ) ;
#26822 = LINE ( 'NONE', #2429, #3433 ) ;
#26821 = CIRCLE ( 'NONE', #14349, 2.500000000000002220 ) ;
#26823 = CARTESIAN_POINT ( 'NONE',  ( 2.789999999999999147, 0.000000000000000000, 0.000000000000000000 ) ) ;
#26824 = CYLINDRICAL_SURFACE ( 'NONE', #13762, 4.750000000000004441 ) ;
#26825 = DIRECTION ( 'NONE',  ( -0.000000000000000000, -0.000000000000000000, 1.000000000000000000 ) ) ;
#26826 = DIRECTION ( 'NONE',  ( 0.000000000000000000, 0.000000000000000000, -1.000000000000000000 ) ) ;
#26827 = ORIENTED_EDGE ( 'NONE', *, *, #6734, .T. ) ;
#26828 = EDGE_CURVE ( 'NONE', #13032, #6490, #15744, .T. ) ;
#26829 = CARTESIAN_POINT ( 'NONE',  ( 0.7561992110385835630, 21.20694131899082535, -26.46705060818936062 ) ) ;
#26830 = LINE ( 'NONE', #4930, #25690 ) ;
#26831 = ADVANCED_FACE ( 'NONE', ( #31904 ), #2193, .F. ) ;
#26832 = VECTOR ( 'NONE', #22385, 1000.000000000000000 ) ;
#26833 = DIRECTION ( 'NONE',  ( 0.000000000000000000, 1.000000000000000000, 2.309213040847544338E-50 ) ) ;
#26834 = ORIENTED_EDGE ( 'NONE', *, *, #24824, .F. ) ;
#26835 = EDGE_CURVE ( 'NONE', #2399, #29809, #33803, .T. ) ;
#26836 = CIRCLE ( 'NONE', #25121, 32.54542015209055705 ) ;
#26837 = CARTESIAN_POINT ( 'NONE',  ( 1.749999999999999778, 22.14447232807506438, 26.34405054495565679 ) ) ;
#26838 = ORIENTED_EDGE ( 'NONE', *, *, #12854, .F. ) ;
#26839 = CARTESIAN_POINT ( 'NONE',  ( -99.91820555927569103, 0.6742432172868390028, -12.48628981526124804 ) ) ;
#26840 = DIRECTION ( 'NONE',  ( 0.000000000000000000, 0.000000000000000000, -1.000000000000000000 ) ) ;
#26841 = ORIENTED_EDGE ( 'NONE', *, *, #8995, .T. ) ;
#26842 = CARTESIAN_POINT ( 'NONE',  ( -430.0000000000000000, -114.9999999999999858, 113.9999999999999858 ) ) ;
#26843 = CARTESIAN_POINT ( 'NONE',  ( -442.0000000000000000, 105.0000000000000000, -77.99999999999997158 ) ) ;
#26844 = CARTESIAN_POINT ( 'NONE',  ( -449.9999999999999432, 124.9999999999999574, -187.0000000000000000 ) ) ;
#26845 = ORIENTED_EDGE ( 'NONE', *, *, #32618, .T. ) ;
#26846 = ORIENTED_EDGE ( 'NONE', *, *, #30777, .T. ) ;
#26847 = DIRECTION ( 'NONE',  ( -7.893605728314050488E-14, 1.618803117314786135E-15, 0.9999999999999998890 ) ) ;
#26848 = CARTESIAN_POINT ( 'NONE',  ( 17.88561705399011714, -27.19023860642122514, 49.43553178847298568 ) ) ;
#26849 = VERTEX_POINT ( 'NONE', #24592 ) ;
#26850 = CARTESIAN_POINT ( 'NONE',  ( -418.0000000000000000, 104.9999999999999858, -155.0000000000000000 ) ) ;
#26851 = LINE ( 'NONE', #13165, #33422 ) ;
#26852 = CIRCLE ( 'NONE', #13250, 4.309328216469825001 ) ;
#26853 = DIRECTION ( 'NONE',  ( 1.000000000000000000, 0.000000000000000000, 0.000000000000000000 ) ) ;
#26854 = CARTESIAN_POINT ( 'NONE',  ( 103.4562544601546108, -5.539877390153430170, 5.057044031126181061 ) ) ;
#26856 = MECHANICAL_DESIGN_GEOMETRIC_PRESENTATION_REPRESENTATION (  '', ( #4676 ), #30260 ) ;
#26855 = ITEM_DEFINED_TRANSFORMATION ( 'NONE', 'NONE', #20068,  #28566 ) ;
#26857 = AXIS2_PLACEMENT_3D ( 'NONE', #24855, #492, #11350 ) ;
#26858 = ORIENTED_EDGE ( 'NONE', *, *, #5118, .F. ) ;
#26859 = DIRECTION ( 'NONE',  ( -1.000000000000000000, -0.000000000000000000, 0.000000000000000000 ) ) ;
#26861 = CARTESIAN_POINT ( 'NONE',  ( 129.3530333899765594, -6.000000000000000000, -57.49999999999999289 ) ) ;
#26860 = DIRECTION ( 'NONE',  ( -1.000000000000000000, 0.000000000000000000, 0.000000000000000000 ) ) ;
#26862 = VERTEX_POINT ( 'NONE', #5547 ) ;
#26863 = VERTEX_POINT ( 'NONE', #32957 ) ;
#26864 = CARTESIAN_POINT ( 'NONE',  ( -35.00000000000000000, -46.95407462254104303, 36.69637551990492597 ) ) ;
#26865 = EDGE_CURVE ( 'NONE', #33296, #13606, #8056, .T. ) ;
#26866 = ORIENTED_EDGE ( 'NONE', *, *, #30914, .T. ) ;
#26867 = EDGE_CURVE ( 'NONE', #2667, #31399, #34352, .T. ) ;
#26868 = CARTESIAN_POINT ( 'NONE',  ( -499.9999999999999432, -113.0000000000000000, -187.0000000000000000 ) ) ;
#26869 = CARTESIAN_POINT ( 'NONE',  ( 5.021133111224679091, 24.02303923978504940, -67.50000000000000000 ) ) ;
#26870 = ORIENTED_EDGE ( 'NONE', *, *, #22135, .T. ) ;
#26871 = CARTESIAN_POINT ( 'NONE',  ( -361.0000000000000000, -125.0000000000000284, 110.0000000000000000 ) ) ;
#26872 = ADVANCED_FACE ( 'NONE', ( #18934 ), #10745, .T. ) ;
#26873 = CARTESIAN_POINT ( 'NONE',  ( 0.2204769333331085268, -13.33789614101574372, -3.898086217683921273 ) ) ;
#26874 = ORIENTED_EDGE ( 'NONE', *, *, #18810, .T. ) ;
#26875 = ADVANCED_FACE ( 'NONE', ( #32265 ), #19463, .T. ) ;
#26876 = CARTESIAN_POINT ( 'NONE',  ( -349.0000000000000000, -135.0000000000000000, 113.9999999999999858 ) ) ;
#26877 = CARTESIAN_POINT ( 'NONE',  ( -145.0000000000000568, -12.50000000000000888, -14.99999999999998757 ) ) ;
#26878 = DIRECTION ( 'NONE',  ( -0.000000000000000000, 1.000000000000000000, -0.000000000000000000 ) ) ;
#26879 = CARTESIAN_POINT ( 'NONE',  ( 22.10765473302597073, -14.55883922869198344, -77.50000000000000000 ) ) ;
#26880 = CIRCLE ( 'NONE', #9829, 3.999999999999948042 ) ;
#26881 = VECTOR ( 'NONE', #26708, 1000.000000000000000 ) ;
#26882 = VECTOR ( 'NONE', #15550, 1000.000000000000000 ) ;
#26883 = DIRECTION ( 'NONE',  ( -0.000000000000000000, 1.000000000000000000, -0.000000000000000000 ) ) ;
#26884 = DIRECTION ( 'NONE',  ( 0.000000000000000000, 5.053935297177146739E-49, 1.000000000000000000 ) ) ;
#26885 = CARTESIAN_POINT ( 'NONE',  ( -35.00000000000000000, -38.34433698000722046, -36.69637551990492597 ) ) ;
#26886 = ADVANCED_FACE ( 'NONE', ( #21759 ), #5383, .T. ) ;
#26887 = VERTEX_POINT ( 'NONE', #24781 ) ;
#26888 = CARTESIAN_POINT ( 'NONE',  ( 8.000000000000000000, 1.374666032042903655E-15, 11.22499999999999787 ) ) ;
#26889 = CARTESIAN_POINT ( 'NONE',  ( 787.0597240610745757, 1342.348721680648850, 1322.896119909291428 ) ) ;
#26890 = ORIENTED_EDGE ( 'NONE', *, *, #27311, .T. ) ;
#26891 = ORIENTED_EDGE ( 'NONE', *, *, #7167, .T. ) ;
#26892 = VECTOR ( 'NONE', #28379, 1000.000000000000000 ) ;
#26893 = DIRECTION ( 'NONE',  ( 0.000000000000000000, -0.000000000000000000, 1.000000000000000000 ) ) ;
#26894 =( LENGTH_UNIT ( ) NAMED_UNIT ( * ) SI_UNIT ( .MILLI., .METRE. ) );
#26895 = ORIENTED_EDGE ( 'NONE', *, *, #26617, .T. ) ;
#26896 = CARTESIAN_POINT ( 'NONE',  ( 11.99999999999999645, 124.9999999999999716, 155.0000000000000000 ) ) ;
#26898 = AXIS2_PLACEMENT_3D ( 'NONE', #21518, #32358, #7972 ) ;
#26897 = CONTEXT_DEPENDENT_SHAPE_REPRESENTATION ( #9895, #18420 ) ;
#26899 = FACE_OUTER_BOUND ( 'NONE', #1581, .T. ) ;
#26900 = AXIS2_PLACEMENT_3D ( 'NONE', #2753, #29817, #8802 ) ;
#26901 = ORIENTED_EDGE ( 'NONE', *, *, #13240, .F. ) ;
#26902 = ORIENTED_EDGE ( 'NONE', *, *, #29938, .F. ) ;
#26903 = CIRCLE ( 'NONE', #15008, 10.30000000000000071 ) ;
#26904 = CARTESIAN_POINT ( 'NONE',  ( 0.006871051546331624453, 7.365904273040736250, -29.97784191786578134 ) ) ;
#26905 = CARTESIAN_POINT ( 'NONE',  ( 0.000000000000000000, 3.524919873834583163E-15, 68.31122994652405112 ) ) ;
#26906 = EDGE_CURVE ( 'NONE', #3592, #1944, #30123, .T. ) ;
#26907 = DIRECTION ( 'NONE',  ( 0.000000000000000000, 1.836970198721029441E-16, -1.000000000000000000 ) ) ;
#26908 = CARTESIAN_POINT ( 'NONE',  ( 32.54460952423469422, 0.2297037030477265540, 68.31122994652405112 ) ) ;
#26909 = CARTESIAN_POINT ( 'NONE',  ( 0.000000000000000000, -13.59935610937992401, 28.90010281771827039 ) ) ;
#26910 = ORIENTED_EDGE ( 'NONE', *, *, #24288, .T. ) ;
#26911 = DIRECTION ( 'NONE',  ( 1.000000000000000000, 0.000000000000000000, 0.000000000000000000 ) ) ;
#26912 = DIRECTION ( 'NONE',  ( -0.000000000000000000, 0.8486862100397269959, 0.5288966977476833309 ) ) ;
#26913 = DIRECTION ( 'NONE',  ( 0.000000000000000000, 0.000000000000000000, -1.000000000000000000 ) ) ;
#26914 = EDGE_CURVE ( 'NONE', #16221, #31232, #21942, .T. ) ;
#26915 = DIRECTION ( 'NONE',  ( -0.000000000000000000, -0.000000000000000000, -1.000000000000000000 ) ) ;
#26916 = CARTESIAN_POINT ( 'NONE',  ( 9.736651044630743712, -33.69708579775584667, 49.43553178847298568 ) ) ;
#26917 = EDGE_CURVE ( 'NONE', #34661, #16142, #24249, .T. ) ;
#26918 = CARTESIAN_POINT ( 'NONE',  ( -11.99999999999998224, -145.0000000000000000, 155.0000000000000000 ) ) ;
#26920 = CARTESIAN_POINT ( 'NONE',  ( -7.176301005103106867, -1.505030548027689319, 0.000000000000000000 ) ) ;
#26919 = DIRECTION ( 'NONE',  ( 0.000000000000000000, 0.000000000000000000, 1.000000000000000000 ) ) ;
#26921 = AXIS2_PLACEMENT_3D ( 'NONE', #19967, #5886, #27612 ) ;
#26922 = ADVANCED_FACE ( 'NONE', ( #5902 ), #32790, .T. ) ;
#26923 = ADVANCED_FACE ( 'NONE', ( #16623 ), #21594, .F. ) ;
#26924 = CARTESIAN_POINT ( 'NONE',  ( -5.210000000000000853, 0.000000000000000000, 0.000000000000000000 ) ) ;
#26925 = ORIENTED_EDGE ( 'NONE', *, *, #24005, .F. ) ;
#26926 = CARTESIAN_POINT ( 'NONE',  ( -11.99999999999998224, -134.9999999999999716, 187.0000000000000000 ) ) ;
#26928 = CARTESIAN_POINT ( 'NONE',  ( -499.9999999999999432, 144.9999999999999716, -162.9999999999999716 ) ) ;
#26927 = DIRECTION ( 'NONE',  ( -0.000000000000000000, 0.8486862100397269959, 0.5288966977476833309 ) ) ;
#26929 =( GEOMETRIC_REPRESENTATION_CONTEXT ( 3 ) GLOBAL_UNCERTAINTY_ASSIGNED_CONTEXT ( ( #13208 ) ) GLOBAL_UNIT_ASSIGNED_CONTEXT ( ( #26894, #26545, #10540 ) ) REPRESENTATION_CONTEXT ( 'NONE', 'WORKASPACE' ) );
#26930 = B_SPLINE_CURVE_WITH_KNOTS ( 'NONE', 3,
 ( #29517, #23979, #34678, #13492 ),
 .UNSPECIFIED., .F., .F.,
 ( 4, 4 ),
 ( 2.128468106751623115E-07, 0.0006879486673519059079 ),
 .UNSPECIFIED. ) ;
#26932 = VERTEX_POINT ( 'NONE', #13589 ) ;
#26931 = VECTOR ( 'NONE', #21420, 1000.000000000000000 ) ;
#26933 = CIRCLE ( 'NONE', #16155, 3.999999999999976019 ) ;
#26934 = CYLINDRICAL_SURFACE ( 'NONE', #1849, 7.999999999999979572 ) ;
#26935 = PRODUCT_DEFINITION_SHAPE ( 'NONE', 'NONE',  #35246 ) ;
#26936 = ORIENTED_EDGE ( 'NONE', *, *, #22117, .F. ) ;
#26937 = EDGE_CURVE ( 'NONE', #5262, #33527, #11437, .T. ) ;
#26938 =( REPRESENTATION_RELATIONSHIP ('NONE','NONE', #23037, #15767 ) REPRESENTATION_RELATIONSHIP_WITH_TRANSFORMATION ( #4912 )SHAPE_REPRESENTATION_RELATIONSHIP( ) );
#26939 = ORIENTED_EDGE ( 'NONE', *, *, #3485, .T. ) ;
#26940 = FACE_OUTER_BOUND ( 'NONE', #265, .T. ) ;
#26941 = VERTEX_POINT ( 'NONE', #19118 ) ;
#26942 = ORIENTED_EDGE ( 'NONE', *, *, #3205, .T. ) ;
#26943 = LINE ( 'NONE', #26590, #9382 ) ;
#26944 = CIRCLE ( 'NONE', #29241, 7.999999999999979572 ) ;
#26945 = CARTESIAN_POINT ( 'NONE',  ( 8.485274312747499437, 31.41981051364775013, 68.31122994652405112 ) ) ;
#26946 = DIRECTION ( 'NONE',  ( 0.5611870653623828309, 0.8276889981568903432, 1.520440023423472778E-16 ) ) ;
#26947 = EDGE_LOOP ( 'NONE', ( #33132, #19233, #11749, #28332 ) ) ;
#26948 = EDGE_LOOP ( 'NONE', ( #18305, #15160, #32435, #22395 ) ) ;
#26949 = CARTESIAN_POINT ( 'NONE',  ( 0.7561992015540950351, -29.97203090897408018, -15.87187733271013990 ) ) ;
#26950 = CARTESIAN_POINT ( 'NONE',  ( -145.0000000000000568, -97.49999999999998579, 51.88904920397793319 ) ) ;
#26951 = AXIS2_PLACEMENT_3D ( 'NONE', #27040, #29541, #35066 ) ;
#26952 = CARTESIAN_POINT ( 'NONE',  ( 6.420643415959871274E-16, 11.49079834592231819, -28.42701364291157873 ) ) ;
#26953 = DIRECTION ( 'NONE',  ( -0.000000000000000000, -2.465190328815661892E-32, -1.000000000000000000 ) ) ;
#26954 = ORIENTED_EDGE ( 'NONE', *, *, #3446, .F. ) ;
#26955 = ORIENTED_EDGE ( 'NONE', *, *, #31303, .F. ) ;
#26956 = CARTESIAN_POINT ( 'NONE',  ( -345.0000000000000000, -125.0000000000000284, 181.0000000000000000 ) ) ;
#26957 = CIRCLE ( 'NONE', #4206, 7.999999999999979572 ) ;
#26958 = VECTOR ( 'NONE', #28853, 1000.000000000000000 ) ;
#26959 = DIRECTION ( 'NONE',  ( -1.000000000000000000, -0.000000000000000000, -0.000000000000000000 ) ) ;
#26960 = VERTEX_POINT ( 'NONE', #27457 ) ;
#26961 = AXIS2_PLACEMENT_3D ( 'NONE', #23836, #34693, #10306 ) ;
#26962 = DIRECTION ( 'NONE',  ( 1.000000000000000000, 0.000000000000000000, 0.000000000000000000 ) ) ;
#26963 = CARTESIAN_POINT ( 'NONE',  ( -418.0000000000000000, 124.9999999999999574, -187.0000000000000000 ) ) ;
#26964 = DIRECTION ( 'NONE',  ( 0.000000000000000000, 0.000000000000000000, 1.000000000000000000 ) ) ;
#26965 = ORIENTED_EDGE ( 'NONE', *, *, #8722, .F. ) ;
#26966 = CARTESIAN_POINT ( 'NONE',  ( 0.7564103445415252258, -32.71412841873081589, -8.947071897915261474 ) ) ;
#26967 = ORIENTED_EDGE ( 'NONE', *, *, #2125, .F. ) ;
#26968 = EDGE_CURVE ( 'NONE', #23318, #18383, #3065, .T. ) ;
#26969 = ADVANCED_FACE ( 'NONE', ( #27276 ), #2884, .F. ) ;
#26970 = DIRECTION ( 'NONE',  ( 1.000000000000000000, -0.000000000000000000, -0.000000000000000000 ) ) ;
#26971 = ORIENTED_EDGE ( 'NONE', *, *, #23435, .T. ) ;
#26973 =( NAMED_UNIT ( * ) SI_UNIT ( $, .STERADIAN. ) SOLID_ANGLE_UNIT ( ) );
#26972 = SURFACE_STYLE_FILL_AREA ( #34817 ) ;
#26974 = DIRECTION ( 'NONE',  ( 0.000000000000000000, -1.000000000000000000, -1.541976423090495633E-16 ) ) ;
#26975 = VECTOR ( 'NONE', #13429, 1000.000000000000000 ) ;
#26976 = EDGE_LOOP ( 'NONE', ( #28981, #20141, #13658, #6217, #11669, #9923 ) ) ;
#26977 = DIRECTION ( 'NONE',  ( -1.000000000000000000, -0.000000000000000000, -0.000000000000000000 ) ) ;
#26978 = CARTESIAN_POINT ( 'NONE',  ( 2.719051678294378327, 26.43909160613360854, 17.47815001432931226 ) ) ;
#26979 = AXIS2_PLACEMENT_3D ( 'NONE', #32019, #7635, #29896 ) ;
#26980 = VERTEX_POINT ( 'NONE', #18765 ) ;
#26981 = ADVANCED_FACE ( 'NONE', ( #29600 ), #31505, .T. ) ;
#26982 = AXIS2_PLACEMENT_3D ( 'NONE', #11829, #9657, #6267 ) ;
#26983 = AXIS2_PLACEMENT_3D ( 'NONE', #27452, #754, #25119 ) ;
#26984 = CIRCLE ( 'NONE', #13938, 2.000000000000001776 ) ;
#26985 = VERTEX_POINT ( 'NONE', #16090 ) ;
#26986 = DIRECTION ( 'NONE',  ( 0.000000000000000000, -1.000000000000000000, -1.836970198721029688E-16 ) ) ;
#26987 = LINE ( 'NONE', #2770, #6792 ) ;
#26988 = ORIENTED_EDGE ( 'NONE', *, *, #17544, .F. ) ;
#26989 = DIRECTION ( 'NONE',  ( 0.000000000000000000, 0.000000000000000000, -1.000000000000000000 ) ) ;
#26990 = TOROIDAL_SURFACE ( 'NONE', #9946, 30.47050528711511674, 8.000000000000000000 ) ;
#26991 = ADVANCED_FACE ( 'NONE', ( #1112 ), #27984, .F. ) ;
#26992 = ADVANCED_FACE ( 'NONE', ( #1287 ), #3936, .T. ) ;
#26993 = EDGE_CURVE ( 'NONE', #6886, #31215, #814, .T. ) ;
#26994 = CARTESIAN_POINT ( 'NONE',  ( -109.9311937893276365, -1.369675690685145719, -7.375755714855094958 ) ) ;
#26995 = CYLINDRICAL_SURFACE ( 'NONE', #16529, 2.000000000000001776 ) ;
#26996 = VERTEX_POINT ( 'NONE', #11627 ) ;
#26997 = ORIENTED_EDGE ( 'NONE', *, *, #11621, .F. ) ;
#26998 = EDGE_LOOP ( 'NONE', ( #16648, #32288, #31617, #18274 ) ) ;
#26999 = CARTESIAN_POINT ( 'NONE',  ( -0.9727285265192152641, -1.747512292859696670, 0.000000000000000000 ) ) ;
#27000 = CARTESIAN_POINT ( 'NONE',  ( -19.99999999999998934, 144.9999999999999716, -186.9999999999999716 ) ) ;
#27001 = ADVANCED_FACE ( 'NONE', ( #22298 ), #20334, .F. ) ;
#27002 = PLANE ( 'NONE',  #22282 ) ;
#27003 = TOROIDAL_SURFACE ( 'NONE', #4247, 30.47050528711511674, 8.000000000000000000 ) ;
#27004 = DIRECTION ( 'NONE',  ( 0.000000000000000000, 2.309213040847544338E-50, 1.000000000000000000 ) ) ;
#27005 = DIRECTION ( 'NONE',  ( 0.000000000000000000, 0.000000000000000000, 1.000000000000000000 ) ) ;
#27006 = DIRECTION ( 'NONE',  ( -1.000000000000000000, 0.000000000000000000, 0.000000000000000000 ) ) ;
#27007 = FACE_OUTER_BOUND ( 'NONE', #1933, .T. ) ;
#27008 = VERTEX_POINT ( 'NONE', #14824 ) ;
#27009 = LINE ( 'NONE', #35033, #24786 ) ;
#27010 = CARTESIAN_POINT ( 'NONE',  ( 0.1835379170796097859, -16.25808774470393914, 27.87656317279337514 ) ) ;
#27011 = CARTESIAN_POINT ( 'NONE',  ( 110.7380848894539866, -2.712459438615764475E-14, -7.500000000000241585 ) ) ;
#27012 = VERTEX_POINT ( 'NONE', #22823 ) ;
#27013 = VECTOR ( 'NONE', #7968, 1000.000000000000000 ) ;
#27014 = LINE ( 'NONE', #13326, #27446 ) ;
#27015 = ORIENTED_EDGE ( 'NONE', *, *, #4135, .T. ) ;
#27017 = CLOSED_SHELL ( 'NONE', ( #31600, #5277, #29977, #33700, #1322, #22710, #34194, #10041, #8318, #22787, #22604, #24292, #3734, #18672, #7384, #21946, #2280, #4771 ) ) ;
#27016 = DIRECTION ( 'NONE',  ( -0.9635499925192230197, 0.2675283385292207550, 0.000000000000000000 ) ) ;
#27018 = DIRECTION ( 'NONE',  ( -1.000000000000000000, -0.000000000000000000, 0.000000000000000000 ) ) ;
#27019 = VERTEX_POINT ( 'NONE', #3588 ) ;
#27020 = DIRECTION ( 'NONE',  ( 0.000000000000000000, 0.000000000000000000, -1.000000000000000000 ) ) ;
#27021 = CARTESIAN_POINT ( 'NONE',  ( 1.394999999999999574, 6.714005886384948774, 33.75364837705175347 ) ) ;
#27022 = LINE ( 'NONE', #28989, #22291 ) ;
#27023 = ORIENTED_EDGE ( 'NONE', *, *, #26629, .F. ) ;
#27024 = AXIS2_PLACEMENT_3D ( 'NONE', #10806, #29668, #35023 ) ;
#27025 = ORIENTED_EDGE ( 'NONE', *, *, #23714, .F. ) ;
#27026 = DIRECTION ( 'NONE',  ( 2.631470253772867002E-14, 1.478878779867888582E-15, 0.9999999999999998890 ) ) ;
#27027 = LINE ( 'NONE', #11364, #12160 ) ;
#27028 = VERTEX_POINT ( 'NONE', #16981 ) ;
#27029 = VECTOR ( 'NONE', #33885, 1000.000000000000000 ) ;
#27030 = DIRECTION ( 'NONE',  ( -0.000000000000000000, 1.000000000000000000, -0.000000000000000000 ) ) ;
#27031 = EDGE_CURVE ( 'NONE', #6498, #13611, #33144, .T. ) ;
#27032 = DIRECTION ( 'NONE',  ( 0.000000000000000000, 0.000000000000000000, -1.000000000000000000 ) ) ;
#27033 = EDGE_CURVE ( 'NONE', #10097, #9979, #27541, .T. ) ;
#27034 = LINE ( 'NONE', #13349, #29227 ) ;
#27035 = CARTESIAN_POINT ( 'NONE',  ( 110.4176386092808571, -1.928835813323004800, 7.257044673176061167 ) ) ;
#27036 = EDGE_LOOP ( 'NONE', ( #7492, #989, #11591, #4120 ) ) ;
#27037 = ORIENTED_EDGE ( 'NONE', *, *, #18854, .F. ) ;
#27038 = CARTESIAN_POINT ( 'NONE',  ( -418.0000000000000000, 113.0000000000000000, -175.0000000000000000 ) ) ;
#27039 = AXIS2_PLACEMENT_3D ( 'NONE', #17671, #17844, #15167 ) ;
#27041 = CARTESIAN_POINT ( 'NONE',  ( 0.000000000000000000, -44.99999999999995737, -36.68877005347594888 ) ) ;
#27040 = CARTESIAN_POINT ( 'NONE',  ( 11.99999999999995559, -134.9999999999999716, -186.9999999999999716 ) ) ;
#27042 = EDGE_LOOP ( 'NONE', ( #8579, #28343, #2033, #23344 ) ) ;
#27043 = ORIENTED_EDGE ( 'NONE', *, *, #24987, .F. ) ;
#27044 = DIRECTION ( 'NONE',  ( 0.000000000000000000, 1.000000000000000000, -3.374343856708137958E-53 ) ) ;
#27045 = EDGE_LOOP ( 'NONE', ( #10292, #9747, #30960, #646 ) ) ;
#27046 = CARTESIAN_POINT ( 'NONE',  ( 17.88561705399012780, -27.19023860642123935, 68.31122994652405112 ) ) ;
#27047 = CARTESIAN_POINT ( 'NONE',  ( -445.9999999999999432, 105.0000000000000142, 162.9999999999999716 ) ) ;
#27048 = ORIENTED_EDGE ( 'NONE', *, *, #13131, .F. ) ;
#27049 = VERTEX_POINT ( 'NONE', #19642 ) ;
#27050 = CIRCLE ( 'NONE', #13418, 1.999999999999999556 ) ;
#27051 = DIRECTION ( 'NONE',  ( 0.000000000000000000, 0.000000000000000000, 1.000000000000000000 ) ) ;
#27052 = CYLINDRICAL_SURFACE ( 'NONE', #22314, 7.999999999999979572 ) ;
#27053 = ORIENTED_EDGE ( 'NONE', *, *, #18265, .T. ) ;
#27054 = VECTOR ( 'NONE', #37, 1000.000000000000000 ) ;
#27055 = CARTESIAN_POINT ( 'NONE',  ( 1.999999999999999556, 0.000000000000000000, -0.7500000000000000000 ) ) ;
#27056 = PLANE ( 'NONE',  #13765 ) ;
#27057 = CARTESIAN_POINT ( 'NONE',  ( 1.040000000000001812, -1.891117961019736393, -34.36292081097834483 ) ) ;
#27058 = PLANE ( 'NONE',  #32750 ) ;
#27059 = CARTESIAN_POINT ( 'NONE',  ( 0.07098931954374571029, -0.5906890623668855644, 31.68904954958502884 ) ) ;
#27060 = DIRECTION ( 'NONE',  ( -1.000000000000000000, 0.000000000000000000, 0.000000000000000000 ) ) ;
#27061 = DIRECTION ( 'NONE',  ( 0.000000000000000000, 0.000000000000000000, 1.000000000000000000 ) ) ;
#27062 = VECTOR ( 'NONE', #10612, 1000.000000000000000 ) ;
#27063 = ORIENTED_EDGE ( 'NONE', *, *, #29689, .T. ) ;
#27064 = AXIS2_PLACEMENT_3D ( 'NONE', #4509, #15402, #26239 ) ;
#27065 = CARTESIAN_POINT ( 'NONE',  ( 0.3923936511923831194, 30.27116788629744804, 13.00174666746672969 ) ) ;
#27066 = DIRECTION ( 'NONE',  ( 2.631201909438060585E-14, -5.396010391056496978E-16, 1.000000000000000000 ) ) ;
#27067 = VERTEX_POINT ( 'NONE', #22659 ) ;
#27068 = ORIENTED_EDGE ( 'NONE', *, *, #30006, .F. ) ;
#27069 = ADVANCED_FACE ( 'NONE', ( #27802 ), #12226, .T. ) ;
#27070 = AXIS2_PLACEMENT_3D ( 'NONE', #3222, #11248, #21740 ) ;
#27071 = EDGE_CURVE ( 'NONE', #2032, #34687, #14299, .T. ) ;
#27072 = DIRECTION ( 'NONE',  ( 0.2149704402110236556, -0.9766205557100866574, -0.000000000000000000 ) ) ;
#27073 = ORIENTED_EDGE ( 'NONE', *, *, #23046, .F. ) ;
#27074 = EDGE_CURVE ( 'NONE', #5234, #5838, #1410, .T. ) ;
#27075 = CYLINDRICAL_SURFACE ( 'NONE', #11102, 2.524999999999999467 ) ;
#27076 = CIRCLE ( 'NONE', #2000, 7.999999999999979572 ) ;
#27077 = SURFACE_STYLE_FILL_AREA ( #32240 ) ;
#27078 = ITEM_DEFINED_TRANSFORMATION ( 'NONE', 'NONE', #21818,  #28566 ) ;
#27079 = DIRECTION ( 'NONE',  ( 0.000000000000000000, 0.000000000000000000, -1.000000000000000000 ) ) ;
#27080 = ORIENTED_EDGE ( 'NONE', *, *, #26356, .F. ) ;
#27081 = ORIENTED_EDGE ( 'NONE', *, *, #28887, .T. ) ;
#27082 = LINE ( 'NONE', #32245, #10598 ) ;
#27083 = CARTESIAN_POINT ( 'NONE',  ( 2.783084753007022627, 27.98916443103619045, -12.86217335695007868 ) ) ;
#27084 = AXIS2_PLACEMENT_3D ( 'NONE', #13069, #18239, #5030 ) ;
#27085 = DIRECTION ( 'NONE',  ( 1.232595164407830946E-32, 3.421138828918010427E-49, -1.000000000000000000 ) ) ;
#27086 = DIRECTION ( 'NONE',  ( -0.05413890858541756113, 0.9985334138511239299, 1.834276123671687812E-16 ) ) ;
#27087 = DIRECTION ( 'NONE',  ( 0.000000000000000000, 0.000000000000000000, -1.000000000000000000 ) ) ;
#27088 = ORIENTED_EDGE ( 'NONE', *, *, #32175, .F. ) ;
#27089 = PLANE ( 'NONE',  #10703 ) ;
#27090 = CARTESIAN_POINT ( 'NONE',  ( 3.235562306570555532E-30, -1.691831803474591833, -67.50000000000000000 ) ) ;
#27091 = LINE ( 'NONE', #24581, #20898 ) ;
#27092 = B_SPLINE_CURVE_WITH_KNOTS ( 'NONE', 3,
 ( #26401, #9854, #13243, #29256, #23559, #17897, #4851, #26750, #7171, #12898, #28900, #10032, #15216, #18592, #20890, #7519, #28727, #18072, #34953, #21423, #4496, #2362, #29067, #26221, #15559, #31735, #10569, #31566, #10208, #20722, #7344, #23384, #4665, #12721, #21061, #18237, #29431, #32086, #7001, #7705, #26056, #2021 ),
 .UNSPECIFIED., .F., .F.,
 ( 4, 2, 2, 2, 2, 2, 2, 2, 2, 2, 2, 2, 2, 2, 2, 2, 2, 2, 2, 2, 4 ),
 ( 6.768890431529877174E-19, 0.001137415812192693870, 0.002274831624385387305, 0.003412247436578080741, 0.003980955342674426592, 0.004549663248770772876, 0.005687079060963435954, 0.006824494873156099033, 0.007393202779252448786, 0.007961910685348797673, 0.009099326497541459016, 0.009668034403637809637, 0.01023674230973416026, 0.01137415812192686150, 0.01251157393411956274, 0.01364898974631226572, 0.01478640555850496696, 0.01535511346460131411, 0.01592382137069766473, 0.01706123718289036251, 0.01819865299508306028 ),
 .UNSPECIFIED. ) ;
#27093 = LINE ( 'NONE', #27620, #16354 ) ;
#27094 = VECTOR ( 'NONE', #9632, 1000.000000000000000 ) ;
#27095 = DIRECTION ( 'NONE',  ( -0.000000000000000000, -0.000000000000000000, -1.000000000000000000 ) ) ;
#27097 = CARTESIAN_POINT ( 'NONE',  ( -365.0000000000000000, -131.0000000000000000, 128.0000000000000000 ) ) ;
#27096 = CARTESIAN_POINT ( 'NONE',  ( 0.02407890056655781832, -29.68817180695682723, 9.232883799364120847 ) ) ;
#27098 = AXIS2_PLACEMENT_3D ( 'NONE', #23492, #7820, #13176 ) ;
#27099 = DIRECTION ( 'NONE',  ( 0.000000000000000000, 0.000000000000000000, 1.000000000000000000 ) ) ;
#27100 = ORIENTED_EDGE ( 'NONE', *, *, #29181, .F. ) ;
#27101 = CARTESIAN_POINT ( 'NONE',  ( -12.00000000000001066, 136.9999999999999716, -175.0000000000000284 ) ) ;
#27103 = CARTESIAN_POINT ( 'NONE',  ( 143.0000000000000568, 85.49999999999998579, 65.00000000000000000 ) ) ;
#27102 = CARTESIAN_POINT ( 'NONE',  ( -414.0000000000000568, -137.0000000000000000, 154.9999999999999716 ) ) ;
#27104 = EDGE_LOOP ( 'NONE', ( #27635, #22822, #26635, #32507 ) ) ;
#27105 = DIRECTION ( 'NONE',  ( 0.000000000000000000, -0.000000000000000000, -1.000000000000000000 ) ) ;
#27106 = VECTOR ( 'NONE', #10264, 1000.000000000000000 ) ;
#27107 = EDGE_LOOP ( 'NONE', ( #17401, #31210, #6067, #23255 ) ) ;
#27108 = EDGE_CURVE ( 'NONE', #1533, #32452, #25311, .T. ) ;
#27109 = ORIENTED_EDGE ( 'NONE', *, *, #30579, .T. ) ;
#27110 = FACE_OUTER_BOUND ( 'NONE', #33377, .T. ) ;
#27111 = ORIENTED_EDGE ( 'NONE', *, *, #33619, .T. ) ;
#27112 = VERTEX_POINT ( 'NONE', #6787 ) ;
#27113 = EDGE_CURVE ( 'NONE', #34772, #15054, #25125, .T. ) ;
#27114 = DIRECTION ( 'NONE',  ( 1.000000000000000000, -0.000000000000000000, 0.000000000000000000 ) ) ;
#27115 = AXIS2_PLACEMENT_3D ( 'NONE', #13275, #31773, #10417 ) ;
#27116 = TOROIDAL_SURFACE ( 'NONE', #18635, 30.47050528711512030, 8.000000000000000000 ) ;
#27117 = VECTOR ( 'NONE', #23169, 1000.000000000000000 ) ;
#27118 = FACE_OUTER_BOUND ( 'NONE', #5469, .T. ) ;
#27119 = FACE_BOUND ( 'NONE', #34957, .T. ) ;
#27120 = ORIENTED_EDGE ( 'NONE', *, *, #21253, .F. ) ;
#27121 = EDGE_CURVE ( 'NONE', #731, #3983, #28344, .T. ) ;
#27122 = VERTEX_POINT ( 'NONE', #759 ) ;
#27123 = CARTESIAN_POINT ( 'NONE',  ( 129.3530333899765594, -6.000000000000000000, -62.49999999999999289 ) ) ;
#27124 = CARTESIAN_POINT ( 'NONE',  ( -442.0000000000000000, -105.0000000000000142, 100.0000000000000000 ) ) ;
#27125 = EDGE_CURVE ( 'NONE', #32109, #6108, #12775, .T. ) ;
#27126 = CARTESIAN_POINT ( 'NONE',  ( 99.26191511054631178, -0.3844778738587134037, -12.49999999999999822 ) ) ;
#27127 = DIRECTION ( 'NONE',  ( 0.000000000000000000, 0.000000000000000000, 1.000000000000000000 ) ) ;
#27128 = ORIENTED_EDGE ( 'NONE', *, *, #7786, .F. ) ;
#27129 = VECTOR ( 'NONE', #17969, 1000.000000000000000 ) ;
#27130 = CARTESIAN_POINT ( 'NONE',  ( -5.823698994896891357, -1.505030548027689319, 0.000000000000000000 ) ) ;
#27131 = CARTESIAN_POINT ( 'NONE',  ( 30.69344702212033837, -10.82204614554913036, 68.31122994652405112 ) ) ;
#27132 = VERTEX_POINT ( 'NONE', #30662 ) ;
#27133 = LINE ( 'NONE', #10777, #309 ) ;
#27134 = CARTESIAN_POINT ( 'NONE',  ( 145.0000000000000568, 87.50000000000000000, 65.00000000000000000 ) ) ;
#27135 = CARTESIAN_POINT ( 'NONE',  ( 11.99999999999999645, -124.9999999999999432, -154.9999999999999716 ) ) ;
#27136 = DIRECTION ( 'NONE',  ( -0.000000000000000000, -0.000000000000000000, -1.000000000000000000 ) ) ;
#27137 = VERTEX_POINT ( 'NONE', #17513 ) ;
#27138 = AXIS2_PLACEMENT_3D ( 'NONE', #12561, #21084, #26422 ) ;
#27139 = CARTESIAN_POINT ( 'NONE',  ( -414.0000000000000568, 105.0000000000000000, -77.99999999999997158 ) ) ;
#27140 = VERTEX_POINT ( 'NONE', #7301 ) ;
#27141 = LINE ( 'NONE', #2927, #7434 ) ;
#27142 = DIRECTION ( 'NONE',  ( 0.000000000000000000, 0.5000000000000004441, -0.8660254037844382635 ) ) ;
#27143 = VECTOR ( 'NONE', #13679, 1000.000000000000114 ) ;
#27144 = AXIS2_PLACEMENT_3D ( 'NONE', #24844, #22012, #24477 ) ;
#27145 = ORIENTED_EDGE ( 'NONE', *, *, #11367, .T. ) ;
#27146 = APPLICATION_CONTEXT ( 'automotive_design' ) ;
#27147 = DIRECTION ( 'NONE',  ( 1.997825486195704824E-17, 0.000000000000000000, -1.000000000000000000 ) ) ;
#27148 = LINE ( 'NONE', #2761, #11475 ) ;
#27149 = ORIENTED_EDGE ( 'NONE', *, *, #14148, .F. ) ;
#27150 = AXIS2_PLACEMENT_3D ( 'NONE', #33921, #17924, #6682 ) ;
#27151 = ORIENTED_EDGE ( 'NONE', *, *, #12447, .F. ) ;
#27152 = LINE ( 'NONE', #2769, #8390 ) ;
#27153 = CARTESIAN_POINT ( 'NONE',  ( -99.92067881447050581, 0.6938560566811392549, 7.475525031754233218 ) ) ;
#27154 = ORIENTED_EDGE ( 'NONE', *, *, #25045, .T. ) ;
#27155 = ORIENTED_EDGE ( 'NONE', *, *, #28013, .F. ) ;
#27156 = CARTESIAN_POINT ( 'NONE',  ( -365.0000000000000000, -125.0000000000000284, 168.9999999999999716 ) ) ;
#27157 = EDGE_CURVE ( 'NONE', #10776, #22434, #12851, .T. ) ;
#27158 = CARTESIAN_POINT ( 'NONE',  ( 1.205771365940050410, 15.58845726811990495, 1.140844902514640588E-16 ) ) ;
#27159 = CIRCLE ( 'NONE', #20920, 7.999999999999979572 ) ;
#27160 = DIRECTION ( 'NONE',  ( -3.040835319149746090E-31, -1.000000000000000000, 0.000000000000000000 ) ) ;
#27161 = CARTESIAN_POINT ( 'NONE',  ( -45.00000000000000000, -4.831299144296466785, -15.81122994652406355 ) ) ;
#27162 = ADVANCED_FACE ( 'NONE', ( #18026 ), #26531, .T. ) ;
#27163 = ORIENTED_EDGE ( 'NONE', *, *, #19869, .F. ) ;
#27164 = EDGE_CURVE ( 'NONE', #16061, #25913, #4807, .T. ) ;
#27165 = ORIENTED_EDGE ( 'NONE', *, *, #18226, .T. ) ;
#27166 = DIRECTION ( 'NONE',  ( -1.000000000000000000, 0.000000000000000000, 1.232595164407831220E-32 ) ) ;
#27167 = DIRECTION ( 'NONE',  ( 1.000000000000000000, 0.000000000000000000, 0.000000000000000000 ) ) ;
#27168 = CARTESIAN_POINT ( 'NONE',  ( 22.89764159710611224, 13.56412600238610544, -87.50000000000000000 ) ) ;
#27169 = FACE_OUTER_BOUND ( 'NONE', #34823, .T. ) ;
#27170 = AXIS2_PLACEMENT_3D ( 'NONE', #10513, #27225, #24537 ) ;
#27171 = AXIS2_PLACEMENT_3D ( 'NONE', #19214, #24349, #29533 ) ;
#27172 = DIRECTION ( 'NONE',  ( 0.000000000000000000, 1.836970198721029441E-16, -1.000000000000000000 ) ) ;
#27173 = LINE ( 'NONE', #19008, #25631 ) ;
#27174 = CARTESIAN_POINT ( 'NONE',  ( -418.0000000000000000, -141.0000000000000000, -175.0000000000000000 ) ) ;
#27175 = DIRECTION ( 'NONE',  ( 0.000000000000000000, 2.309213040847544338E-50, 1.000000000000000000 ) ) ;
#27176 = ORIENTED_EDGE ( 'NONE', *, *, #33503, .T. ) ;
#27177 = CARTESIAN_POINT ( 'NONE',  ( -499.9999999999999432, 112.9999999999999574, -190.9999999999999716 ) ) ;
#27178 = CARTESIAN_POINT ( 'NONE',  ( -20.00000000000004619, -134.9999999999999716, -186.9999999999999716 ) ) ;
#27179 = EDGE_CURVE ( 'NONE', #11797, #7570, #26200, .T. ) ;
#27180 = VECTOR ( 'NONE', #34575, 1000.000000000000000 ) ;
#27181 = CARTESIAN_POINT ( 'NONE',  ( 0.02815752724870344489, 1.322857909648822439, -13.50000000000000000 ) ) ;
#27182 = ORIENTED_EDGE ( 'NONE', *, *, #2074, .F. ) ;
#27183 = CARTESIAN_POINT ( 'NONE',  ( -12.00000000000001066, -32.99999999999997158, 154.9999999999999716 ) ) ;
#27184 = ORIENTED_EDGE ( 'NONE', *, *, #25091, .F. ) ;
#27185 = LINE ( 'NONE', #21151, #31928 ) ;
#27186 = EDGE_CURVE ( 'NONE', #34878, #23180, #24101, .T. ) ;
#27187 = CIRCLE ( 'NONE', #25486, 3.999999999999976019 ) ;
#27188 = CARTESIAN_POINT ( 'NONE',  ( -5.210000000000000853, 0.000000000000000000, 0.000000000000000000 ) ) ;
#27189 = EDGE_CURVE ( 'NONE', #23058, #20852, #2153, .T. ) ;
#27190 = CIRCLE ( 'NONE', #28347, 4.000000000000003553 ) ;
#27191 = EDGE_LOOP ( 'NONE', ( #25446, #34510, #15029, #19783, #2325, #27906 ) ) ;
#27192 = FACE_OUTER_BOUND ( 'NONE', #32586, .T. ) ;
#27193 = CYLINDRICAL_SURFACE ( 'NONE', #34377, 2.524999999999999467 ) ;
#27194 = CARTESIAN_POINT ( 'NONE',  ( -445.9999999999999432, -125.0000000000000000, 187.0000000000000000 ) ) ;
#27195 = EDGE_CURVE ( 'NONE', #26390, #22784, #15703, .T. ) ;
#27196 = ORIENTED_EDGE ( 'NONE', *, *, #28997, .T. ) ;
#27197 = AXIS2_PLACEMENT_3D ( 'NONE', #9918, #25761, #9404 ) ;
#27198 = ORIENTED_EDGE ( 'NONE', *, *, #3593, .F. ) ;
#27199 = CARTESIAN_POINT ( 'NONE',  ( 845.0436366819767500, 1086.835633900147286, 1753.598338701303419 ) ) ;
#27200 = DIRECTION ( 'NONE',  ( 0.000000000000000000, 0.000000000000000000, 1.000000000000000000 ) ) ;
#27201 = ORIENTED_EDGE ( 'NONE', *, *, #7415, .T. ) ;
#27202 = CARTESIAN_POINT ( 'NONE',  ( -499.9999999999999432, 136.9999999999999432, 187.0000000000000000 ) ) ;
#27203 = AXIS2_PLACEMENT_3D ( 'NONE', #26473, #23811, #31986 ) ;
#27204 = CYLINDRICAL_SURFACE ( 'NONE', #34032, 3.999999999999982681 ) ;
#27205 = DIRECTION ( 'NONE',  ( -0.000000000000000000, -0.000000000000000000, 1.000000000000000000 ) ) ;
#27206 = CARTESIAN_POINT ( 'NONE',  ( -101.8712807483899354, -4.059672565113375597, 6.310142985817157602 ) ) ;
#27207 = EDGE_CURVE ( 'NONE', #18201, #4999, #21298, .T. ) ;
#27208 = ORIENTED_EDGE ( 'NONE', *, *, #14829, .F. ) ;
#27209 = EDGE_CURVE ( 'NONE', #707, #16352, #26358, .T. ) ;
#27210 = ORIENTED_EDGE ( 'NONE', *, *, #10587, .F. ) ;
#27211 = VERTEX_POINT ( 'NONE', #20676 ) ;
#27212 = DIRECTION ( 'NONE',  ( 0.000000000000000000, 0.000000000000000000, -1.000000000000000000 ) ) ;
#27213 = LINE ( 'NONE', #11375, #96 ) ;
#27214 = DIRECTION ( 'NONE',  ( 1.000000000000000000, 0.000000000000000000, 0.000000000000000000 ) ) ;
#27215 = CIRCLE ( 'NONE', #11893, 30.47050528711512030 ) ;
#27216 = VERTEX_POINT ( 'NONE', #4984 ) ;
#27217 = ORIENTED_EDGE ( 'NONE', *, *, #16737, .T. ) ;
#27218 = CARTESIAN_POINT ( 'NONE',  ( -442.0000000000000000, -105.0000000000000142, 187.0000000000000000 ) ) ;
#27219 = ORIENTED_EDGE ( 'NONE', *, *, #24146, .T. ) ;
#27220 = CARTESIAN_POINT ( 'NONE',  ( 2.765921099433443331, -3.506335382740311868, -30.89238256715869468 ) ) ;
#27221 = CARTESIAN_POINT ( 'NONE',  ( -355.0000000000000000, -131.0000000000000000, 113.9999999999999858 ) ) ;
#27222 = VERTEX_POINT ( 'NONE', #18371 ) ;
#27223 = AXIS2_PLACEMENT_3D ( 'NONE', #18569, #21212, #28400 ) ;
#27224 = VERTEX_POINT ( 'NONE', #9814 ) ;
#27225 = DIRECTION ( 'NONE',  ( -1.000000000000000000, -0.000000000000000000, 0.000000000000000000 ) ) ;
#27226 = DIRECTION ( 'NONE',  ( -0.4198891015602635446, -0.9075754196709575616, -1.667188999027280528E-16 ) ) ;
#27227 = EDGE_LOOP ( 'NONE', ( #18296, #30599 ) ) ;
#27228 = DIRECTION ( 'NONE',  ( 1.000000000000000000, 0.000000000000000000, 0.000000000000000000 ) ) ;
#27229 = DIRECTION ( 'NONE',  ( 0.000000000000000000, 0.000000000000000000, -1.000000000000000000 ) ) ;
#27230 = CARTESIAN_POINT ( 'NONE',  ( 0.000000000000000000, 0.000000000000000000, 87.50000000000000000 ) ) ;
#27231 = TOROIDAL_SURFACE ( 'NONE', #6206, 30.47050528711512030, 8.000000000000000000 ) ;
#27232 = EDGE_CURVE ( 'NONE', #8590, #4316, #29389, .T. ) ;
#27233 = CARTESIAN_POINT ( 'NONE',  ( 129.3530333899765594, 6.000000000000000000, -57.49999999999999289 ) ) ;
#27234 = EDGE_CURVE ( 'NONE', #16703, #18132, #20844, .T. ) ;
#27235 = CARTESIAN_POINT ( 'NONE',  ( -20.00000000000001776, -113.0000000000000000, 194.9999999999999716 ) ) ;
#27236 = CARTESIAN_POINT ( 'NONE',  ( -449.9999999999999432, -105.0000000000000142, -174.9999999999999432 ) ) ;
#27237 = DIRECTION ( 'NONE',  ( 0.000000000000000000, 0.000000000000000000, 1.000000000000000000 ) ) ;
#27238 = AXIS2_PLACEMENT_3D ( 'NONE', #11651, #9663, #20360 ) ;
#27239 = EDGE_LOOP ( 'NONE', ( #31997, #31069, #34110, #5596 ) ) ;
#27240 = CARTESIAN_POINT ( 'NONE',  ( 5.021133111224473033, 6.201984591278720593, -87.50000000000000000 ) ) ;
#27241 = EDGE_CURVE ( 'NONE', #30030, #32472, #11798, .T. ) ;
#27242 = ORIENTED_EDGE ( 'NONE', *, *, #30577, .F. ) ;
#27243 = ORIENTED_EDGE ( 'NONE', *, *, #26098, .F. ) ;
#27244 = AXIS2_PLACEMENT_3D ( 'NONE', #8028, #22094, #16773 ) ;
#27245 = CARTESIAN_POINT ( 'NONE',  ( -418.0000000000000000, -105.0000000000000142, 107.9999999999999858 ) ) ;
#27246 = ORIENTED_EDGE ( 'NONE', *, *, #20276, .F. ) ;
#27247 = B_SPLINE_CURVE_WITH_KNOTS ( 'NONE', 3,
 ( #11463, #17173, #8434, #22320, #3611, #14141 ),
 .UNSPECIFIED., .F., .F.,
 ( 4, 2, 4 ),
 ( 2.078540822438843793E-07, 0.001873406157010511566, 0.003746604459938779504 ),
 .UNSPECIFIED. ) ;
#27248 = CARTESIAN_POINT ( 'NONE',  ( 36.10877985260813716, 11.38239727801118306, 49.43553178847298568 ) ) ;
#27249 = CARTESIAN_POINT ( 'NONE',  ( -2.216215597024039141, -32.46987467335850397, -36.68877005347593467 ) ) ;
#27250 = AXIS2_PLACEMENT_3D ( 'NONE', #23370, #1829, #15028 ) ;
#27251 = CONTEXT_DEPENDENT_SHAPE_REPRESENTATION ( #587, #16156 ) ;
#27253 = CARTESIAN_POINT ( 'NONE',  ( -365.0000000000000000, 130.9999999999999716, 109.9999999999999858 ) ) ;
#27252 = LINE ( 'NONE', #2859, #17331 ) ;
#27254 = ORIENTED_EDGE ( 'NONE', *, *, #17299, .F. ) ;
#27255 = ORIENTED_EDGE ( 'NONE', *, *, #11174, .T. ) ;
#27256 = DIRECTION ( 'NONE',  ( 0.000000000000000000, 1.000000000000000000, 0.000000000000000000 ) ) ;
#27258 = EDGE_CURVE ( 'NONE', #8335, #7441, #10526, .T. ) ;
#27257 = CARTESIAN_POINT ( 'NONE',  ( -418.0000000000000000, 104.9999999999999858, 155.0000000000000000 ) ) ;
#27259 = DIRECTION ( 'NONE',  ( -0.000000000000000000, -0.000000000000000000, 1.000000000000000000 ) ) ;
#27260 = DIRECTION ( 'NONE',  ( 1.000000000000000000, 3.469446951953834515E-18, 0.000000000000000000 ) ) ;
#27261 = CARTESIAN_POINT ( 'NONE',  ( 145.0000000000000568, -175.8248315648716016, -46.05325008164006562 ) ) ;
#27262 = VERTEX_POINT ( 'NONE', #12330 ) ;
#27263 = DIRECTION ( 'NONE',  ( 0.9985334138511239299, -0.05413890858541753337, 0.000000000000000000 ) ) ;
#27264 = DIRECTION ( 'NONE',  ( 0.000000000000000000, 1.836970198721029441E-16, -1.000000000000000000 ) ) ;
#27265 = CARTESIAN_POINT ( 'NONE',  ( -70.00000000000000000, 75.55999999999990280, -172.9900000000000091 ) ) ;
#27266 = AXIS2_PLACEMENT_3D ( 'NONE', #13400, #8037, #24233 ) ;
#27267 = DIRECTION ( 'NONE',  ( 0.000000000000000000, 0.000000000000000000, -1.000000000000000000 ) ) ;
#27268 = EDGE_CURVE ( 'NONE', #33289, #20006, #15170, .T. ) ;
#27269 = CARTESIAN_POINT ( 'NONE',  ( 2.789999999999999147, -13.59935610937951900, -28.90010281771846223 ) ) ;
#27270 = EDGE_CURVE ( 'NONE', #11365, #18155, #21197, .T. ) ;
#27272 = CARTESIAN_POINT ( 'NONE',  ( 0.000000000000000000, -32.54542015209055705, 49.43553178847298568 ) ) ;
#27271 = PLANE ( 'NONE',  #20718 ) ;
#27273 = ADVANCED_FACE ( 'NONE', ( #31349 ), #6956, .F. ) ;
#27274 = PLANE ( 'NONE',  #8763 ) ;
#27275 = VERTEX_POINT ( 'NONE', #26011 ) ;
#27276 = FACE_OUTER_BOUND ( 'NONE', #15616, .T. ) ;
#27277 = CARTESIAN_POINT ( 'NONE',  ( 2.606461820648786620, -32.24848086092536903, -1.209851624881845611 ) ) ;
#27278 = AXIS2_PLACEMENT_3D ( 'NONE', #18563, #10177, #26183 ) ;
#27279 = ORIENTED_EDGE ( 'NONE', *, *, #20060, .T. ) ;
#27280 = DIRECTION ( 'NONE',  ( 0.3701381553399132329, 0.9289767198167918627, -0.000000000000000000 ) ) ;
#27281 = ORIENTED_EDGE ( 'NONE', *, *, #15886, .F. ) ;
#27282 = VERTEX_POINT ( 'NONE', #22079 ) ;
#27283 = DIRECTION ( 'NONE',  ( 0.000000000000000000, 5.053935297177146739E-49, 1.000000000000000000 ) ) ;
#27284 = ORIENTED_EDGE ( 'NONE', *, *, #33236, .T. ) ;
#27285 = ORIENTED_EDGE ( 'NONE', *, *, #19546, .T. ) ;
#27286 = CARTESIAN_POINT ( 'NONE',  ( -349.0000000000000000, -125.0000000000000284, 181.0000000000000000 ) ) ;
#27287 = CONTEXT_DEPENDENT_SHAPE_REPRESENTATION ( #31715, #31918 ) ;
#27288 = DIRECTION ( 'NONE',  ( -1.000000000000000000, 0.000000000000000000, 0.000000000000000000 ) ) ;
#27289 = ORIENTED_EDGE ( 'NONE', *, *, #11004, .F. ) ;
#27290 = ORIENTED_EDGE ( 'NONE', *, *, #25497, .F. ) ;
#27291 = LINE ( 'NONE', #22143, #3190 ) ;
#27292 = DIRECTION ( 'NONE',  ( -0.000000000000000000, -0.000000000000000000, -1.000000000000000000 ) ) ;
#27293 = DIRECTION ( 'NONE',  ( 0.000000000000000000, 1.000000000000000000, -3.374343856708137958E-53 ) ) ;
#27294 = DIRECTION ( 'NONE',  ( 0.000000000000000000, 1.000000000000000000, 1.224646799147353207E-16 ) ) ;
#27295 = ORIENTED_EDGE ( 'NONE', *, *, #34705, .T. ) ;
#27296 = AXIS2_PLACEMENT_3D ( 'NONE', #33252, #9408, #1212 ) ;
#27297 = DIRECTION ( 'NONE',  ( 0.000000000000000000, -1.836970198721029934E-16, 1.000000000000000000 ) ) ;
#27298 = CARTESIAN_POINT ( 'NONE',  ( -29.34345171400087793, 14.07715221144534823, 68.31122994652405112 ) ) ;
#27299 = ORIENTED_EDGE ( 'NONE', *, *, #20071, .F. ) ;
#27300 = EDGE_CURVE ( 'NONE', #25547, #27889, #8541, .T. ) ;
#27301 = DIRECTION ( 'NONE',  ( 0.000000000000000000, 0.000000000000000000, -1.000000000000000000 ) ) ;
#27302 = LINE ( 'NONE', #3101, #19477 ) ;
#27303 = ADVANCED_FACE ( 'NONE', ( #29562 ), #2314, .T. ) ;
#27304 = LINE ( 'NONE', #14863, #20083 ) ;
#27305 = CARTESIAN_POINT ( 'NONE',  ( 0.000000000000000000, 9.869977788041397915, -30.37666815053925973 ) ) ;
#27306 = ORIENTED_EDGE ( 'NONE', *, *, #1342, .T. ) ;
#27307 = ADVANCED_FACE ( 'NONE', ( #32392 ), #371, .T. ) ;
#27308 = VECTOR ( 'NONE', #4043, 1000.000000000000000 ) ;
#27309 = CARTESIAN_POINT ( 'NONE',  ( -1.307386931792819285, 37.83772838912469894, 68.31122994652405112 ) ) ;
#27310 = ORIENTED_EDGE ( 'NONE', *, *, #33489, .F. ) ;
#27311 = EDGE_CURVE ( 'NONE', #31132, #29028, #8012, .T. ) ;
#27313 = CARTESIAN_POINT ( 'NONE',  ( 0.1859802831645324950, 21.49213631816453329, -24.08729967255597870 ) ) ;
#27312 = DIRECTION ( 'NONE',  ( -1.000000000000000000, -0.000000000000000000, -0.000000000000000000 ) ) ;
#27314 = CARTESIAN_POINT ( 'NONE',  ( -3.250000000000000000, -5.838643359331793015, -0.7500000000000000000 ) ) ;
#27315 = ORIENTED_EDGE ( 'NONE', *, *, #2961, .T. ) ;
#27316 = DIRECTION ( 'NONE',  ( -0.000000000000000000, 1.000000000000000000, -0.000000000000000000 ) ) ;
#27317 = CARTESIAN_POINT ( 'NONE',  ( -35.00000000000000000, 0.5883377166429079042, -15.81122994652406355 ) ) ;
#27318 = AXIS2_PLACEMENT_3D ( 'NONE', #258, #16295, #8084 ) ;
#27319 = EDGE_CURVE ( 'NONE', #27517, #16381, #16753, .T. ) ;
#27320 = EDGE_LOOP ( 'NONE', ( #13358, #33504, #17827, #23743 ) ) ;
#27321 = AXIS2_PLACEMENT_3D ( 'NONE', #5217, #26946, #7720 ) ;
#27322 = VERTEX_POINT ( 'NONE', #24733 ) ;
#27323 = ORIENTED_EDGE ( 'NONE', *, *, #2367, .T. ) ;
#27324 = DIRECTION ( 'NONE',  ( -0.000000000000000000, -0.000000000000000000, 1.000000000000000000 ) ) ;
#27325 = CARTESIAN_POINT ( 'NONE',  ( -110.0788626153423451, 0.6978363313042807992, 7.475210363867073937 ) ) ;
#27326 = ORIENTED_EDGE ( 'NONE', *, *, #20341, .F. ) ;
#27327 = ORIENTED_EDGE ( 'NONE', *, *, #32984, .F. ) ;
#27328 = DIRECTION ( 'NONE',  ( -1.000000000000000000, -3.469446951953834515E-18, 0.000000000000000000 ) ) ;
#27329 = DIRECTION ( 'NONE',  ( -1.000000000000000000, 0.000000000000000000, -1.300283923313630633E-47 ) ) ;
#27330 = CARTESIAN_POINT ( 'NONE',  ( 1.749999999999999778, -24.90160365674851306, -23.75493189058367349 ) ) ;
#27331 = VECTOR ( 'NONE', #29759, 1000.000000000000000 ) ;
#27332 = FACE_OUTER_BOUND ( 'NONE', #23206, .T. ) ;
#27333 = ORIENTED_EDGE ( 'NONE', *, *, #9872, .F. ) ;
#27334 = ORIENTED_EDGE ( 'NONE', *, *, #5797, .F. ) ;
#27335 = AXIS2_PLACEMENT_3D ( 'NONE', #4413, #2111, #6911 ) ;
#27336 = CARTESIAN_POINT ( 'NONE',  ( -20.00000000000007461, 140.9999999999999716, -162.9999999999999716 ) ) ;
#27337 = DIRECTION ( 'NONE',  ( 1.000000000000000000, -0.000000000000000000, -0.000000000000000000 ) ) ;
#27338 = AXIS2_PLACEMENT_3D ( 'NONE', #28206, #11313, #6295 ) ;
#27339 = CARTESIAN_POINT ( 'NONE',  ( 2.789999999999999147, 27.60935207499570154, -12.89090262359623118 ) ) ;
#27340 = DIRECTION ( 'NONE',  ( 0.9766205557100871015, 0.2149704402110223789, 0.000000000000000000 ) ) ;
#27341 = FACE_OUTER_BOUND ( 'NONE', #1307, .T. ) ;
#27342 = FACE_OUTER_BOUND ( 'NONE', #6043, .T. ) ;
#27343 = CARTESIAN_POINT ( 'NONE',  ( 0.000000000000000000, 3.524919873834583163E-15, 68.31122994652405112 ) ) ;
#27344 = VERTEX_POINT ( 'NONE', #29916 ) ;
#27345 = VECTOR ( 'NONE', #3270, 1000.000000000000000 ) ;
#27346 = CYLINDRICAL_SURFACE ( 'NONE', #20831, 16.19999999999999574 ) ;
#27347 = CYLINDRICAL_SURFACE ( 'NONE', #4627, 7.999999999999979572 ) ;
#27348 = VECTOR ( 'NONE', #22843, 1000.000000000000000 ) ;
#27349 = DIRECTION ( 'NONE',  ( 0.000000000000000000, 0.000000000000000000, 1.000000000000000000 ) ) ;
#27350 = ORIENTED_EDGE ( 'NONE', *, *, #27232, .T. ) ;
#27351 = APPLICATION_CONTEXT ( 'automotive_design' ) ;
#27352 = DIRECTION ( 'NONE',  ( 0.000000000000000000, 1.000000000000000000, -5.145227585319922065E-49 ) ) ;
#27353 = ORIENTED_EDGE ( 'NONE', *, *, #25399, .F. ) ;
#27354 = ADVANCED_FACE ( 'NONE', ( #24383 ), #19416, .T. ) ;
#27355 = CARTESIAN_POINT ( 'NONE',  ( 2.789999999999999147, 11.30192140231231868, 28.29696565125074414 ) ) ;
#27356 = CARTESIAN_POINT ( 'NONE',  ( 2.790000000000000036, 30.15879770317926756, 5.529954278609506169 ) ) ;
#27357 = ADVANCED_FACE ( 'NONE', ( #13894 ), #13714, .F. ) ;
#27359 = VERTEX_POINT ( 'NONE', #21896 ) ;
#27358 = VECTOR ( 'NONE', #10689, 1000.000000000000000 ) ;
#27360 = EDGE_CURVE ( 'NONE', #22752, #28240, #8228, .T. ) ;
#27361 = EDGE_CURVE ( 'NONE', #31492, #18500, #28133, .T. ) ;
#27362 = AXIS2_PLACEMENT_3D ( 'NONE', #2673, #29561, #11045 ) ;
#27363 = LINE ( 'NONE', #13848, #21702 ) ;
#27364 = CIRCLE ( 'NONE', #12050, 32.54542015209055705 ) ;
#27365 = DIRECTION ( 'NONE',  ( -1.000000000000000000, -0.000000000000000000, -0.000000000000000000 ) ) ;
#27366 = DIRECTION ( 'NONE',  ( 0.9985334138511239299, 0.05413890858541774848, 0.000000000000000000 ) ) ;
#27367 = ORIENTED_EDGE ( 'NONE', *, *, #29030, .F. ) ;
#27368 = ORIENTED_EDGE ( 'NONE', *, *, #31697, .T. ) ;
#27369 = DIRECTION ( 'NONE',  ( 0.1063910735369155841, -0.9943243633099125844, -3.335902418025060287E-15 ) ) ;
#27370 = DIRECTION ( 'NONE',  ( -0.5155538571770218459, 0.8568571761675891629, 0.000000000000000000 ) ) ;
#27371 = ORIENTED_EDGE ( 'NONE', *, *, #10923, .T. ) ;
#27372 = DIRECTION ( 'NONE',  ( -0.000000000000000000, -1.310824597558155437E-49, -1.000000000000000000 ) ) ;
#27373 = EDGE_CURVE ( 'NONE', #20130, #16547, #10, .T. ) ;
#27374 = VECTOR ( 'NONE', #14049, 1000.000000000000000 ) ;
#27375 = FACE_OUTER_BOUND ( 'NONE', #3086, .T. ) ;
#27376 = CARTESIAN_POINT ( 'NONE',  ( 2.606461808080008158, 14.82544181993015009, -28.66416816974122383 ) ) ;
#27377 = CARTESIAN_POINT ( 'NONE',  ( -104.6476413610425169, -5.105803102660849468, 5.493756281618517257 ) ) ;
#27378 = CONTEXT_DEPENDENT_SHAPE_REPRESENTATION ( #30591, #34197 ) ;
#27379 = ORIENTED_EDGE ( 'NONE', *, *, #30049, .T. ) ;
#27380 = ORIENTED_EDGE ( 'NONE', *, *, #27386, .F. ) ;
#27381 = ORIENTED_EDGE ( 'NONE', *, *, #12105, .F. ) ;
#27382 = PRODUCT ( 'short pitch roller chain wheel_s_iso_Chain wheel ISO - 25Z 05B-1 --25SA20.0S1', 'short pitch roller chain wheel_s_iso_Chain wheel ISO - 25Z 05B-1 --25SA20.0S1', '', ( #8910 ) ) ;
#27383 = FACE_OUTER_BOUND ( 'NONE', #3227, .T. ) ;
#27384 = DIRECTION ( 'NONE',  ( 0.000000000000000000, 0.000000000000000000, -1.000000000000000000 ) ) ;
#27385 = VECTOR ( 'NONE', #7609, 1000.000000000000000 ) ;
#27386 = EDGE_CURVE ( 'NONE', #2370, #8469, #17365, .T. ) ;
#27387 = DIRECTION ( 'NONE',  ( 0.000000000000000000, 0.000000000000000000, 1.000000000000000000 ) ) ;
#27388 = ADVANCED_FACE ( 'NONE', ( #5860 ), #29735, .F. ) ;
#27390 = ORIENTED_EDGE ( 'NONE', *, *, #19548, .T. ) ;
#27389 = CIRCLE ( 'NONE', #28516, 34.41491905851385269 ) ;
#27391 = ORIENTED_EDGE ( 'NONE', *, *, #32617, .T. ) ;
#27392 = FACE_OUTER_BOUND ( 'NONE', #31744, .T. ) ;
#27393 = AXIS2_PLACEMENT_3D ( 'NONE', #21339, #29523, #5115 ) ;
#27394 = ORIENTED_EDGE ( 'NONE', *, *, #4299, .F. ) ;
#27395 = VECTOR ( 'NONE', #32179, 1000.000000000000000 ) ;
#27396 = CARTESIAN_POINT ( 'NONE',  ( 2.765921099433442443, 31.00221527374952046, -2.344426712874310148 ) ) ;
#27397 = FACE_OUTER_BOUND ( 'NONE', #22722, .T. ) ;
#27398 = VERTEX_POINT ( 'NONE', #5336 ) ;
#27399 = ORIENTED_EDGE ( 'NONE', *, *, #31324, .F. ) ;
#27400 = DIRECTION ( 'NONE',  ( 0.000000000000000000, 0.000000000000000000, 1.000000000000000000 ) ) ;
#27401 = PLANE ( 'NONE',  #22908 ) ;
#27402 = ORIENTED_EDGE ( 'NONE', *, *, #19114, .T. ) ;
#27403 = FACE_OUTER_BOUND ( 'NONE', #19125, .T. ) ;
#27404 = CARTESIAN_POINT ( 'NONE',  ( 10.17231796313409298, 8.346743312457579833, -77.50000000000000000 ) ) ;
#27405 = DIRECTION ( 'NONE',  ( 0.000000000000000000, 1.000000000000000000, 5.145227585319922065E-49 ) ) ;
#27406 = DIRECTION ( 'NONE',  ( 0.000000000000000000, 1.000000000000000000, 5.053935297177146739E-49 ) ) ;
#27407 = EDGE_CURVE ( 'NONE', #2604, #23345, #29832, .T. ) ;
#27408 = EDGE_CURVE ( 'NONE', #25387, #29898, #30420, .T. ) ;
#27409 =( REPRESENTATION_RELATIONSHIP ('NONE','NONE', #23037, #28231 ) REPRESENTATION_RELATIONSHIP_WITH_TRANSFORMATION ( #22096 )SHAPE_REPRESENTATION_RELATIONSHIP( ) );
#27410 = DIRECTION ( 'NONE',  ( -1.000000000000000000, -3.040835319149746528E-31, -1.232595164407830946E-32 ) ) ;
#27411 = DIRECTION ( 'NONE',  ( 0.000000000000000000, 0.000000000000000000, 1.000000000000000000 ) ) ;
#27412 = DIRECTION ( 'NONE',  ( 0.000000000000000000, 1.310824597558155437E-49, 1.000000000000000000 ) ) ;
#27413 = EDGE_CURVE ( 'NONE', #19034, #8292, #21382, .T. ) ;
#27414 = ORIENTED_EDGE ( 'NONE', *, *, #24211, .F. ) ;
#27415 = CIRCLE ( 'NONE', #12095, 7.999999999999979572 ) ;
#27416 = VECTOR ( 'NONE', #3108, 1000.000000000000000 ) ;
#27417 = FACE_OUTER_BOUND ( 'NONE', #1078, .T. ) ;
#27418 = DIRECTION ( 'NONE',  ( 0.1063910735368947813, -0.9943243633099144718, -3.335902418024520312E-15 ) ) ;
#27419 = PRESENTATION_LAYER_ASSIGNMENT (  '', '', ( #22882 ) ) ;
#27420 = VERTEX_POINT ( 'NONE', #13374 ) ;
#27421 = ORIENTED_EDGE ( 'NONE', *, *, #34960, .F. ) ;
#27422 = CYLINDRICAL_SURFACE ( 'NONE', #15380, 16.19999999999999929 ) ;
#27423 = ORIENTED_EDGE ( 'NONE', *, *, #34788, .T. ) ;
#27424 = DIRECTION ( 'NONE',  ( 0.000000000000000000, 0.000000000000000000, -1.000000000000000000 ) ) ;
#27425 = CARTESIAN_POINT ( 'NONE',  ( 19.99999999999998934, 75.55999999999990280, -172.9900000000000091 ) ) ;
#27426 = EDGE_CURVE ( 'NONE', #26369, #9416, #24207, .T. ) ;
#27427 = ADVANCED_FACE ( 'NONE', ( #14436 ), #14073, .F. ) ;
#27428 = ITEM_DEFINED_TRANSFORMATION ( 'NONE', 'NONE', #29195,  #28566 ) ;
#27429 = EDGE_CURVE ( 'NONE', #24623, #4681, #23583, .T. ) ;
#27431 = PLANE ( 'NONE',  #34593 ) ;
#27430 = DIRECTION ( 'NONE',  ( 0.000000000000000000, -1.000000000000000000, -2.465190328815662439E-32 ) ) ;
#27432 = ORIENTED_EDGE ( 'NONE', *, *, #9605, .T. ) ;
#27433 = ORIENTED_EDGE ( 'NONE', *, *, #2681, .T. ) ;
#27434 = DIRECTION ( 'NONE',  ( -0.5611870653623824978, -0.8276889981568904542, -1.520440023423473517E-16 ) ) ;
#27435 = CARTESIAN_POINT ( 'NONE',  ( 2.789999999999999147, -23.41952779159748133, -19.49300927180569687 ) ) ;
#27436 = EDGE_CURVE ( 'NONE', #29137, #11246, #22432, .T. ) ;
#27437 = LINE ( 'NONE', #13571, #5648 ) ;
#27438 = DIRECTION ( 'NONE',  ( 0.000000000000000000, 0.000000000000000000, -1.000000000000000000 ) ) ;
#27439 = PLANE ( 'NONE',  #16014 ) ;
#27440 = PRODUCT_DEFINITION_CONTEXT ( 'detailed design', #1679, 'design' ) ;
#27441 = ORIENTED_EDGE ( 'NONE', *, *, #18464, .T. ) ;
#27442 = DIRECTION ( 'NONE',  ( -0.000000000000000000, -0.000000000000000000, 1.000000000000000000 ) ) ;
#27443 = PLANE ( 'NONE',  #25352 ) ;
#27444 = DIRECTION ( 'NONE',  ( 0.000000000000000000, 1.131431318426415506E-52, 1.000000000000000000 ) ) ;
#27445 = ADVANCED_FACE ( 'NONE', ( #3730 ), #23035, .T. ) ;
#27446 = VECTOR ( 'NONE', #23645, 1000.000000000000000 ) ;
#27447 = TOROIDAL_SURFACE ( 'NONE', #22317, 30.47050528711511674, 8.000000000000000000 ) ;
#27448 = AXIS2_PLACEMENT_3D ( 'NONE', #10947, #27489, #16657 ) ;
#27449 = CARTESIAN_POINT ( 'NONE',  ( 0.07098932983996933399, -11.11630839801572890, -29.68118041677939445 ) ) ;
#27450 = FILL_AREA_STYLE_COLOUR ( '', #30892 ) ;
#27451 = LINE ( 'NONE', #26743, #10984 ) ;
#27453 = DIRECTION ( 'NONE',  ( -1.000000000000000000, 0.000000000000000000, 0.000000000000000000 ) ) ;
#27452 = CARTESIAN_POINT ( 'NONE',  ( -42.55956070192387841, -20.15143121711728469, 0.000000000000000000 ) ) ;
#27454 = ADVANCED_FACE ( 'NONE', ( #27587 ), #22613, .T. ) ;
#27455 = LINE ( 'NONE', #11094, #17309 ) ;
#27456 = VERTEX_POINT ( 'NONE', #30789 ) ;
#27457 = CARTESIAN_POINT ( 'NONE',  ( 5.021133111224162171, -21.54630831098063837, -67.50000000000000000 ) ) ;
#27458 = LINE ( 'NONE', #2717, #4334 ) ;
#27459 = CIRCLE ( 'NONE', #12131, 2.525000000000000799 ) ;
#27460 = EDGE_LOOP ( 'NONE', ( #17412, #346, #33345, #32108 ) ) ;
#27461 =( NAMED_UNIT ( * ) SI_UNIT ( $, .STERADIAN. ) SOLID_ANGLE_UNIT ( ) );
#27462 = ORIENTED_EDGE ( 'NONE', *, *, #1689, .T. ) ;
#27463 = AXIS2_PLACEMENT_3D ( 'NONE', #33415, #13675, #27895 ) ;
#27464 = CIRCLE ( 'NONE', #33724, 1.999999999999999112 ) ;
#27465 = ORIENTED_EDGE ( 'NONE', *, *, #4798, .T. ) ;
#27466 = DIRECTION ( 'NONE',  ( 0.000000000000000000, 1.000000000000000000, 5.145227585319922065E-49 ) ) ;
#27467 = ORIENTED_EDGE ( 'NONE', *, *, #28121, .T. ) ;
#27468 = ORIENTED_EDGE ( 'NONE', *, *, #4798, .F. ) ;
#27469 = LINE ( 'NONE', #24963, #30970 ) ;
#27470 = EDGE_CURVE ( 'NONE', #30793, #10340, #26420, .T. ) ;
#27471 = CONTEXT_DEPENDENT_SHAPE_REPRESENTATION ( #28309, #4621 ) ;
#27472 = EDGE_CURVE ( 'NONE', #9737, #20411, #16933, .T. ) ;
#27473 = CARTESIAN_POINT ( 'NONE',  ( -410.0000000000000568, -125.0000000000000000, 107.9999999999999858 ) ) ;
#27474 = CARTESIAN_POINT ( 'NONE',  ( 11.99999999999999645, -145.0000000000000000, -186.9999999999999716 ) ) ;
#27475 = EDGE_LOOP ( 'NONE', ( #1060, #23143, #26145, #9422, #26691, #5660, #9775, #29575, #29303, #28699, #18574, #22525, #7944, #24422, #3215, #15461, #11209, #1502, #21547, #9301, #12663, #22033, #16682, #28295, #14715, #9430, #21815, #12776, #23947, #16481, #11500, #13706, #27680, #23599, #30561, #32150, #34269, #14996, #6546, #25334, #19599, #21117, #27801, #29875, #15000, #25363, #23245, #29856, #32117, #31274, #29311, #416, #16111, #16825, #2557, #1352, #19814 ) ) ;
#27476 = VERTEX_POINT ( 'NONE', #25614 ) ;
#27477 = DIRECTION ( 'NONE',  ( 3.697785493223492838E-32, 1.934419779023891545E-16, -1.000000000000000000 ) ) ;
#27478 = CARTESIAN_POINT ( 'NONE',  ( 0.000000000000000000, 0.000000000000000000, 20.00000000000000000 ) ) ;
#27479 = CARTESIAN_POINT ( 'NONE',  ( 100.6811048285187269, -3.796349414716898796, -11.91283353888524843 ) ) ;
#27480 = CARTESIAN_POINT ( 'NONE',  ( -15.99999999999998579, -56.99999999999997868, 154.9999999999999716 ) ) ;
#27481 = VERTEX_POINT ( 'NONE', #12115 ) ;
#27482 = DIRECTION ( 'NONE',  ( -1.000000000000000000, -0.000000000000000000, -0.000000000000000000 ) ) ;
#27483 = DIRECTION ( 'NONE',  ( -1.232595164407830946E-32, 0.000000000000000000, -1.000000000000000000 ) ) ;
#27484 = EDGE_LOOP ( 'NONE', ( #9853, #1391, #15631, #21666, #20549, #16700 ) ) ;
#27485 = DIRECTION ( 'NONE',  ( 0.000000000000000000, 1.836970198721029441E-16, -1.000000000000000000 ) ) ;
#27486 = CARTESIAN_POINT ( 'NONE',  ( -12.00000000000001066, 104.9999999999999858, -175.0000000000000284 ) ) ;
#27487 = CARTESIAN_POINT ( 'NONE',  ( -5.021133111225196011, -21.54630831098063837, -67.50000000000000000 ) ) ;
#27488 = AXIS2_PLACEMENT_3D ( 'NONE', #34650, #21114, #26805 ) ;
#27489 = DIRECTION ( 'NONE',  ( -1.000000000000000000, 0.000000000000000000, -0.000000000000000000 ) ) ;
#27490 = ORIENTED_EDGE ( 'NONE', *, *, #23967, .T. ) ;
#27491 = VECTOR ( 'NONE', #13799, 1000.000000000000000 ) ;
#27492 = VECTOR ( 'NONE', #1790, 1000.000000000000000 ) ;
#27493 = CARTESIAN_POINT ( 'NONE',  ( -7.700000000000000178, 0.000000000000000000, 0.000000000000000000 ) ) ;
#27494 = ORIENTED_EDGE ( 'NONE', *, *, #29299, .F. ) ;
#27496 = CARTESIAN_POINT ( 'NONE',  ( 2.719010676179473229, -27.07245655034563114, -16.48110659958421920 ) ) ;
#27495 = CARTESIAN_POINT ( 'NONE',  ( 2.783084753007022627, 27.98916443103619045, -12.86217335695007868 ) ) ;
#27497 = ORIENTED_EDGE ( 'NONE', *, *, #28341, .T. ) ;
#27498 = CARTESIAN_POINT ( 'NONE',  ( -361.0000000000000000, 124.9999999999999432, 183.0000000000000000 ) ) ;
#27499 = CYLINDRICAL_SURFACE ( 'NONE', #20543, 10.00000000000000000 ) ;
#27500 = EDGE_LOOP ( 'NONE', ( #31705, #6415, #30001, #30131 ) ) ;
#27501 = ORIENTED_EDGE ( 'NONE', *, *, #15053, .F. ) ;
#27502 = VECTOR ( 'NONE', #2945, 1000.000000000000000 ) ;
#27503 = ORIENTED_EDGE ( 'NONE', *, *, #9771, .T. ) ;
#27504 = DIRECTION ( 'NONE',  ( 0.000000000000000000, 1.000000000000000000, 0.000000000000000000 ) ) ;
#27505 = CARTESIAN_POINT ( 'NONE',  ( 2.789999999999999147, 6.312585643774527355, 29.77790610619688394 ) ) ;
#27506 = ORIENTED_EDGE ( 'NONE', *, *, #28224, .T. ) ;
#27507 = VERTEX_POINT ( 'NONE', #9252 ) ;
#27508 = LINE ( 'NONE', #815, #15027 ) ;
#27509 = EDGE_CURVE ( 'NONE', #14780, #16444, #32110, .T. ) ;
#27510 = DIRECTION ( 'NONE',  ( -0.000000000000000000, -0.000000000000000000, -1.000000000000000000 ) ) ;
#27511 = CARTESIAN_POINT ( 'NONE',  ( -355.0000000000000000, 118.9999999999999858, 111.9999999999999858 ) ) ;
#27512 = ADVANCED_FACE ( 'NONE', ( #33810 ), #33455, .T. ) ;
#27513 = AXIS2_PLACEMENT_3D ( 'NONE', #26009, #28851, #9812 ) ;
#27514 = CARTESIAN_POINT ( 'NONE',  ( -418.0000000000000000, -105.0000000000000142, 190.9999999999999716 ) ) ;
#27515 = CARTESIAN_POINT ( 'NONE',  ( -20.00000000000007461, 112.9999999999999574, -190.9999999999999716 ) ) ;
#27516 = VERTEX_POINT ( 'NONE', #14615 ) ;
#27517 = VERTEX_POINT ( 'NONE', #25440 ) ;
#27518 = VECTOR ( 'NONE', #15477, 1000.000000000000000 ) ;
#27519 = DIRECTION ( 'NONE',  ( 0.000000000000000000, 5.053935297177146739E-49, 1.000000000000000000 ) ) ;
#27520 = LINE ( 'NONE', #28312, #16405 ) ;
#27521 = EDGE_CURVE ( 'NONE', #26887, #34290, #716, .T. ) ;
#27522 = CARTESIAN_POINT ( 'NONE',  ( -349.0000000000000000, 124.9999999999999432, 183.0000000000000000 ) ) ;
#27523 = AXIS2_PLACEMENT_3D ( 'NONE', #4589, #2122, #31829 ) ;
#27524 = CARTESIAN_POINT ( 'NONE',  ( 1.749999999999999778, 6.714005886384948774, 33.75364837705175347 ) ) ;
#27525 = DIRECTION ( 'NONE',  ( 1.000000000000000000, 3.469446951953834515E-18, 0.000000000000000000 ) ) ;
#27526 = LINE ( 'NONE', #7953, #29968 ) ;
#27527 = DIRECTION ( 'NONE',  ( 1.000000000000000000, 0.000000000000000000, 0.000000000000000000 ) ) ;
#27528 = ORIENTED_EDGE ( 'NONE', *, *, #23745, .T. ) ;
#27529 = DIRECTION ( 'NONE',  ( -1.000000000000000000, 0.000000000000000000, 0.000000000000000000 ) ) ;
#27530 = CARTESIAN_POINT ( 'NONE',  ( 2.790000000000081304, 4.061185680397615627, -30.39260865248084187 ) ) ;
#27531 = CARTESIAN_POINT ( 'NONE',  ( 8.000000000000000000, 0.000000000000000000, 0.000000000000000000 ) ) ;
#27532 = ORIENTED_EDGE ( 'NONE', *, *, #10636, .T. ) ;
#27533 = VECTOR ( 'NONE', #13082, 1000.000000000000000 ) ;
#27534 = CARTESIAN_POINT ( 'NONE',  ( 0.000000000000000000, 23.28319895603611300, -21.86437915510192909 ) ) ;
#27535 = ORIENTED_EDGE ( 'NONE', *, *, #20451, .T. ) ;
#27536 = CARTESIAN_POINT ( 'NONE',  ( -418.0000000000000000, 113.0000000000000000, -175.0000000000000000 ) ) ;
#27537 = CARTESIAN_POINT ( 'NONE',  ( -107.2815281471303450, 4.590414103366523335, 11.62745871345765991 ) ) ;
#27538 = DIRECTION ( 'NONE',  ( 0.000000000000000000, 0.000000000000000000, -1.000000000000000000 ) ) ;
#27539 = AXIS2_PLACEMENT_3D ( 'NONE', #23045, #23216, #31221 ) ;
#27540 = ORIENTED_EDGE ( 'NONE', *, *, #32921, .T. ) ;
#27541 = CIRCLE ( 'NONE', #3656, 32.54542015209054995 ) ;
#27542 = DIRECTION ( 'NONE',  ( 0.000000000000000000, 0.000000000000000000, 1.000000000000000000 ) ) ;
#27543 = DIRECTION ( 'NONE',  ( 0.000000000000000000, 0.000000000000000000, 1.000000000000000000 ) ) ;
#27544 = LINE ( 'NONE', #3508, #34227 ) ;
#27545 = CIRCLE ( 'NONE', #32674, 3.999999999999982681 ) ;
#27546 = ORIENTED_EDGE ( 'NONE', *, *, #2651, .F. ) ;
#27547 = DIRECTION ( 'NONE',  ( 2.631201909438060585E-14, -5.396010391056496978E-16, 1.000000000000000000 ) ) ;
#27548 = DIRECTION ( 'NONE',  ( 0.9868265225415261410, -0.1617819965527648174, 0.000000000000000000 ) ) ;
#27549 = ORIENTED_EDGE ( 'NONE', *, *, #16240, .F. ) ;
#27550 = CARTESIAN_POINT ( 'NONE',  ( -361.0000000000000000, 124.9999999999999432, 166.9999999999999716 ) ) ;
#27551 = EDGE_CURVE ( 'NONE', #13276, #30004, #22960, .T. ) ;
#27552 = CARTESIAN_POINT ( 'NONE',  ( 2.261199742992266337, -33.38088972941607580, 0.7716149733912494035 ) ) ;
#27553 = VECTOR ( 'NONE', #16421, 1000.000000000000114 ) ;
#27554 = CARTESIAN_POINT ( 'NONE',  ( 5.021133111224679091, 24.02303923978505296, -87.50000000000000000 ) ) ;
#27555 = CARTESIAN_POINT ( 'NONE',  ( -109.4057322091481694, -2.603972021169313145, 7.035140931575562639 ) ) ;
#27556 = ORIENTED_EDGE ( 'NONE', *, *, #15615, .T. ) ;
#27557 = ORIENTED_EDGE ( 'NONE', *, *, #28844, .F. ) ;
#27558 = ORIENTED_EDGE ( 'NONE', *, *, #8881, .T. ) ;
#27559 = EDGE_CURVE ( 'NONE', #16257, #11365, #33630, .T. ) ;
#27560 = LINE ( 'NONE', #870, #24907 ) ;
#27561 = AXIS2_PLACEMENT_3D ( 'NONE', #19395, #11915, #6187 ) ;
#27562 = EDGE_CURVE ( 'NONE', #9321, #16675, #8720, .T. ) ;
#27563 = CYLINDRICAL_SURFACE ( 'NONE', #25083, 34.41491905851385269 ) ;
#27564 = DIRECTION ( 'NONE',  ( 1.000000000000000000, 0.000000000000000000, 0.000000000000000000 ) ) ;
#27565 = CIRCLE ( 'NONE', #9391, 4.000000000000003553 ) ;
#27566 = ORIENTED_EDGE ( 'NONE', *, *, #25785, .T. ) ;
#27567 = VERTEX_POINT ( 'NONE', #30441 ) ;
#27568 = EDGE_CURVE ( 'NONE', #31871, #22788, #33844, .T. ) ;
#27569 = EDGE_CURVE ( 'NONE', #20636, #9157, #27938, .T. ) ;
#27570 = CARTESIAN_POINT ( 'NONE',  ( -365.0000000000000000, 118.9999999999999716, 111.9999999999999858 ) ) ;
#27571 = ORIENTED_EDGE ( 'NONE', *, *, #25448, .F. ) ;
#27572 = AXIS2_PLACEMENT_3D ( 'NONE', #28200, #22697, #25700 ) ;
#27573 = CYLINDRICAL_SURFACE ( 'NONE', #2186, 2.033421858999711951 ) ;
#27574 = EDGE_CURVE ( 'NONE', #15307, #11484, #3682, .T. ) ;
#27575 = DIRECTION ( 'NONE',  ( -1.000000000000000000, 0.000000000000000000, 0.000000000000000000 ) ) ;
#27576 = ORIENTED_EDGE ( 'NONE', *, *, #15295, .T. ) ;
#27577 = EDGE_LOOP ( 'NONE', ( #19389, #17317, #1784, #867, #19399, #11851, #27073, #30989 ) ) ;
#27578 = CARTESIAN_POINT ( 'NONE',  ( -20.02113311122509032, -11.61907005722761532, -67.50000000000000000 ) ) ;
#27579 = CARTESIAN_POINT ( 'NONE',  ( -442.0000000000000000, 105.0000000000000142, 107.9999999999999858 ) ) ;
#27580 = ORIENTED_EDGE ( 'NONE', *, *, #22942, .F. ) ;
#27581 = DIRECTION ( 'NONE',  ( -0.000000000000000000, -0.000000000000000000, -1.000000000000000000 ) ) ;
#27582 = CARTESIAN_POINT ( 'NONE',  ( -143.0000000000000568, -45.49999999999999289, 65.00000000000000000 ) ) ;
#27583 = LINE ( 'NONE', #3196, #1362 ) ;
#27584 = AXIS2_PLACEMENT_3D ( 'NONE', #21312, #13312, #19181 ) ;
#27585 = VECTOR ( 'NONE', #29057, 1000.000000000000000 ) ;
#27586 = DIRECTION ( 'NONE',  ( -1.000000000000000000, -0.000000000000000000, -0.000000000000000000 ) ) ;
#27587 = FACE_OUTER_BOUND ( 'NONE', #32883, .T. ) ;
#27588 = DIRECTION ( 'NONE',  ( 0.000000000000000000, 1.836970198721029441E-16, -1.000000000000000000 ) ) ;
#27589 = AXIS2_PLACEMENT_3D ( 'NONE', #31425, #14900, #7028 ) ;
#27590 = ORIENTED_EDGE ( 'NONE', *, *, #14279, .F. ) ;
#27591 = AXIS2_PLACEMENT_3D ( 'NONE', #28072, #25217, #30398 ) ;
#27592 = CARTESIAN_POINT ( 'NONE',  ( 829.1381798504595508, 1235.487045258097396, 1753.598338701303646 ) ) ;
#27593 = ORIENTED_EDGE ( 'NONE', *, *, #13570, .T. ) ;
#27594 = AXIS2_PLACEMENT_3D ( 'NONE', #6824, #21056, #2189 ) ;
#27595 = ORIENTED_EDGE ( 'NONE', *, *, #3726, .F. ) ;
#27596 = LINE ( 'NONE', #11774, #19605 ) ;
#27597 = DIRECTION ( 'NONE',  ( -0.000000000000000000, 1.836970198721029688E-16, -1.000000000000000000 ) ) ;
#27598 = APPLICATION_PROTOCOL_DEFINITION ( 'draft international standard', 'automotive_design', 1998, #21229 ) ;
#27599 = ORIENTED_EDGE ( 'NONE', *, *, #7941, .F. ) ;
#27600 = DIRECTION ( 'NONE',  ( 0.000000000000000000, 1.000000000000000000, 5.145227585319922065E-49 ) ) ;
#27601 = ADVANCED_FACE ( 'NONE', ( #28639 ), #34506, .F. ) ;
#27603 = CARTESIAN_POINT ( 'NONE',  ( 2.765921099433441110, -17.95514392185398833, -25.38201125280375692 ) ) ;
#27602 = CARTESIAN_POINT ( 'NONE',  ( -349.0000000000000000, -125.0000000000000284, 111.9999999999999858 ) ) ;
#27604 = ORIENTED_EDGE ( 'NONE', *, *, #9970, .F. ) ;
#27605 = ORIENTED_EDGE ( 'NONE', *, *, #20531, .T. ) ;
#27606 = EDGE_CURVE ( 'NONE', #22562, #2115, #20983, .T. ) ;
#27607 = EDGE_CURVE ( 'NONE', #17615, #8779, #19638, .T. ) ;
#27608 = DIRECTION ( 'NONE',  ( 1.000000000000000000, 0.000000000000000000, 0.000000000000000000 ) ) ;
#27609 = AXIS2_PLACEMENT_3D ( 'NONE', #9842, #7509, #29240 ) ;
#27610 = CARTESIAN_POINT ( 'NONE',  ( 0.02407890056655695096, 11.80989368511462523, 28.76039115933989976 ) ) ;
#27611 = CYLINDRICAL_SURFACE ( 'NONE', #23379, 4.750000000000004441 ) ;
#27612 = DIRECTION ( 'NONE',  ( 0.000000000000000000, 1.836970198721029934E-16, -1.000000000000000000 ) ) ;
#27613 = VERTEX_POINT ( 'NONE', #7261 ) ;
#27614 = DIRECTION ( 'NONE',  ( 1.000000000000000000, 0.000000000000000000, 0.000000000000000000 ) ) ;
#27615 = DIRECTION ( 'NONE',  ( -0.000000000000000000, -0.000000000000000000, -1.000000000000000000 ) ) ;
#27616 = CARTESIAN_POINT ( 'NONE',  ( 0.8377008405913450861, 8.431745484731994367, 12.39578842395470737 ) ) ;
#27617 =( REPRESENTATION_RELATIONSHIP ('NONE','NONE', #23037, #15767 ) REPRESENTATION_RELATIONSHIP_WITH_TRANSFORMATION ( #3347 )SHAPE_REPRESENTATION_RELATIONSHIP( ) );
#27618 = ORIENTED_EDGE ( 'NONE', *, *, #23868, .F. ) ;
#27619 = VECTOR ( 'NONE', #8894, 1000.000000000000000 ) ;
#27620 = CARTESIAN_POINT ( 'NONE',  ( 2.789999999999999147, -20.35927063852789232, -22.08513060777193004 ) ) ;
#27621 = CARTESIAN_POINT ( 'NONE',  ( 0.02407890056655651728, 7.350529080603541487, 30.20932655202940254 ) ) ;
#27622 = ADVANCED_FACE ( 'NONE', ( #20634 ), #10123, .F. ) ;
#27623 = DIRECTION ( 'NONE',  ( -0.8835120444460228262, 0.4684084406997903183, 0.000000000000000000 ) ) ;
#27625 = PLANE ( 'NONE',  #8286 ) ;
#27624 = DIRECTION ( 'NONE',  ( -1.000000000000000000, -0.000000000000000000, -0.000000000000000000 ) ) ;
#27626 = CIRCLE ( 'NONE', #21939, 1.999999999999999556 ) ;
#27627 = LINE ( 'NONE', #10567, #1381 ) ;
#27628 = VERTEX_POINT ( 'NONE', #31999 ) ;
#27629 = DIRECTION ( 'NONE',  ( 0.9766205557100864354, -0.2149704402110247659, 0.000000000000000000 ) ) ;
#27630 = DIRECTION ( 'NONE',  ( 0.000000000000000000, -1.000000000000000000, 6.123233995736766036E-17 ) ) ;
#27631 = EDGE_CURVE ( 'NONE', #18417, #22127, #9949, .T. ) ;
#27632 = ADVANCED_FACE ( 'NONE', ( #26493 ), #23308, .T. ) ;
#27633 = EDGE_CURVE ( 'NONE', #14045, #30081, #18162, .T. ) ;
#27634 = VECTOR ( 'NONE', #20183, 1000.000000000000000 ) ;
#27635 = ORIENTED_EDGE ( 'NONE', *, *, #34927, .F. ) ;
#27636 = VECTOR ( 'NONE', #32171, 1000.000000000000000 ) ;
#27637 = EDGE_CURVE ( 'NONE', #19620, #9427, #13928, .T. ) ;
#27638 = VERTEX_POINT ( 'NONE', #14955 ) ;
#27639 = ORIENTED_EDGE ( 'NONE', *, *, #11403, .F. ) ;
#27640 = CARTESIAN_POINT ( 'NONE',  ( -418.0000000000000000, 105.0000000000000142, -175.0000000000000000 ) ) ;
#27641 = ORIENTED_EDGE ( 'NONE', *, *, #28297, .T. ) ;
#27642 = ORIENTED_EDGE ( 'NONE', *, *, #5572, .T. ) ;
#27643 = DIRECTION ( 'NONE',  ( 0.000000000000000000, -1.000000000000000000, 6.123233995736766036E-17 ) ) ;
#27644 = VECTOR ( 'NONE', #25169, 1000.000000000000000 ) ;
#27645 = CONTEXT_DEPENDENT_SHAPE_REPRESENTATION ( #9223, #31072 ) ;
#27646 = ORIENTED_EDGE ( 'NONE', *, *, #24953, .F. ) ;
#27647 = LINE ( 'NONE', #29793, #20375 ) ;
#27648 = CARTESIAN_POINT ( 'NONE',  ( 2.789999999999999147, 0.000000000000000000, 0.000000000000000000 ) ) ;
#27649 = EDGE_LOOP ( 'NONE', ( #16980, #29537, #14367, #13189 ) ) ;
#27650 = ORIENTED_EDGE ( 'NONE', *, *, #16488, .F. ) ;
#27651 = EDGE_CURVE ( 'NONE', #24189, #4119, #4243, .T. ) ;
#27652 = DIRECTION ( 'NONE',  ( -0.3193015301359781177, 0.9476531711828031224, 1.740810634186287624E-16 ) ) ;
#27653 = CYLINDRICAL_SURFACE ( 'NONE', #23207, 22.50000000000000355 ) ;
#27654 = CARTESIAN_POINT ( 'NONE',  ( 110.4388056112352956, -1.867505626284029940, -12.36477516193776260 ) ) ;
#27655 = CARTESIAN_POINT ( 'NONE',  ( -349.0000000000000000, 134.9999999999999716, 128.0000000000000000 ) ) ;
#27656 = ORIENTED_EDGE ( 'NONE', *, *, #31895, .F. ) ;
#27657 = VECTOR ( 'NONE', #3751, 1000.000000000000114 ) ;
#27658 = DIRECTION ( 'NONE',  ( 0.000000000000000000, 1.000000000000000000, -6.123233995736766036E-17 ) ) ;
#27659 = CARTESIAN_POINT ( 'NONE',  ( -12.00000000000001066, 144.9999999999999716, 194.9999999999999716 ) ) ;
#27660 = ORIENTED_EDGE ( 'NONE', *, *, #25737, .F. ) ;
#27661 = CARTESIAN_POINT ( 'NONE',  ( -8.499999999999998224, 0.000000000000000000, 3.930000000000000160 ) ) ;
#27662 = CARTESIAN_POINT ( 'NONE',  ( 0.000000000000000000, 3.909681563762119172, -30.21863799912381054 ) ) ;
#27663 = CARTESIAN_POINT ( 'NONE',  ( 1.749999999999999778, -18.21166265554811403, 29.20140402659732359 ) ) ;
#27664 = CYLINDRICAL_SURFACE ( 'NONE', #10372, 10.00000000000000000 ) ;
#27665 = DIRECTION ( 'NONE',  ( 0.000000000000000000, 0.000000000000000000, 1.000000000000000000 ) ) ;
#27666 = CYLINDRICAL_SURFACE ( 'NONE', #6438, 2.033421858999711507 ) ;
#27667 = VERTEX_POINT ( 'NONE', #21155 ) ;
#27669 = CARTESIAN_POINT ( 'NONE',  ( 0.000000000000000000, 0.000000000000000000, 0.000000000000000000 ) ) ;
#27668 = LINE ( 'NONE', #16846, #2332 ) ;
#27670 = B_SPLINE_CURVE_WITH_KNOTS ( 'NONE', 3,
 ( #16227, #27059, #14953, #28467, #33281, #22431 ),
 .UNSPECIFIED., .F., .F.,
 ( 4, 2, 4 ),
 ( 2.078540817596000944E-07, 0.001873406157010270006, 0.003746604459938780371 ),
 .UNSPECIFIED. ) ;
#27671 = ADVANCED_FACE ( 'NONE', ( #1930 ), #4258, .T. ) ;
#27672 = EDGE_CURVE ( 'NONE', #28835, #19630, #12813, .T. ) ;
#27673 = ORIENTED_EDGE ( 'NONE', *, *, #3839, .F. ) ;
#27674 = DIRECTION ( 'NONE',  ( -0.000000000000000000, 1.000000000000000000, -0.000000000000000000 ) ) ;
#27675 = DIRECTION ( 'NONE',  ( 0.000000000000000000, 1.000000000000000000, 1.224646799147353207E-16 ) ) ;
#27676 = ORIENTED_EDGE ( 'NONE', *, *, #1099, .F. ) ;
#27677 = EDGE_LOOP ( 'NONE', ( #30036, #2820, #9626, #18139 ) ) ;
#27678 = AXIS2_PLACEMENT_3D ( 'NONE', #9059, #19923, #6375 ) ;
#27679 = CIRCLE ( 'NONE', #1548, 2.525000000000000799 ) ;
#27680 = ORIENTED_EDGE ( 'NONE', *, *, #29895, .F. ) ;
#27681 = DIRECTION ( 'NONE',  ( 1.000000000000000000, 0.000000000000000000, 0.000000000000000000 ) ) ;
#27682 = CARTESIAN_POINT ( 'NONE',  ( -499.9999999999999432, -145.0000000000000000, -187.0000000000000000 ) ) ;
#27683 = ORIENTED_EDGE ( 'NONE', *, *, #12675, .T. ) ;
#27684 = ORIENTED_EDGE ( 'NONE', *, *, #13661, .F. ) ;
#27685 = CARTESIAN_POINT ( 'NONE',  ( -12.91951790633627439, -3.497874208484963443, -14.98024667272714083 ) ) ;
#27686 = CARTESIAN_POINT ( 'NONE',  ( -19.99999999999998934, 112.9999999999999574, -155.0000000000000000 ) ) ;
#27687 = CARTESIAN_POINT ( 'NONE',  ( 2.606461903588221940, -22.67993007562043317, -22.95754798008726993 ) ) ;
#27688 = DIRECTION ( 'NONE',  ( 2.891205793294675368E-16, 0.000000000000000000, -1.000000000000000000 ) ) ;
#27689 = B_SPLINE_CURVE_WITH_KNOTS ( 'NONE', 3,
 ( #9587, #25769, #26465, #17783, #14935, #4557 ),
 .UNSPECIFIED., .F., .F.,
 ( 4, 2, 4 ),
 ( 2.555309558362774114E-07, 0.001873453885876978078, 0.003746652240798119780 ),
 .UNSPECIFIED. ) ;
#27690 = ORIENTED_EDGE ( 'NONE', *, *, #21100, .T. ) ;
#27691 = ORIENTED_EDGE ( 'NONE', *, *, #9991, .F. ) ;
#27692 = CARTESIAN_POINT ( 'NONE',  ( 0.1859802785888828025, -31.54566302605132222, 6.854274004867739301 ) ) ;
#27694 = VECTOR ( 'NONE', #17439, 1000.000000000000000 ) ;
#27693 = CARTESIAN_POINT ( 'NONE',  ( 1.395000000000002238, 27.68252950111368094, -20.44661865013457813 ) ) ;
#27695 = CARTESIAN_POINT ( 'NONE',  ( -23.78520691327551262, 22.21414650552148373, 68.31122994652405112 ) ) ;
#27696 = DIRECTION ( 'NONE',  ( 0.000000000000000000, 0.000000000000000000, 1.000000000000000000 ) ) ;
#27697 = LINE ( 'NONE', #3314, #8624 ) ;
#27698 = LINE ( 'NONE', #19186, #20215 ) ;
#27699 = CIRCLE ( 'NONE', #32242, 3.999999999999976019 ) ;
#27700 = DIRECTION ( 'NONE',  ( 0.000000000000000000, 0.7071067811865462405, -0.7071067811865489050 ) ) ;
#27701 = DIRECTION ( 'NONE',  ( -0.000000000000000000, 1.836970198721029934E-16, -1.000000000000000000 ) ) ;
#27702 = ORIENTED_EDGE ( 'NONE', *, *, #8583, .F. ) ;
#27703 = EDGE_CURVE ( 'NONE', #4014, #2214, #26984, .T. ) ;
#27704 = DIRECTION ( 'NONE',  ( -0.000000000000000000, 2.309213040847544338E-50, 1.000000000000000000 ) ) ;
#27705 = FACE_OUTER_BOUND ( 'NONE', #34534, .T. ) ;
#27706 = CARTESIAN_POINT ( 'NONE',  ( -20.72055270933793736, 25.09707290294328885, 68.31122994652405112 ) ) ;
#27707 = ORIENTED_EDGE ( 'NONE', *, *, #26715, .T. ) ;
#27708 = AXIS2_PLACEMENT_3D ( 'NONE', #7155, #17704, #9667 ) ;
#27709 = AXIS2_PLACEMENT_3D ( 'NONE', #31340, #3926, #22990 ) ;
#27710 = FACE_BOUND ( 'NONE', #18141, .T. ) ;
#27711 = EDGE_LOOP ( 'NONE', ( #6991, #27540, #2724, #28461 ) ) ;
#27712 = LINE ( 'NONE', #16885, #15647 ) ;
#27713 = LINE ( 'NONE', #20077, #25611 ) ;
#27714 = ADVANCED_FACE ( 'NONE', ( #7435 ), #4064, .F. ) ;
#27715 = AXIS2_PLACEMENT_3D ( 'NONE', #19351, #5789, #9015 ) ;
#27716 = EDGE_CURVE ( 'NONE', #33784, #27140, #15659, .T. ) ;
#27717 = EDGE_CURVE ( 'NONE', #109, #12045, #31307, .T. ) ;
#27718 = VERTEX_POINT ( 'NONE', #9773 ) ;
#27719 = CARTESIAN_POINT ( 'NONE',  ( 5.713835024271042506, 32.03991982186466458, 68.31122994652405112 ) ) ;
#27720 = DIRECTION ( 'NONE',  ( 1.000000000000000000, 0.000000000000000000, 0.000000000000000000 ) ) ;
#27722 = PLANE ( 'NONE',  #6948 ) ;
#27721 = PRODUCT_DEFINITION ( 'UNKNOWN', '', #25220, #2500 ) ;
#27723 = ORIENTED_EDGE ( 'NONE', *, *, #31577, .F. ) ;
#27724 = CIRCLE ( 'NONE', #26017, 7.999999999999986677 ) ;
#27725 = CARTESIAN_POINT ( 'NONE',  ( 849.1928862901987713, 1048.057004850247267, 1753.598338701303419 ) ) ;
#27726 = LINE ( 'NONE', #11542, #16479 ) ;
#27727 = VERTEX_POINT ( 'NONE', #17988 ) ;
#27728 = PLANE ( 'NONE',  #3618 ) ;
#27729 = FILL_AREA_STYLE_COLOUR ( '', #31193 ) ;
#27730 = AXIS2_PLACEMENT_3D ( 'NONE', #16222, #9248, #33450 ) ;
#27731 = FACE_OUTER_BOUND ( 'NONE', #17496, .T. ) ;
#27732 = CARTESIAN_POINT ( 'NONE',  ( -109.9401885228446645, -1.370240552585045180, 7.381692049079063622 ) ) ;
#27733 = VERTEX_POINT ( 'NONE', #24687 ) ;
#27734 = VERTEX_POINT ( 'NONE', #18682 ) ;
#27735 = ORIENTED_EDGE ( 'NONE', *, *, #32646, .F. ) ;
#27736 = CARTESIAN_POINT ( 'NONE',  ( -2.448281906437820454E-16, -29.22790002295985090, 9.266248432308520577 ) ) ;
#27737 = B_SPLINE_CURVE_WITH_KNOTS ( 'NONE', 3,
 ( #5286, #27356, #10824, #2973 ),
 .UNSPECIFIED., .F., .F.,
 ( 4, 4 ),
 ( 0.005298484651059772073, 0.005985351487543621660 ),
 .UNSPECIFIED. ) ;
#27738 = CARTESIAN_POINT ( 'NONE',  ( 2.261199765623164826, -29.62362497318111920, -15.40519487321921765 ) ) ;
#27739 = VECTOR ( 'NONE', #6273, 1000.000000000000000 ) ;
#27740 = CARTESIAN_POINT ( 'NONE',  ( 22.89764159710615132, -1.579009122040562207, -77.50000000000000000 ) ) ;
#27741 = VERTEX_POINT ( 'NONE', #23986 ) ;
#27742 = ORIENTED_EDGE ( 'NONE', *, *, #15404, .T. ) ;
#27743 = CARTESIAN_POINT ( 'NONE',  ( 2.765921099433441110, -17.95514392185398833, -25.38201125280375692 ) ) ;
#27744 = EDGE_LOOP ( 'NONE', ( #28511, #34125, #27255, #24082 ) ) ;
#27745 = LINE ( 'NONE', #3360, #21457 ) ;
#27746 = DIRECTION ( 'NONE',  ( -0.000000000000000000, -0.000000000000000000, -1.000000000000000000 ) ) ;
#27747 = ORIENTED_EDGE ( 'NONE', *, *, #3213, .F. ) ;
#27748 = ORIENTED_EDGE ( 'NONE', *, *, #1447, .T. ) ;
#27749 = CARTESIAN_POINT ( 'NONE',  ( -3.250000000000000000, -5.838643359331793015, 3.180000000000000160 ) ) ;
#27750 = AXIS2_PLACEMENT_3D ( 'NONE', #10545, #5354, #19267 ) ;
#27751 = ADVANCED_FACE ( 'NONE', ( #16362 ), #27193, .F. ) ;
#27752 = CARTESIAN_POINT ( 'NONE',  ( -418.0000000000000000, -125.0000000000000000, 162.9999999999999716 ) ) ;
#27753 = ORIENTED_EDGE ( 'NONE', *, *, #5963, .F. ) ;
#27754 = CARTESIAN_POINT ( 'NONE',  ( 2.765921099433442443, 20.99477179376825120, 22.93149026599753526 ) ) ;
#27755 = EDGE_CURVE ( 'NONE', #14836, #14594, #2802, .T. ) ;
#27756 = DIRECTION ( 'NONE',  ( 0.000000000000000000, 0.000000000000000000, 1.000000000000000000 ) ) ;
#27757 = CARTESIAN_POINT ( 'NONE',  ( 30.69344702212033127, -10.82204614554912325, 49.43553178847298568 ) ) ;
#27758 = AXIS2_PLACEMENT_3D ( 'NONE', #27772, #30451, #22966 ) ;
#27759=STYLED_ITEM('',(#35254),#11234);
#27760 = DIRECTION ( 'NONE',  ( 1.000000000000000000, 0.000000000000000000, -1.232595164407831220E-32 ) ) ;
#27761 = CARTESIAN_POINT ( 'NONE',  ( -355.0000000000000000, 118.9999999999999716, 109.9999999999999858 ) ) ;
#27763 = EDGE_CURVE ( 'NONE', #27067, #15570, #5116, .T. ) ;
#27762 = SURFACE_SIDE_STYLE ('',( #5508 ) ) ;
#27764 = EDGE_LOOP ( 'NONE', ( #12945, #30202, #20889, #12224 ) ) ;
#27765 = AXIS2_PLACEMENT_3D ( 'NONE', #14943, #21741, #19271 ) ;
#27766 = ORIENTED_EDGE ( 'NONE', *, *, #25497, .T. ) ;
#27767 = CARTESIAN_POINT ( 'NONE',  ( 842.9690118778659098, 1106.224948425097409, 1753.598338701303646 ) ) ;
#27768 = ORIENTED_EDGE ( 'NONE', *, *, #1408, .F. ) ;
#27769 = EDGE_LOOP ( 'NONE', ( #4377, #10270, #6092, #10367 ) ) ;
#27770 = EDGE_CURVE ( 'NONE', #31774, #2524, #2278, .T. ) ;
#27771 = EDGE_CURVE ( 'NONE', #29651, #30403, #23609, .T. ) ;
#27772 = CARTESIAN_POINT ( 'NONE',  ( -20.63749999999999929, 0.000000000000000000, 0.000000000000000000 ) ) ;
#27773 = AXIS2_PLACEMENT_3D ( 'NONE', #15858, #16872, #13172 ) ;
#27774 = LINE ( 'NONE', #24918, #13093 ) ;
#27775 = APPLICATION_PROTOCOL_DEFINITION ( 'draft international standard', 'automotive_design', 1998, #18084 ) ;
#27776 = ORIENTED_EDGE ( 'NONE', *, *, #20000, .T. ) ;
#27777 = DIRECTION ( 'NONE',  ( 1.000000000000000000, 0.000000000000000000, 0.000000000000000000 ) ) ;
#27778 = CARTESIAN_POINT ( 'NONE',  ( -101.6217835190355885, -3.855135278743967220, -11.89320834461815934 ) ) ;
#27779 = CIRCLE ( 'NONE', #5586, 7.999999999999979572 ) ;
#27781 = DIRECTION ( 'NONE',  ( -1.000000000000000000, 0.000000000000000000, 0.000000000000000000 ) ) ;
#27780 = LINE ( 'NONE', #17123, #15030 ) ;
#27782 = EDGE_LOOP ( 'NONE', ( #32971, #29438, #3296, #9082 ) ) ;
#27783 = ORIENTED_EDGE ( 'NONE', *, *, #21401, .F. ) ;
#27784 = FACE_OUTER_BOUND ( 'NONE', #5401, .T. ) ;
#27785 = DIRECTION ( 'NONE',  ( 0.000000000000000000, 1.836970198721029441E-16, -1.000000000000000000 ) ) ;
#27786 = FACE_OUTER_BOUND ( 'NONE', #22759, .T. ) ;
#27787 = DIRECTION ( 'NONE',  ( 1.000000000000000000, 0.000000000000000000, 0.000000000000000000 ) ) ;
#27788 = ORIENTED_EDGE ( 'NONE', *, *, #4767, .T. ) ;
#27789 = AXIS2_PLACEMENT_3D ( 'NONE', #27343, #7954, #16166 ) ;
#27790 = DIRECTION ( 'NONE',  ( -0.2675283385292216987, 0.9635499925192227977, -0.000000000000000000 ) ) ;
#27791 = CARTESIAN_POINT ( 'NONE',  ( 19.99999999999998224, -55.00000000000000711, -158.9999999999999716 ) ) ;
#27792 = DIRECTION ( 'NONE',  ( 0.000000000000000000, 0.000000000000000000, -1.000000000000000000 ) ) ;
#27793 = ORIENTED_EDGE ( 'NONE', *, *, #7238, .F. ) ;
#27794 = CARTESIAN_POINT ( 'NONE',  ( 2.719010685383924208, 31.58942871418359744, -2.579295332369116789 ) ) ;
#27795 = CARTESIAN_POINT ( 'NONE',  ( 60.00000000000000000, -33.69708579775584667, 49.43553178847298568 ) ) ;
#27796 = CARTESIAN_POINT ( 'NONE',  ( 13.32059394339353986, -35.43959265050634144, 68.31122994652405112 ) ) ;
#27798 = CARTESIAN_POINT ( 'NONE',  ( 0.1396634953560761672, 2.649662288454536441, 13.50000000000000000 ) ) ;
#27797 = DIRECTION ( 'NONE',  ( -1.000000000000000000, 0.000000000000000000, 0.000000000000000000 ) ) ;
#27799 = UNCERTAINTY_MEASURE_WITH_UNIT (LENGTH_MEASURE( 1.000000000000000082E-05 ), #1843, 'distance_accuracy_value', 'NONE');
#27800 = DIRECTION ( 'NONE',  ( 3.697785493223492838E-32, 1.934419779023891545E-16, -1.000000000000000000 ) ) ;
#27801 = ORIENTED_EDGE ( 'NONE', *, *, #16935, .F. ) ;
#27802 = FACE_OUTER_BOUND ( 'NONE', #24260, .T. ) ;
#27803 =( NAMED_UNIT ( * ) SI_UNIT ( $, .STERADIAN. ) SOLID_ANGLE_UNIT ( ) );
#27804 = EDGE_CURVE ( 'NONE', #31987, #20636, #13849, .T. ) ;
#27805 = CIRCLE ( 'NONE', #32350, 2.033421858999710619 ) ;
#27806 = ORIENTED_EDGE ( 'NONE', *, *, #11310, .T. ) ;
#27807 = EDGE_CURVE ( 'NONE', #13700, #1315, #34870, .T. ) ;
#27808 = EDGE_CURVE ( 'NONE', #2690, #29500, #32707, .T. ) ;
#27809 = ORIENTED_EDGE ( 'NONE', *, *, #5206, .T. ) ;
#27810 = AXIS2_PLACEMENT_3D ( 'NONE', #34987, #16301, #13444 ) ;
#27811 = B_SPLINE_CURVE_WITH_KNOTS ( 'NONE', 3,
 ( #4010, #14904, #1366, #17752 ),
 .UNSPECIFIED., .F., .F.,
 ( 4, 4 ),
 ( 0.005298419352602242068, 0.005985287046740441104 ),
 .UNSPECIFIED. ) ;
#27812 = ORIENTED_EDGE ( 'NONE', *, *, #5390, .F. ) ;
#27813 = DIRECTION ( 'NONE',  ( -1.000000000000000000, -0.000000000000000000, -0.000000000000000000 ) ) ;
#27814 = ORIENTED_EDGE ( 'NONE', *, *, #21303, .F. ) ;
#27815 = ORIENTED_EDGE ( 'NONE', *, *, #12425, .T. ) ;
#27816 = CARTESIAN_POINT ( 'NONE',  ( -3.250000000000000000, -5.838643359331793015, 4.679999999999999716 ) ) ;
#27817 = EDGE_CURVE ( 'NONE', #9350, #8552, #10482, .T. ) ;
#27818 = VECTOR ( 'NONE', #18184, 1000.000000000000000 ) ;
#27819 = VERTEX_POINT ( 'NONE', #35046 ) ;
#27820 = DIRECTION ( 'NONE',  ( -0.000000000000000000, 1.000000000000000000, -0.000000000000000000 ) ) ;
#27821 = CARTESIAN_POINT ( 'NONE',  ( 13.32059394339353986, -35.43959265050632013, -36.68877005347593467 ) ) ;
#27822 = EDGE_LOOP ( 'NONE', ( #11427, #9996 ) ) ;
#27823 = VERTEX_POINT ( 'NONE', #29873 ) ;
#27824 =( REPRESENTATION_RELATIONSHIP ('NONE','NONE', #23037, #15767 ) REPRESENTATION_RELATIONSHIP_WITH_TRANSFORMATION ( #11777 )SHAPE_REPRESENTATION_RELATIONSHIP( ) );
#27825 = DIRECTION ( 'NONE',  ( -0.000000000000000000, -0.000000000000000000, -1.000000000000000000 ) ) ;
#27826 = DIRECTION ( 'NONE',  ( 0.000000000000000000, 0.000000000000000000, -1.000000000000000000 ) ) ;
#27827 = ADVANCED_FACE ( 'NONE', ( #29349, #16006, #21340 ), #21513, .F. ) ;
#27828 = CARTESIAN_POINT ( 'NONE',  ( 104.2470790493104147, -5.691643476845046123, -11.12904465084466388 ) ) ;
#27829 = DIRECTION ( 'NONE',  ( 1.000000000000000000, 3.040835319149746090E-31, 1.232595164407830946E-32 ) ) ;
#27830 = DIRECTION ( 'NONE',  ( 0.000000000000000000, 0.000000000000000000, -1.000000000000000000 ) ) ;
#27831 = VERTEX_POINT ( 'NONE', #10659 ) ;
#27832 = ADVANCED_FACE ( 'NONE', ( #7793 ), #32137, .T. ) ;
#27833 = DIRECTION ( 'NONE',  ( 0.000000000000000000, -1.000000000000000000, 0.000000000000000000 ) ) ;
#27834 = EDGE_CURVE ( 'NONE', #17587, #32711, #21904, .T. ) ;
#27835 = CARTESIAN_POINT ( 'NONE',  ( -15.64512930492131382, -28.53829535743846435, 68.31122994652405112 ) ) ;
#27836 = ORIENTED_EDGE ( 'NONE', *, *, #18517, .T. ) ;
#27837 = CARTESIAN_POINT ( 'NONE',  ( -442.0000000000000000, 144.9999999999999716, -155.0000000000000000 ) ) ;
#27838 = FACE_OUTER_BOUND ( 'NONE', #21884, .T. ) ;
#27839 = LINE ( 'NONE', #14514, #26892 ) ;
#27840 = AXIS2_PLACEMENT_3D ( 'NONE', #3942, #7137, #19516 ) ;
#27841 = CARTESIAN_POINT ( 'NONE',  ( 100.0629074363043003, 2.947297676519624599, -6.904853577595275738 ) ) ;
#27842 = DIRECTION ( 'NONE',  ( 0.9635499925192227977, -0.2675283385292215321, -4.914415851915309929E-17 ) ) ;
#27843 = LINE ( 'NONE', #25883, #22957 ) ;
#27844 = ORIENTED_EDGE ( 'NONE', *, *, #2027, .T. ) ;
#27845 = CARTESIAN_POINT ( 'NONE',  ( 0.000000000000000000, 3.670182593897650235E-31, 87.50000000000000000 ) ) ;
#27847 = FACE_OUTER_BOUND ( 'NONE', #27042, .T. ) ;
#27846 = CARTESIAN_POINT ( 'NONE',  ( 5.390701026406702567, -37.47456861236020131, 68.31122994652405112 ) ) ;
#27848 = ORIENTED_EDGE ( 'NONE', *, *, #16583, .F. ) ;
#27849 = EDGE_CURVE ( 'NONE', #18440, #14675, #5471, .T. ) ;
#27850 = EDGE_CURVE ( 'NONE', #10220, #32910, #13501, .T. ) ;
#27851 = DIRECTION ( 'NONE',  ( 0.000000000000000000, 0.000000000000000000, -1.000000000000000000 ) ) ;
#27852 = CYLINDRICAL_SURFACE ( 'NONE', #25665, 3.999999999999976019 ) ;
#27853 = EDGE_LOOP ( 'NONE', ( #33254, #24009, #3941, #15385 ) ) ;
#27854 = EDGE_CURVE ( 'NONE', #11247, #4608, #30044, .T. ) ;
#27855 = ORIENTED_EDGE ( 'NONE', *, *, #13110, .F. ) ;
#27856 = FACE_OUTER_BOUND ( 'NONE', #631, .T. ) ;
#27857 = ORIENTED_EDGE ( 'NONE', *, *, #2849, .T. ) ;
#27858 = ORIENTED_EDGE ( 'NONE', *, *, #34334, .T. ) ;
#27859 = LINE ( 'NONE', #996, #33195 ) ;
#27860 = CIRCLE ( 'NONE', #13641, 11.80000000000000071 ) ;
#27861 = DIRECTION ( 'NONE',  ( 0.000000000000000000, 0.000000000000000000, 1.000000000000000000 ) ) ;
#27862 = CARTESIAN_POINT ( 'NONE',  ( -35.00000000000000000, -46.95407462254104303, -36.69637551990492597 ) ) ;
#27863 = CARTESIAN_POINT ( 'NONE',  ( 0.006915246992955798207, 27.98916443103565399, -12.86217335695007868 ) ) ;
#27864 = EDGE_LOOP ( 'NONE', ( #5653, #28350, #15829, #12278, #10038, #10723, #26463, #917, #24692 ) ) ;
#27865 = VERTEX_POINT ( 'NONE', #141 ) ;
#27866 = DIRECTION ( 'NONE',  ( 0.000000000000000000, 0.000000000000000000, -1.000000000000000000 ) ) ;
#27867 = CARTESIAN_POINT ( 'NONE',  ( 8.927936315454026328, -31.29690601358700519, 68.31122994652405112 ) ) ;
#27868 = DIRECTION ( 'NONE',  ( 0.000000000000000000, 0.5288966977476834419, 0.8486862100397269959 ) ) ;
#27869 = DIRECTION ( 'NONE',  ( -0.000000000000000000, -0.000000000000000000, -1.000000000000000000 ) ) ;
#27870 = FACE_OUTER_BOUND ( 'NONE', #22173, .T. ) ;
#27871 = ADVANCED_FACE ( 'NONE', ( #10999 ), #21851, .F. ) ;
#27872 = EDGE_CURVE ( 'NONE', #19171, #21431, #29305, .T. ) ;
#27873 = FACE_OUTER_BOUND ( 'NONE', #7895, .T. ) ;
#27874 = AXIS2_PLACEMENT_3D ( 'NONE', #21136, #34668, #26470 ) ;
#27875 = CARTESIAN_POINT ( 'NONE',  ( 0.000000000000000000, 0.000000000000000000, 20.00000000000000000 ) ) ;
#27876 = ORIENTED_EDGE ( 'NONE', *, *, #25785, .F. ) ;
#27877 = FACE_OUTER_BOUND ( 'NONE', #13106, .T. ) ;
#27878 = EDGE_CURVE ( 'NONE', #8166, #4507, #22207, .T. ) ;
#27879 = CARTESIAN_POINT ( 'NONE',  ( 11.99999999999995559, -134.9999999999999716, -154.9999999999999716 ) ) ;
#27880 = CARTESIAN_POINT ( 'NONE',  ( 0.000000000000000000, 0.000000000000000000, -0.7500000000000000000 ) ) ;
#27881 = EDGE_LOOP ( 'NONE', ( #24643, #8244, #12178, #30680 ) ) ;
#27882 = EDGE_CURVE ( 'NONE', #27945, #15892, #17429, .T. ) ;
#27883 = ADVANCED_FACE ( 'NONE', ( #19904 ), #11538, .T. ) ;
#27884 = LINE ( 'NONE', #5805, #19532 ) ;
#27885 = ORIENTED_EDGE ( 'NONE', *, *, #30891, .T. ) ;
#27886 = LINE ( 'NONE', #17422, #20739 ) ;
#27887 = CARTESIAN_POINT ( 'NONE',  ( -35.71762877834949990, -12.58147180936567011, 68.31122994652405112 ) ) ;
#27888 = AXIS2_PLACEMENT_3D ( 'NONE', #20605, #23282, #21127 ) ;
#27889 = VERTEX_POINT ( 'NONE', #19372 ) ;
#27890 = DIRECTION ( 'NONE',  ( -1.000000000000000000, -0.000000000000000000, -0.000000000000000000 ) ) ;
#27891 = CARTESIAN_POINT ( 'NONE',  ( 0.6763010051031080883, -1.505030548027688875, 0.000000000000000000 ) ) ;
#27892 = CYLINDRICAL_SURFACE ( 'NONE', #29701, 34.41491905851385269 ) ;
#27893 = ORIENTED_EDGE ( 'NONE', *, *, #15478, .F. ) ;
#27894 = VECTOR ( 'NONE', #23204, 1000.000000000000000 ) ;
#27895 = DIRECTION ( 'NONE',  ( 0.1063910735369155841, -0.9943243633099125844, -3.335902418025060287E-15 ) ) ;
#27896 = VECTOR ( 'NONE', #25747, 1000.000000000000000 ) ;
#27897 = PRESENTATION_LAYER_ASSIGNMENT (  '', '', ( #9156 ) ) ;
#27898 = CYLINDRICAL_SURFACE ( 'NONE', #26697, 7.999999999999979572 ) ;
#27899 = ADVANCED_FACE ( 'NONE', ( #19551 ), #503, .T. ) ;
#27900 = VERTEX_POINT ( 'NONE', #33584 ) ;
#27901 = DIRECTION ( 'NONE',  ( 0.000000000000000000, 1.374038396813312784E-15, -1.000000000000000000 ) ) ;
#27902 = DIRECTION ( 'NONE',  ( -1.000000000000000000, -0.000000000000000000, -0.000000000000000000 ) ) ;
#27903 = CARTESIAN_POINT ( 'NONE',  ( 105.0000000000000000, 0.000000000000000000, 57.49999999999999289 ) ) ;
#27904 = PLANE ( 'NONE',  #27296 ) ;
#27905 = CONTEXT_DEPENDENT_SHAPE_REPRESENTATION ( #3956, #28514 ) ;
#27906 = ORIENTED_EDGE ( 'NONE', *, *, #16611, .F. ) ;
#27907 = ORIENTED_EDGE ( 'NONE', *, *, #17273, .F. ) ;
#27908 = VERTEX_POINT ( 'NONE', #20080 ) ;
#27909 = VECTOR ( 'NONE', #26600, 1000.000000000000000 ) ;
#27910 = CARTESIAN_POINT ( 'NONE',  ( 0.02407890056655781832, -29.68817180695682723, 9.232883799364120847 ) ) ;
#27911 = EDGE_CURVE ( 'NONE', #28782, #7203, #28158, .T. ) ;
#27913 = AXIS2_PLACEMENT_3D ( 'NONE', #32107, #26769, #13261 ) ;
#27912 = LINE ( 'NONE', #33431, #24514 ) ;
#27914 = ADVANCED_FACE ( 'NONE', ( #25397 ), #30922, .F. ) ;
#27915 = EDGE_CURVE ( 'NONE', #34290, #34864, #32879, .T. ) ;
#27916 = CYLINDRICAL_SURFACE ( 'NONE', #845, 34.41491905851385269 ) ;
#27917 = CARTESIAN_POINT ( 'NONE',  ( -36.04853892210773836, 11.59936550071287797, -29.04209251724896745 ) ) ;
#27918 = ORIENTED_EDGE ( 'NONE', *, *, #18334, .F. ) ;
#27919 = EDGE_LOOP ( 'NONE', ( #20181, #636, #31769, #34503 ) ) ;
#27920 = DIRECTION ( 'NONE',  ( 0.000000000000000000, 0.000000000000000000, 1.000000000000000000 ) ) ;
#27921 = ORIENTED_EDGE ( 'NONE', *, *, #9919, .F. ) ;
#27922 = PRODUCT_DEFINITION_SHAPE ( 'NONE', 'NONE',  #35153 ) ;
#27923 = CARTESIAN_POINT ( 'NONE',  ( -442.0000000000000000, -124.9999999999999716, 135.9999999999999716 ) ) ;
#27924 = DIRECTION ( 'NONE',  ( 0.000000000000000000, 1.000000000000000000, 1.934419779023891545E-16 ) ) ;
#27925 = EDGE_LOOP ( 'NONE', ( #2789, #10349 ) ) ;
#27926 = ORIENTED_EDGE ( 'NONE', *, *, #4836, .T. ) ;
#27927 = PRESENTATION_STYLE_ASSIGNMENT (( #5846 ) ) ;
#27928 = CIRCLE ( 'NONE', #12043, 2.525000000000001243 ) ;
#27929 = AXIS2_PLACEMENT_3D ( 'NONE', #21718, #13893, #24732 ) ;
#27931 = VECTOR ( 'NONE', #25530, 1000.000000000000000 ) ;
#27930 = CARTESIAN_POINT ( 'NONE',  ( 127.4999999999999147, 0.000000000000000000, 12.50000000000000000 ) ) ;
#27932 = ORIENTED_EDGE ( 'NONE', *, *, #17441, .T. ) ;
#27933 = CARTESIAN_POINT ( 'NONE',  ( -42.55956070192386420, -17.65143121711728469, 20.00000000000000000 ) ) ;
#27934 = DIRECTION ( 'NONE',  ( 0.000000000000000000, -2.309213040847544338E-50, -1.000000000000000000 ) ) ;
#27935 = DIRECTION ( 'NONE',  ( -1.292961597001347186E-16, -0.000000000000000000, 1.000000000000000000 ) ) ;
#27936 = CARTESIAN_POINT ( 'NONE',  ( 5.390701026406702567, -37.47456861236018000, -36.68877005347593467 ) ) ;
#27937 = CARTESIAN_POINT ( 'NONE',  ( -106.6595803520255430, -4.849832969747407851, 11.52164913186504869 ) ) ;
#27938 = LINE ( 'NONE', #6571, #33238 ) ;
#27939 = DIRECTION ( 'NONE',  ( 0.000000000000000000, 1.310824597558155437E-49, 1.000000000000000000 ) ) ;
#27940 = ORIENTED_EDGE ( 'NONE', *, *, #232, .T. ) ;
#27941 = VECTOR ( 'NONE', #8872, 1000.000000000000114 ) ;
#27942 = VERTEX_POINT ( 'NONE', #12075 ) ;
#27943 = DIRECTION ( 'NONE',  ( 2.631201909438060269E-14, -5.396010391056495992E-16, 0.9999999999999998890 ) ) ;
#27944 = EDGE_LOOP ( 'NONE', ( #28965, #23490, #25616, #30949 ) ) ;
#27945 = VERTEX_POINT ( 'NONE', #11360 ) ;
#27946 = AXIS2_PLACEMENT_3D ( 'NONE', #6249, #760, #941 ) ;
#27947 = DIRECTION ( 'NONE',  ( 1.000000000000000000, 0.000000000000000000, 0.000000000000000000 ) ) ;
#27948 = VECTOR ( 'NONE', #29678, 1000.000000000000000 ) ;
#27949 = CARTESIAN_POINT ( 'NONE',  ( -442.0000000000000000, -112.9999999999999858, -174.9999999999999716 ) ) ;
#27950 = VECTOR ( 'NONE', #15091, 1000.000000000000000 ) ;
#27951 = ORIENTED_EDGE ( 'NONE', *, *, #27804, .F. ) ;
#27952 = VECTOR ( 'NONE', #34904, 1000.000000000000000 ) ;
#27953 = CARTESIAN_POINT ( 'NONE',  ( -5.021133111224886036, 8.235406450278427215, -67.50000000000000000 ) ) ;
#27954 = CARTESIAN_POINT ( 'NONE',  ( -100.3444248244574908, -2.125365432952321054, -12.31898464336051191 ) ) ;
#27955 = ADVANCED_FACE ( 'NONE', ( #6529 ), #17066, .F. ) ;
#27956 = CONTEXT_DEPENDENT_SHAPE_REPRESENTATION ( #1273, #18713 ) ;
#27957 = EDGE_CURVE ( 'NONE', #20902, #5869, #22742, .T. ) ;
#27959 = CARTESIAN_POINT ( 'NONE',  ( 31.83311414508813897, -6.771795677801486057, 68.31122994652405112 ) ) ;
#27958 = CARTESIAN_POINT ( 'NONE',  ( -6.500000000000000000, 0.000000000000000000, -0.7520000000000001128 ) ) ;
#27960 = ORIENTED_EDGE ( 'NONE', *, *, #10429, .T. ) ;
#27961 = VERTEX_POINT ( 'NONE', #27891 ) ;
#27962 = DIRECTION ( 'NONE',  ( 1.000000000000000000, 0.000000000000000000, -1.848892746611746966E-32 ) ) ;
#27963 = EDGE_CURVE ( 'NONE', #3468, #3784, #852, .T. ) ;
#27964 = CARTESIAN_POINT ( 'NONE',  ( -442.0000000000000000, 137.0000000000000000, -155.0000000000000000 ) ) ;
#27965 = CARTESIAN_POINT ( 'NONE',  ( -418.0000000000000568, -104.9999999999999858, -159.0000000000000000 ) ) ;
#27966 = CYLINDRICAL_SURFACE ( 'NONE', #2473, 3.999999999999989786 ) ;
#27967 = ORIENTED_EDGE ( 'NONE', *, *, #34834, .T. ) ;
#27968 = AXIS2_PLACEMENT_3D ( 'NONE', #19185, #30022, #3136 ) ;
#27969 = DIRECTION ( 'NONE',  ( -0.000000000000000000, -0.000000000000000000, -1.000000000000000000 ) ) ;
#27970 = CARTESIAN_POINT ( 'NONE',  ( 0.000000000000000000, -20.35927063852789232, -24.61013060777193218 ) ) ;
#27971 = VERTEX_POINT ( 'NONE', #14568 ) ;
#27972 = CARTESIAN_POINT ( 'NONE',  ( -45.05956070192387841, -20.15143121711730245, 20.00000000000000000 ) ) ;
#27973 = DIRECTION ( 'NONE',  ( -0.000000000000000000, 1.836970198721029688E-16, -1.000000000000000000 ) ) ;
#27974 = EDGE_CURVE ( 'NONE', #23491, #34313, #14212, .T. ) ;
#27975 = DIRECTION ( 'NONE',  ( 0.000000000000000000, 0.000000000000000000, 1.000000000000000000 ) ) ;
#27978 = CARTESIAN_POINT ( 'NONE',  ( -262.5000000000000000, 0.000000000000000000, 0.000000000000000000 ) ) ;
#27977 = FACE_OUTER_BOUND ( 'NONE', #1133, .T. ) ;
#27976 = CIRCLE ( 'NONE', #25687, 44.99999999999997868 ) ;
#27979 = AXIS2_PLACEMENT_3D ( 'NONE', #9713, #21095, #32122 ) ;
#27980 = CIRCLE ( 'NONE', #17210, 30.47050528711511674 ) ;
#27981 = DIRECTION ( 'NONE',  ( 0.000000000000000000, -0.000000000000000000, 1.000000000000000000 ) ) ;
#27982 = CARTESIAN_POINT ( 'NONE',  ( -6.500000000000000000, 0.000000000000000000, 4.679999999999999716 ) ) ;
#27983 = ORIENTED_EDGE ( 'NONE', *, *, #2127, .F. ) ;
#27984 = CYLINDRICAL_SURFACE ( 'NONE', #23556, 2.524999999999999467 ) ;
#27985 = SURFACE_STYLE_FILL_AREA ( #5903 ) ;
#27986 = ORIENTED_EDGE ( 'NONE', *, *, #2718, .T. ) ;
#27987 = ORIENTED_EDGE ( 'NONE', *, *, #25388, .F. ) ;
#27988 = EDGE_LOOP ( 'NONE', ( #18609, #23395, #12550, #16060 ) ) ;
#27989 = DIRECTION ( 'NONE',  ( 1.000000000000000000, 0.000000000000000000, 0.000000000000000000 ) ) ;
#27990 = EDGE_LOOP ( 'NONE', ( #28617, #19403, #586, #23773 ) ) ;
#27991 = VERTEX_POINT ( 'NONE', #14394 ) ;
#27992 = DIRECTION ( 'NONE',  ( 0.000000000000000000, 0.000000000000000000, 1.000000000000000000 ) ) ;
#27993 = EDGE_CURVE ( 'NONE', #22922, #2593, #15672, .T. ) ;
#27995 = CIRCLE ( 'NONE', #17785, 9.999999999999994671 ) ;
#27994 = CONTEXT_DEPENDENT_SHAPE_REPRESENTATION ( #28089, #22744 ) ;
#27996 = VERTEX_POINT ( 'NONE', #676 ) ;
#27997 = CARTESIAN_POINT ( 'NONE',  ( 15.04122381213380244, 28.86114964982165887, 68.31122994652405112 ) ) ;
#27998 = VECTOR ( 'NONE', #14608, 1000.000000000000000 ) ;
#27999 = DIRECTION ( 'NONE',  ( 0.000000000000000000, 1.000000000000000000, 1.836970198721029688E-16 ) ) ;
#28000 = EDGE_LOOP ( 'NONE', ( #17541, #2551, #23358, #1023 ) ) ;
#28001 = CIRCLE ( 'NONE', #1851, 34.41491905851385269 ) ;
#28002 = ORIENTED_EDGE ( 'NONE', *, *, #4343, .T. ) ;
#28003 = VECTOR ( 'NONE', #15782, 1000.000000000000000 ) ;
#28004 = DIRECTION ( 'NONE',  ( -0.000000000000000000, -0.000000000000000000, -1.000000000000000000 ) ) ;
#28005 = DIRECTION ( 'NONE',  ( -1.000000000000000000, -0.000000000000000000, -0.000000000000000000 ) ) ;
#28006 = ADVANCED_FACE ( 'NONE', ( #25569 ), #8502, .T. ) ;
#28007 = EDGE_CURVE ( 'NONE', #10470, #6402, #14031, .T. ) ;
#28008 = PLANE ( 'NONE',  #14765 ) ;
#28009 = DIRECTION ( 'NONE',  ( 0.000000000000000000, 0.000000000000000000, 1.000000000000000000 ) ) ;
#28010 = DIRECTION ( 'NONE',  ( 1.000000000000000000, -0.000000000000000000, -0.000000000000000000 ) ) ;
#28011 = ORIENTED_EDGE ( 'NONE', *, *, #17426, .F. ) ;
#28012 = DIRECTION ( 'NONE',  ( 3.040835319149746090E-31, 1.000000000000000000, 0.000000000000000000 ) ) ;
#28013 = EDGE_CURVE ( 'NONE', #19775, #2856, #28949, .T. ) ;
#28014 = EDGE_CURVE ( 'NONE', #10479, #27216, #23612, .T. ) ;
#28015 = DIRECTION ( 'NONE',  ( 0.000000000000000000, -1.000000000000000000, 0.000000000000000000 ) ) ;
#28016 =( BOUNDED_CURVE ( )  B_SPLINE_CURVE ( 3, ( #16903, #24181, #35059, #21527 ),
 .UNSPECIFIED., .F., .F. ) 
 B_SPLINE_CURVE_WITH_KNOTS ( ( 4, 4 ),
 ( 4.340081192300065283, 4.340194262747512965 ),
 .UNSPECIFIED. ) 
 CURVE ( )  GEOMETRIC_REPRESENTATION_ITEM ( )  RATIONAL_B_SPLINE_CURVE ( ( 1.000000000000000000, 0.9999999989345893514, 0.9999999989345893514, 1.000000000000000000 ) ) 
 REPRESENTATION_ITEM ( '' )  );
#28017 = EDGE_LOOP ( 'NONE', ( #1115, #27176, #26242, #9692 ) ) ;
#28018 = DIRECTION ( 'NONE',  ( -0.6051742151937663516, -0.7960930657056428661, -1.462399237109728568E-16 ) ) ;
#28019 = CYLINDRICAL_SURFACE ( 'NONE', #23996, 2.525000000000001243 ) ;
#28020 = DIRECTION ( 'NONE',  ( 0.000000000000000000, 0.000000000000000000, 1.000000000000000000 ) ) ;
#28021 = ADVANCED_FACE ( 'NONE', ( #22916 ), #20425, .F. ) ;
#28022 = DIRECTION ( 'NONE',  ( 0.000000000000000000, 0.000000000000000000, 1.000000000000000000 ) ) ;
#28023 = DIRECTION ( 'NONE',  ( 0.000000000000000000, 0.000000000000000000, -1.000000000000000000 ) ) ;
#28024 = DIRECTION ( 'NONE',  ( 0.000000000000000000, 1.224646799147353207E-16, -1.000000000000000000 ) ) ;
#28025 = VERTEX_POINT ( 'NONE', #34289 ) ;
#28026 = CARTESIAN_POINT ( 'NONE',  ( 53.89849999999999852, 0.000000000000000000, 0.000000000000000000 ) ) ;
#28028 = FACE_OUTER_BOUND ( 'NONE', #25353, .T. ) ;
#28027 = LINE ( 'NONE', #14163, #158 ) ;
#28029 = EDGE_CURVE ( 'NONE', #16015, #16248, #15613, .T. ) ;
#28031 = VERTEX_POINT ( 'NONE', #23101 ) ;
#28030 = VECTOR ( 'NONE', #4193, 1000.000000000000000 ) ;
#28032 = CIRCLE ( 'NONE', #21771, 10.00000000000000000 ) ;
#28033 = AXIS2_PLACEMENT_3D ( 'NONE', #33180, #3972, #9332 ) ;
#28034 = CARTESIAN_POINT ( 'NONE',  ( -15.99999999999998579, -124.9999999999999432, -162.9999999999999432 ) ) ;
#28035 = VERTEX_POINT ( 'NONE', #15266 ) ;
#28036 = ORIENTED_EDGE ( 'NONE', *, *, #7901, .F. ) ;
#28037 = VERTEX_POINT ( 'NONE', #1888 ) ;
#28038 = LINE ( 'NONE', #23752, #3713 ) ;
#28039 = ORIENTED_EDGE ( 'NONE', *, *, #27631, .F. ) ;
#28040 = ORIENTED_EDGE ( 'NONE', *, *, #3989, .T. ) ;
#28041 = DIRECTION ( 'NONE',  ( 0.000000000000000000, 0.000000000000000000, 1.000000000000000000 ) ) ;
#28042 = FACE_OUTER_BOUND ( 'NONE', #25847, .T. ) ;
#28043 = VECTOR ( 'NONE', #17889, 1000.000000000000000 ) ;
#28044 = CARTESIAN_POINT ( 'NONE',  ( -499.9999999999999432, 112.9999999999999574, 162.9999999999999716 ) ) ;
#28045 = DIRECTION ( 'NONE',  ( 0.000000000000000000, 1.000000000000000000, 0.000000000000000000 ) ) ;
#28046 = ORIENTED_EDGE ( 'NONE', *, *, #34382, .F. ) ;
#28047 = ORIENTED_EDGE ( 'NONE', *, *, #14148, .T. ) ;
#28048 = LINE ( 'NONE', #33211, #7116 ) ;
#28049 = DIRECTION ( 'NONE',  ( 0.000000000000000000, 0.000000000000000000, 1.000000000000000000 ) ) ;
#28050 = DIRECTION ( 'NONE',  ( -1.000000000000000000, -0.000000000000000000, -0.000000000000000000 ) ) ;
#28051 = DIRECTION ( 'NONE',  ( 0.000000000000000000, -1.000000000000000000, -2.465190328815662439E-32 ) ) ;
#28052 = CARTESIAN_POINT ( 'NONE',  ( 15.99999999999997868, 144.9999999999999716, 187.0000000000000000 ) ) ;
#28053 = AXIS2_PLACEMENT_3D ( 'NONE', #8680, #30401, #16896 ) ;
#28054 = DIRECTION ( 'NONE',  ( -1.000000000000000000, 0.000000000000000000, -5.546364386991661285E-52 ) ) ;
#28055 = VECTOR ( 'NONE', #8619, 1000.000000000000000 ) ;
#28056 = ADVANCED_FACE ( 'NONE', ( #31440 ), #22474, .T. ) ;
#28057 = EDGE_CURVE ( 'NONE', #2660, #13396, #7222, .T. ) ;
#28058 = VECTOR ( 'NONE', #27405, 1000.000000000000000 ) ;
#28059 = DIRECTION ( 'NONE',  ( -1.848892746611746419E-32, -6.842277657836020854E-49, 1.000000000000000000 ) ) ;
#28060 = ORIENTED_EDGE ( 'NONE', *, *, #24788, .F. ) ;
#28061 = CARTESIAN_POINT ( 'NONE',  ( 2.789999999999999147, 14.63235270440974922, -27.43224275967423509 ) ) ;
#28062 = LINE ( 'NONE', #31093, #13759 ) ;
#28063 = DIRECTION ( 'NONE',  ( -0.1081190184239420177, -0.9941379571543595972, 0.000000000000000000 ) ) ;
#28064 = ORIENTED_EDGE ( 'NONE', *, *, #20693, .T. ) ;
#28065 = CARTESIAN_POINT ( 'NONE',  ( 32.81769769215652133, 18.87860345536237006, 68.31122994652405112 ) ) ;
#28066 = EDGE_LOOP ( 'NONE', ( #25347, #9779, #7134, #3005 ) ) ;
#28067 = CARTESIAN_POINT ( 'NONE',  ( -102.7226881718362392, 4.592153980832016202, 11.62674774045203385 ) ) ;
#28068 = EDGE_CURVE ( 'NONE', #14836, #1154, #24739, .T. ) ;
#28069 = AXIS2_PLACEMENT_3D ( 'NONE', #11193, #5644, #5299 ) ;
#28070 = ORIENTED_EDGE ( 'NONE', *, *, #22490, .T. ) ;
#28071 = CARTESIAN_POINT ( 'NONE',  ( 2.261199741936142704, 14.91106968280055156, 29.87539438830526706 ) ) ;
#28072 = CARTESIAN_POINT ( 'NONE',  ( 10.17231796313409298, 6.310691531022071921, -87.50000000000000000 ) ) ;
#28073 = CARTESIAN_POINT ( 'NONE',  ( -500.0000000000000000, -113.0000000000000000, -155.0000000000000000 ) ) ;
#28074 = EDGE_CURVE ( 'NONE', #15074, #16015, #34108, .T. ) ;
#28075 = ORIENTED_EDGE ( 'NONE', *, *, #14777, .T. ) ;
#28076 = EDGE_CURVE ( 'NONE', #14266, #18467, #1718, .T. ) ;
#28077 = AXIS2_PLACEMENT_3D ( 'NONE', #4723, #12949, #12774 ) ;
#28078 = EDGE_CURVE ( 'NONE', #19079, #7089, #9192, .T. ) ;
#28079 = AXIS2_PLACEMENT_3D ( 'NONE', #3769, #3933, #22820 ) ;
#28080 = DIRECTION ( 'NONE',  ( -0.4942497486739246271, -0.8693199560206600340, -1.920742770896671076E-14 ) ) ;
#28081 = TOROIDAL_SURFACE ( 'NONE', #5907, 30.47050528711512030, 8.000000000000000000 ) ;
#28082 = CARTESIAN_POINT ( 'NONE',  ( -9.978866888775733912, -13.65249191622732816, -67.50000000000000000 ) ) ;
#28083 = ORIENTED_EDGE ( 'NONE', *, *, #26217, .F. ) ;
#28084 = CARTESIAN_POINT ( 'NONE',  ( -99.88497961182919482, -2.585407550593147656E-15, 7.500000000000000000 ) ) ;
#28085 = EDGE_CURVE ( 'NONE', #8194, #9865, #8303, .T. ) ;
#28086 = CARTESIAN_POINT ( 'NONE',  ( 31.83311414508813897, -6.771795677801482505, 49.43553178847298568 ) ) ;
#28087 = CARTESIAN_POINT ( 'NONE',  ( 3.235562306570555532E-30, 1.325223266901699007E-14, -67.50000000000000000 ) ) ;
#28088 = ORIENTED_EDGE ( 'NONE', *, *, #4096, .F. ) ;
#28090 = EDGE_LOOP ( 'NONE', ( #18949, #24236, #18675, #34731 ) ) ;
#28089 =( REPRESENTATION_RELATIONSHIP ('NONE','NONE', #23037, #28231 ) REPRESENTATION_RELATIONSHIP_WITH_TRANSFORMATION ( #25139 )SHAPE_REPRESENTATION_RELATIONSHIP( ) );
#28091 = VERTEX_POINT ( 'NONE', #9395 ) ;
#28092 = CARTESIAN_POINT ( 'NONE',  ( -117.4999999999997442, 0.000000000000000000, 0.000000000000000000 ) ) ;
#28093 = DIRECTION ( 'NONE',  ( 0.000000000000000000, 0.000000000000000000, -1.000000000000000000 ) ) ;
#28094 = DIRECTION ( 'NONE',  ( -1.000000000000000000, 0.000000000000000000, -1.300283923313630633E-47 ) ) ;
#28095 = DIRECTION ( 'NONE',  ( 0.9868265225415266961, 0.1617819965527614590, 2.971887063570111902E-17 ) ) ;
#28096 = ORIENTED_EDGE ( 'NONE', *, *, #16383, .F. ) ;
#28097 = VERTEX_POINT ( 'NONE', #20767 ) ;
#28098 = ADVANCED_FACE ( 'NONE', ( #25934 ), #1551, .F. ) ;
#28099 = DIRECTION ( 'NONE',  ( 0.000000000000000000, 1.836970198721029441E-16, -1.000000000000000000 ) ) ;
#28100 = DIRECTION ( 'NONE',  ( -0.000000000000000000, 1.836970198721029934E-16, -1.000000000000000000 ) ) ;
#28101 = ORIENTED_EDGE ( 'NONE', *, *, #18501, .T. ) ;
#28102 = VECTOR ( 'NONE', #22631, 1000.000000000000000 ) ;
#28103 = DIRECTION ( 'NONE',  ( -0.000000000000000000, -1.000000000000000000, -0.000000000000000000 ) ) ;
#28104 = CARTESIAN_POINT ( 'NONE',  ( 108.7927201099689682, 4.321688686550378300, 11.73238900788529726 ) ) ;
#28105 = ORIENTED_EDGE ( 'NONE', *, *, #3009, .F. ) ;
#28106 = VERTEX_POINT ( 'NONE', #7349 ) ;
#28107 = EDGE_LOOP ( 'NONE', ( #3951, #33681, #31167, #2580 ) ) ;
#28108 = LINE ( 'NONE', #19404, #28274 ) ;
#28109 = VECTOR ( 'NONE', #17330, 1000.000000000000000 ) ;
#28110 = DIRECTION ( 'NONE',  ( 0.000000000000000000, -1.000000000000000000, -5.053935297177146739E-49 ) ) ;
#28111 = ORIENTED_EDGE ( 'NONE', *, *, #35020, .T. ) ;
#28112 = DIRECTION ( 'NONE',  ( 0.2675283385292215321, 0.9635499925192227977, 0.000000000000000000 ) ) ;
#28114 = AXIS2_PLACEMENT_3D ( 'NONE', #14667, #30671, #8769 ) ;
#28113 =( NAMED_UNIT ( * ) PLANE_ANGLE_UNIT ( ) SI_UNIT ( $, .RADIAN. ) );
#28115 = CYLINDRICAL_SURFACE ( 'NONE', #21799, 16.19999999999999574 ) ;
#28116 = CARTESIAN_POINT ( 'NONE',  ( -102.7238790343726009, -4.592825538643425354, 11.62648616087115805 ) ) ;
#28117 = DIRECTION ( 'NONE',  ( 0.000000000000000000, -0.2486898871648554887, 0.9685831611286309650 ) ) ;
#28118 = DIRECTION ( 'NONE',  ( -1.000000000000000000, -3.040835319149746090E-31, 1.232595164407830946E-32 ) ) ;
#28119 = VERTEX_POINT ( 'NONE', #18125 ) ;
#28120 = EDGE_CURVE ( 'NONE', #25488, #8590, #6702, .T. ) ;
#28121 = EDGE_CURVE ( 'NONE', #33855, #23099, #17743, .T. ) ;
#28122 = AXIS2_PLACEMENT_3D ( 'NONE', #25673, #34211, #22839 ) ;
#28123 = EDGE_LOOP ( 'NONE', ( #9236, #17043, #7065, #29690 ) ) ;
#28124 = DIRECTION ( 'NONE',  ( 0.1063910735368947813, -0.9943243633099144718, -3.335902418024520312E-15 ) ) ;
#28125 = VERTEX_POINT ( 'NONE', #28430 ) ;
#28126 = AXIS2_PLACEMENT_3D ( 'NONE', #17972, #31464, #34129 ) ;
#28127 = ORIENTED_EDGE ( 'NONE', *, *, #17635, .F. ) ;
#28128 = CARTESIAN_POINT ( 'NONE',  ( 11.99999999999999645, 134.9999999999998863, 155.0000000000000000 ) ) ;
#28129 = CARTESIAN_POINT ( 'NONE',  ( -143.0000000000000568, -97.56119630548165844, -180.0000000000000000 ) ) ;
#28130 = CIRCLE ( 'NONE', #33821, 7.999999999999979572 ) ;
#28131 = LINE ( 'NONE', #14628, #18203 ) ;
#28132 = CONTEXT_DEPENDENT_SHAPE_REPRESENTATION ( #16941, #20036 ) ;
#28133 = CIRCLE ( 'NONE', #16211, 7.500000000000000000 ) ;
#28134 = VERTEX_POINT ( 'NONE', #14917 ) ;
#28135 = PRODUCT_DEFINITION_SHAPE ( 'NONE', 'NONE',  #35215 ) ;
#28136 = CARTESIAN_POINT ( 'NONE',  ( -499.9999999999999432, 104.9999999999999858, -162.9999999999999716 ) ) ;
#28137 = CARTESIAN_POINT ( 'NONE',  ( -107.5740425955733741, -4.432593925698495418, -11.68934397677214498 ) ) ;
#28139 = FACE_OUTER_BOUND ( 'NONE', #13226, .T. ) ;
#28138 = DIRECTION ( 'NONE',  ( 1.000000000000000000, 3.040835319149746528E-31, 1.232595164407830946E-32 ) ) ;
#28140 = EDGE_LOOP ( 'NONE', ( #3608, #8320, #32136, #6262 ) ) ;
#28141 = ORIENTED_EDGE ( 'NONE', *, *, #19989, .F. ) ;
#28142 = LINE ( 'NONE', #14637, #11751 ) ;
#28143 = CYLINDRICAL_SURFACE ( 'NONE', #25562, 3.999999999999976019 ) ;
#28144 = DIRECTION ( 'NONE',  ( 1.000000000000000000, 0.000000000000000000, 0.000000000000000000 ) ) ;
#28145 = CARTESIAN_POINT ( 'NONE',  ( -27.76765758629847269, -16.97532223688794417, 68.31122994652405112 ) ) ;
#28146 = ORIENTED_EDGE ( 'NONE', *, *, #33067, .T. ) ;
#28147 = DIRECTION ( 'NONE',  ( 0.000000000000000000, 0.8443279255020087470, 0.5358267949790064266 ) ) ;
#28148 = VECTOR ( 'NONE', #5172, 1000.000000000000000 ) ;
#28149 = DIRECTION ( 'NONE',  ( 0.000000000000000000, 1.836970198721029688E-16, -1.000000000000000000 ) ) ;
#28150 = VECTOR ( 'NONE', #18109, 1000.000000000000000 ) ;
#28151 = ORIENTED_EDGE ( 'NONE', *, *, #13776, .T. ) ;
#28152 = AXIS2_PLACEMENT_3D ( 'NONE', #19710, #30728, #30558 ) ;
#28153 = CARTESIAN_POINT ( 'NONE',  ( 11.99999999999999645, 124.9999999999999716, 194.9999999999999716 ) ) ;
#28154 = DIRECTION ( 'NONE',  ( 0.000000000000000000, 0.000000000000000000, -1.000000000000000000 ) ) ;
#28155 = LINE ( 'NONE', #3409, #24026 ) ;
#28157 = LINE ( 'NONE', #14820, #6580 ) ;
#28156 = DIRECTION ( 'NONE',  ( 0.000000000000000000, 1.836970198721029441E-16, -1.000000000000000000 ) ) ;
#28158 = CIRCLE ( 'NONE', #27591, 2.036051781435508801 ) ;
#28159 = CARTESIAN_POINT ( 'NONE',  ( 0.02407890056655651728, 11.80989368511502846, -28.76039115933972923 ) ) ;
#28161 = AXIS2_PLACEMENT_3D ( 'NONE', #20046, #14359, #6307 ) ;
#28160 = DIRECTION ( 'NONE',  ( -1.000000000000000000, 0.000000000000000000, 0.000000000000000000 ) ) ;
#28162 = ORIENTED_EDGE ( 'NONE', *, *, #8436, .F. ) ;
#28163 = CARTESIAN_POINT ( 'NONE',  ( 2.606461941304143881, -8.814691041839068930, -31.04399216667579964 ) ) ;
#28164 = CARTESIAN_POINT ( 'NONE',  ( 60.00000000000000000, 33.69708579775584667, 49.43553178847298568 ) ) ;
#28165 = AXIS2_PLACEMENT_3D ( 'NONE', #15740, #12370, #12533 ) ;
#28166 = EDGE_CURVE ( 'NONE', #21633, #6559, #25753, .T. ) ;
#28167 = ADVANCED_FACE ( 'NONE', ( #20596 ), #2415, .F. ) ;
#28168 = EDGE_CURVE ( 'NONE', #2456, #23263, #10456, .T. ) ;
#28169 = EDGE_LOOP ( 'NONE', ( #24996, #5697, #21097, #9827, #20640, #30861, #32346, #24400 ) ) ;
#28170 = ADVANCED_FACE ( 'NONE', ( #13632 ), #21469, .T. ) ;
#28171 = ORIENTED_EDGE ( 'NONE', *, *, #23202, .T. ) ;
#28172 = CIRCLE ( 'NONE', #3161, 32.54542015209054995 ) ;
#28173 = VERTEX_POINT ( 'NONE', #8285 ) ;
#28174 = DIRECTION ( 'NONE',  ( 0.000000000000000000, 0.000000000000000000, 1.000000000000000000 ) ) ;
#28175 = VERTEX_POINT ( 'NONE', #16141 ) ;
#28176 = VERTEX_POINT ( 'NONE', #21634 ) ;
#28177 = CARTESIAN_POINT ( 'NONE',  ( -430.0000000000000000, -119.0000000000000000, 130.0000000000000000 ) ) ;
#28178 = AXIS2_PLACEMENT_3D ( 'NONE', #16650, #27833, #22150 ) ;
#28179 = ITEM_DEFINED_TRANSFORMATION ( 'NONE', 'NONE', #18414,  #28566 ) ;
#28180 = EDGE_LOOP ( 'NONE', ( #2114, #24039, #32355, #4389, #22416, #7454, #25593, #16171 ) ) ;
#28181 = PLANE ( 'NONE',  #14095 ) ;
#28182 = PLANE ( 'NONE',  #29643 ) ;
#28183 = ORIENTED_EDGE ( 'NONE', *, *, #22982, .F. ) ;
#28184 = ORIENTED_EDGE ( 'NONE', *, *, #9241, .F. ) ;
#28185 = DIRECTION ( 'NONE',  ( 0.000000000000000000, 0.000000000000000000, -1.000000000000000000 ) ) ;
#28186 = DIRECTION ( 'NONE',  ( -1.000000000000000000, 0.000000000000000000, -0.000000000000000000 ) ) ;
#28188 = VECTOR ( 'NONE', #31519, 1000.000000000000000 ) ;
#28187 = B_SPLINE_CURVE_WITH_KNOTS ( 'NONE', 3,
 ( #5506, #14072, #24382, #9 ),
 .UNSPECIFIED., .F., .F.,
 ( 4, 4 ),
 ( 2.075676022607228905E-07, 0.0006879433439099471746 ),
 .UNSPECIFIED. ) ;
#28189 = CARTESIAN_POINT ( 'NONE',  ( 0.02407890056655738464, -29.68817180695669578, -9.232883799364548949 ) ) ;
#28190 = CARTESIAN_POINT ( 'NONE',  ( 10.00000000000000000, 15.58845726811990495, 0.000000000000000000 ) ) ;
#28191 = PLANE ( 'NONE',  #30760 ) ;
#28192 = ORIENTED_EDGE ( 'NONE', *, *, #21608, .T. ) ;
#28193 = CARTESIAN_POINT ( 'NONE',  ( 143.0000000000000568, -89.01471862576147487, 43.40376782973931569 ) ) ;
#28194 = DIRECTION ( 'NONE',  ( -1.000000000000000000, 0.000000000000000000, 0.000000000000000000 ) ) ;
#28195 = EDGE_LOOP ( 'NONE', ( #17381, #23704, #7994, #29823 ) ) ;
#28196 = LINE ( 'NONE', #14692, #33280 ) ;
#28197 = CARTESIAN_POINT ( 'NONE',  ( 0.0001801434340936737804, -25.83993731729792742, -16.24881338200996694 ) ) ;
#28198 = CARTESIAN_POINT ( 'NONE',  ( -37.85301660235036536, 0.7430237821112765095, -36.68877005347593467 ) ) ;
#28199 = DIRECTION ( 'NONE',  ( 0.000000000000000000, 0.000000000000000000, -1.000000000000000000 ) ) ;
#28200 = CARTESIAN_POINT ( 'NONE',  ( 127.4999999999999147, 0.000000000000000000, 0.000000000000000000 ) ) ;
#28201 = AXIS2_PLACEMENT_3D ( 'NONE', #9132, #12180, #17696 ) ;
#28202 = EDGE_CURVE ( 'NONE', #26104, #5255, #14701, .T. ) ;
#28203 = CARTESIAN_POINT ( 'NONE',  ( 5.021133111224162171, -21.54630831098063837, -67.50000000000000000 ) ) ;
#28204 = VERTEX_POINT ( 'NONE', #27317 ) ;
#28205 = DIRECTION ( 'NONE',  ( -0.000000000000000000, -1.836970198721029688E-16, 1.000000000000000000 ) ) ;
#28207 = CARTESIAN_POINT ( 'NONE',  ( -117.4999999999997442, 0.000000000000000000, 0.000000000000000000 ) ) ;
#28206 = CARTESIAN_POINT ( 'NONE',  ( -349.0000000000000000, -125.0000000000000284, 126.0000000000000000 ) ) ;
#28208 = AXIS2_PLACEMENT_3D ( 'NONE', #11794, #23640, #30650 ) ;
#28209 = EDGE_CURVE ( 'NONE', #30170, #18484, #23946, .T. ) ;
#28210 = ORIENTED_EDGE ( 'NONE', *, *, #29134, .F. ) ;
#28211 = FACE_OUTER_BOUND ( 'NONE', #17339, .T. ) ;
#28212 = ADVANCED_FACE ( 'NONE', ( #18639 ), #21111, .F. ) ;
#28213 = AXIS2_PLACEMENT_3D ( 'NONE', #29300, #15260, #17941 ) ;
#28214 = ORIENTED_EDGE ( 'NONE', *, *, #12067, .T. ) ;
#28215 = ORIENTED_EDGE ( 'NONE', *, *, #7303, .F. ) ;
#28216 = EDGE_CURVE ( 'NONE', #10965, #27900, #33621, .T. ) ;
#28217 = ORIENTED_EDGE ( 'NONE', *, *, #21645, .T. ) ;
#28218 = CARTESIAN_POINT ( 'NONE',  ( 101.5039560588549676, -4.564063043377788453, -5.956988494001920209 ) ) ;
#28219 = ORIENTED_EDGE ( 'NONE', *, *, #20341, .T. ) ;
#28220 = VERTEX_POINT ( 'NONE', #99 ) ;
#28221 = DIRECTION ( 'NONE',  ( 0.000000000000000000, 0.000000000000000000, 1.000000000000000000 ) ) ;
#28222 = PRODUCT_DEFINITION_SHAPE ( 'NONE', 'NONE',  #35145 ) ;
#28223 = EDGE_CURVE ( 'NONE', #6836, #14097, #31902, .T. ) ;
#28224 = EDGE_CURVE ( 'NONE', #1565, #4220, #26802, .T. ) ;
#28225 = CARTESIAN_POINT ( 'NONE',  ( 1.040000000000000702, -10.89151784028311809, 32.64600270996213283 ) ) ;
#28226 = VECTOR ( 'NONE', #9627, 1000.000000000000000 ) ;
#28227 = CARTESIAN_POINT ( 'NONE',  ( -442.0000000000000000, -104.9999999999999858, -162.9999999999999716 ) ) ;
#28228 = PLANE ( 'NONE',  #24490 ) ;
#28229 = ORIENTED_EDGE ( 'NONE', *, *, #15594, .T. ) ;
#28230 = ORIENTED_EDGE ( 'NONE', *, *, #19838, .F. ) ;
#28231 = SHAPE_REPRESENTATION ( 'chainlinkage', ( #28566 ), #6416 ) ;
#28232 = DIRECTION ( 'NONE',  ( -1.000000000000000000, 0.000000000000000000, 0.000000000000000000 ) ) ;
#28233 = CARTESIAN_POINT ( 'NONE',  ( -10.00000000000000000, 0.000000000000000000, 0.000000000000000000 ) ) ;
#28234 = LINE ( 'NONE', #30369, #12946 ) ;
#28235 = AXIS2_PLACEMENT_3D ( 'NONE', #15249, #26257, #9378 ) ;
#28236 = DIRECTION ( 'NONE',  ( -0.000000000000000000, 0.000000000000000000, 1.000000000000000000 ) ) ;
#28237 = DIRECTION ( 'NONE',  ( 0.000000000000000000, 0.000000000000000000, 1.000000000000000000 ) ) ;
#28238 = CARTESIAN_POINT ( 'NONE',  ( 0.02407890056655825201, -3.506335382740311868, -30.89238256715869468 ) ) ;
#28239 = DIRECTION ( 'NONE',  ( -1.000000000000000000, 0.000000000000000000, -0.000000000000000000 ) ) ;
#28240 = VERTEX_POINT ( 'NONE', #21292 ) ;
#28241 = PRESENTATION_LAYER_ASSIGNMENT (  '', '', ( #7178 ) ) ;
#28242 = FACE_OUTER_BOUND ( 'NONE', #4580, .T. ) ;
#28243 = CARTESIAN_POINT ( 'NONE',  ( 21.85761591200894216, 30.91355005303806180, 49.43553178847298568 ) ) ;
#28244 = DIRECTION ( 'NONE',  ( -0.000000000000000000, -0.000000000000000000, -1.000000000000000000 ) ) ;
#28245 = ORIENTED_EDGE ( 'NONE', *, *, #3463, .F. ) ;
#28246 = LINE ( 'NONE', #22561, #16100 ) ;
#28247 = ORIENTED_EDGE ( 'NONE', *, *, #28761, .F. ) ;
#28248 = DIRECTION ( 'NONE',  ( 0.000000000000000000, 1.836970198721029688E-16, -1.000000000000000000 ) ) ;
#28249 = CARTESIAN_POINT ( 'NONE',  ( -99.91893143628131213, 0.6776097359754149618, 12.48599830169775693 ) ) ;
#28250 = AXIS2_PLACEMENT_3D ( 'NONE', #9104, #14464, #8748 ) ;
#28251 = AXIS2_PLACEMENT_3D ( 'NONE', #26513, #2135, #7641 ) ;
#28252 = ORIENTED_EDGE ( 'NONE', *, *, #5632, .F. ) ;
#28253 = DIRECTION ( 'NONE',  ( -0.000000000000000000, -0.000000000000000000, -1.000000000000000000 ) ) ;
#28254 = DIRECTION ( 'NONE',  ( 0.000000000000000000, 1.836970198721029441E-16, -1.000000000000000000 ) ) ;
#28255 = PLANE ( 'NONE',  #29118 ) ;
#28256 = EDGE_CURVE ( 'NONE', #4555, #4220, #5427, .T. ) ;
#28257 = ORIENTED_EDGE ( 'NONE', *, *, #22152, .T. ) ;
#28258 = EDGE_CURVE ( 'NONE', #21475, #9815, #27148, .T. ) ;
#28259 = ADVANCED_FACE ( 'NONE', ( #18463 ), #29308, .T. ) ;
#28260 = DIRECTION ( 'NONE',  ( -0.7924409893660955273, 0.6099485866632401443, -2.785165617058316951E-14 ) ) ;
#28261 = AXIS2_PLACEMENT_3D ( 'NONE', #34479, #20953, #31797 ) ;
#28262 = CARTESIAN_POINT ( 'NONE',  ( 2.765921099433442443, -30.46391896562403190, -6.211548095912885259 ) ) ;
#28263 = ORIENTED_EDGE ( 'NONE', *, *, #24146, .F. ) ;
#28264 = DIRECTION ( 'NONE',  ( -1.000000000000000000, 0.000000000000000000, -0.000000000000000000 ) ) ;
#28265 = FACE_OUTER_BOUND ( 'NONE', #3250, .T. ) ;
#28266 = CARTESIAN_POINT ( 'NONE',  ( 0.02407890056655608360, 14.63235270440974922, -27.43224275967423509 ) ) ;
#28267 = FACE_OUTER_BOUND ( 'NONE', #29570, .T. ) ;
#28268 = ITEM_DEFINED_TRANSFORMATION ( 'NONE', 'NONE', #4703,  #28566 ) ;
#28269 = EDGE_LOOP ( 'NONE', ( #299, #9198, #14988, #6705 ) ) ;
#28270 = ORIENTED_EDGE ( 'NONE', *, *, #28660, .T. ) ;
#28271 = VERTEX_POINT ( 'NONE', #26624 ) ;
#28272 = PRODUCT_DEFINITION_SHAPE ( 'NONE', 'NONE',  #35096 ) ;
#28273 = CARTESIAN_POINT ( 'NONE',  ( -442.0000000000000000, 105.0000000000000142, -175.0000000000000000 ) ) ;
#28274 = VECTOR ( 'NONE', #17460, 1000.000000000000000 ) ;
#28275 = ADVANCED_FACE ( 'NONE', ( #7751 ), #29481, .T. ) ;
#28276 = CARTESIAN_POINT ( 'NONE',  ( 44.94043929807611448, -32.65143121711728469, 0.000000000000000000 ) ) ;
#28277 = AXIS2_PLACEMENT_3D ( 'NONE', #7329, #18224, #29054 ) ;
#28278 = AXIS2_PLACEMENT_3D ( 'NONE', #34945, #7693, #29243 ) ;
#28279 = CARTESIAN_POINT ( 'NONE',  ( -12.00000000000001066, -145.0000000000000000, 159.0000000000000000 ) ) ;
#28280 = CARTESIAN_POINT ( 'NONE',  ( 2.765921099433441110, 11.80989368511462523, 28.76039115933989976 ) ) ;
#28281 = ORIENTED_EDGE ( 'NONE', *, *, #13293, .T. ) ;
#28282 = CARTESIAN_POINT ( 'NONE',  ( 1.040000000000000924, 0.000000000000000000, 0.000000000000000000 ) ) ;
#28283 = DIRECTION ( 'NONE',  ( 0.000000000000000000, -1.131431318426415506E-52, -1.000000000000000000 ) ) ;
#28284 = ORIENTED_EDGE ( 'NONE', *, *, #8908, .F. ) ;
#28285 = ADVANCED_FACE ( 'NONE', ( #24119 ), #18804, .F. ) ;
#28286 = CARTESIAN_POINT ( 'NONE',  ( -499.9999999999999432, 136.9999999999999432, -190.9999999999999716 ) ) ;
#28287 = CARTESIAN_POINT ( 'NONE',  ( 106.5040302774077361, 5.540701522433002957, 11.20510851329258983 ) ) ;
#28288 = VECTOR ( 'NONE', #6146, 1000.000000000000000 ) ;
#28290 = EDGE_CURVE ( 'NONE', #32869, #19981, #25354, .T. ) ;
#28289 = ORIENTED_EDGE ( 'NONE', *, *, #12272, .T. ) ;
#28291 = FILL_AREA_STYLE_COLOUR ( '', #12350 ) ;
#28292 = ADVANCED_FACE ( 'NONE', ( #3113 ), #3635, .F. ) ;
#28293 = CIRCLE ( 'NONE', #32726, 3.999999999999976019 ) ;
#28294 = DIRECTION ( 'NONE',  ( 0.000000000000000000, 1.310824597558155437E-49, 1.000000000000000000 ) ) ;
#28295 = ORIENTED_EDGE ( 'NONE', *, *, #4836, .F. ) ;
#28296 = CARTESIAN_POINT ( 'NONE',  ( -36.80830595996284416, 8.862931941313773265, 68.31122994652405112 ) ) ;
#28297 = EDGE_CURVE ( 'NONE', #20392, #23064, #6129, .T. ) ;
#28298 = DIRECTION ( 'NONE',  ( 0.000000000000000000, 1.836970198721029441E-16, -1.000000000000000000 ) ) ;
#28299 = AXIS2_PLACEMENT_3D ( 'NONE', #20232, #30724, #33740 ) ;
#28300 = CARTESIAN_POINT ( 'NONE',  ( -110.0732068518744597, -0.6743631657302426863, 12.48293875069316350 ) ) ;
#28301 = SURFACE_SIDE_STYLE ('',( #12462 ) ) ;
#28302 = ORIENTED_EDGE ( 'NONE', *, *, #23338, .T. ) ;
#28303 = VECTOR ( 'NONE', #10838, 1000.000000000000000 ) ;
#28304 = VECTOR ( 'NONE', #18190, 1000.000000000000000 ) ;
#28305 = ORIENTED_EDGE ( 'NONE', *, *, #16602, .F. ) ;
#28306 = EDGE_CURVE ( 'NONE', #31368, #32385, #11491, .T. ) ;
#28307 = ADVANCED_FACE ( 'NONE', ( #986 ), #19331, .F. ) ;
#28308 = DIRECTION ( 'NONE',  ( -7.893605728314050488E-14, 1.618803117314786135E-15, 0.9999999999999998890 ) ) ;
#28309 =( REPRESENTATION_RELATIONSHIP ('NONE','NONE', #23037, #28231 ) REPRESENTATION_RELATIONSHIP_WITH_TRANSFORMATION ( #19473 )SHAPE_REPRESENTATION_RELATIONSHIP( ) );
#28310 = VERTEX_POINT ( 'NONE', #629 ) ;
#28311 = VECTOR ( 'NONE', #10404, 1000.000000000000000 ) ;
#28312 = CARTESIAN_POINT ( 'NONE',  ( -12.00000000000001066, -124.9999999999999432, -154.9999999999999716 ) ) ;
#28313 = CARTESIAN_POINT ( 'NONE',  ( -15.00000000000000000, 0.000000000000000000, 0.000000000000000000 ) ) ;
#28314 = ITEM_DEFINED_TRANSFORMATION ( 'NONE', 'NONE', #16099,  #28566 ) ;
#28315 = ORIENTED_EDGE ( 'NONE', *, *, #3893, .T. ) ;
#28316 = CARTESIAN_POINT ( 'NONE',  ( 0.02407890056655738464, 24.20451283648857554, -19.51346322004903300 ) ) ;
#28317 = CARTESIAN_POINT ( 'NONE',  ( -108.1252680363369336, -4.062792622693889300, -11.82295934283893146 ) ) ;
#28319 = CARTESIAN_POINT ( 'NONE',  ( 2.789999999999999147, -30.43331811787861341, 0.6209492052231032622 ) ) ;
#28318 = DIRECTION ( 'NONE',  ( -1.000000000000000000, 0.000000000000000000, 0.000000000000000000 ) ) ;
#28320 = AXIS2_PLACEMENT_3D ( 'NONE', #11288, #16823, #3262 ) ;
#28321 = ORIENTED_EDGE ( 'NONE', *, *, #15963, .T. ) ;
#28322 = EDGE_LOOP ( 'NONE', ( #12658, #17078, #26378, #19824 ) ) ;
#28323 = CARTESIAN_POINT ( 'NONE',  ( 1.039999999999999591, -18.21166265554809627, 29.20140402659733425 ) ) ;
#28324 = DIRECTION ( 'NONE',  ( -1.000000000000000000, 0.000000000000000000, -0.000000000000000000 ) ) ;
#28325 = CARTESIAN_POINT ( 'NONE',  ( -9.978866888775527855, 8.235406450278427215, -67.50000000000000000 ) ) ;
#28326 = ORIENTED_EDGE ( 'NONE', *, *, #22349, .T. ) ;
#28327 = EDGE_CURVE ( 'NONE', #23446, #24976, #21487, .T. ) ;
#28329 = DIRECTION ( 'NONE',  ( -1.000000000000000000, 0.000000000000000000, -5.546364386991661285E-52 ) ) ;
#28328 = MECHANICAL_DESIGN_GEOMETRIC_PRESENTATION_REPRESENTATION (  '', ( #31172 ), #15303 ) ;
#28330 = EDGE_CURVE ( 'NONE', #23654, #13441, #6483, .T. ) ;
#28331 = CARTESIAN_POINT ( 'NONE',  ( -15.64512930492131382, -28.53829535743844659, -36.68877005347593467 ) ) ;
#28332 = ORIENTED_EDGE ( 'NONE', *, *, #26475, .T. ) ;
#28333 = CARTESIAN_POINT ( 'NONE',  ( 0.000000000000000000, 0.000000000000000000, 3.930000000000000160 ) ) ;
#28334 = DIRECTION ( 'NONE',  ( 1.000000000000000000, 0.000000000000000000, -0.000000000000000000 ) ) ;
#28335 = ADVANCED_FACE ( 'NONE', ( #22706 ), #27852, .F. ) ;
#28336 = DIRECTION ( 'NONE',  ( -0.8568571761675891629, -0.5155538571770218459, -9.470570714698669088E-17 ) ) ;
#28337 = CIRCLE ( 'NONE', #31179, 30.47050528711512030 ) ;
#28339 = DIRECTION ( 'NONE',  ( -0.000000000000000000, -0.000000000000000000, -1.000000000000000000 ) ) ;
#28338 = LINE ( 'NONE', #33850, #23034 ) ;
#28341 = EDGE_CURVE ( 'NONE', #30722, #20533, #27364, .T. ) ;
#28340 = CARTESIAN_POINT ( 'NONE',  ( 145.0000000000000568, -97.49999999999998579, 51.88904920397793319 ) ) ;
#28342 = LINE ( 'NONE', #9644, #2890 ) ;
#28343 = ORIENTED_EDGE ( 'NONE', *, *, #8888, .F. ) ;
#28344 = LINE ( 'NONE', #28512, #28109 ) ;
#28345 = CYLINDRICAL_SURFACE ( 'NONE', #8048, 2.524999999999999467 ) ;
#28346 = CIRCLE ( 'NONE', #11867, 30.47050528711512030 ) ;
#28347 = AXIS2_PLACEMENT_3D ( 'NONE', #15495, #15147, #7636 ) ;
#28348 = EDGE_LOOP ( 'NONE', ( #28436, #21363, #16952, #8911 ) ) ;
#28349 = ORIENTED_EDGE ( 'NONE', *, *, #10937, .T. ) ;
#28350 = ORIENTED_EDGE ( 'NONE', *, *, #17593, .T. ) ;
#28351 = AXIS2_PLACEMENT_3D ( 'NONE', #8864, #22578, #6003 ) ;
#28352 = CARTESIAN_POINT ( 'NONE',  ( 19.99999999999998934, 4.559999999999908127, -172.9900000000000091 ) ) ;
#28353 = ORIENTED_EDGE ( 'NONE', *, *, #16373, .T. ) ;
#28354 = VERTEX_POINT ( 'NONE', #33001 ) ;
#28355 = ORIENTED_EDGE ( 'NONE', *, *, #21069, .T. ) ;
#28356 = ADVANCED_FACE ( 'NONE', ( #22168 ), #20038, .F. ) ;
#28357 = CARTESIAN_POINT ( 'NONE',  ( 2.789999999999999147, -17.83604598421683107, 24.70480026434158916 ) ) ;
#28358 = AXIS2_PLACEMENT_3D ( 'NONE', #33566, #1013, #3664 ) ;
#28359 = VERTEX_POINT ( 'NONE', #24827 ) ;
#28360 = CARTESIAN_POINT ( 'NONE',  ( 1.749999999999999778, -2.430610048905780030, -34.32897884578301984 ) ) ;
#28361 = CARTESIAN_POINT ( 'NONE',  ( 26.97014235612466493, -26.57093094961043533, 49.43553178847298568 ) ) ;
#28362 = ORIENTED_EDGE ( 'NONE', *, *, #34586, .T. ) ;
#28363 = ORIENTED_EDGE ( 'NONE', *, *, #494, .F. ) ;
#28364 = DIRECTION ( 'NONE',  ( 0.2149704402110236556, 0.9766205557100866574, 0.000000000000000000 ) ) ;
#28365 = CARTESIAN_POINT ( 'NONE',  ( -37.85301660235036536, 0.7430237821112573027, 68.31122994652405112 ) ) ;
#28366 = EDGE_CURVE ( 'NONE', #3550, #33018, #11148, .T. ) ;
#28367 = LINE ( 'NONE', #28707, #19868 ) ;
#28368 = CYLINDRICAL_SURFACE ( 'NONE', #15417, 16.19999999999999574 ) ;
#28369 = DIRECTION ( 'NONE',  ( -3.469446951953832974E-18, -1.000000000000000000, -7.888609052210116302E-31 ) ) ;
#28370 = ORIENTED_EDGE ( 'NONE', *, *, #16448, .T. ) ;
#28371 = EDGE_CURVE ( 'NONE', #14545, #29231, #9163, .T. ) ;
#28372 = PLANE ( 'NONE',  #13491 ) ;
#28373 = ADVANCED_FACE ( 'NONE', ( #33192 ), #13809, .T. ) ;
#28374 = AXIS2_PLACEMENT_3D ( 'NONE', #12651, #34348, #29004 ) ;
#28375 = CARTESIAN_POINT ( 'NONE',  ( -30.76765767668600660, -10.60922306139170779, -36.68877005347593467 ) ) ;
#28376 = ORIENTED_EDGE ( 'NONE', *, *, #1542, .T. ) ;
#28377 = CARTESIAN_POINT ( 'NONE',  ( 0.000000000000000000, 2.296212748401288367E-15, 47.49999999999999289 ) ) ;
#28378 = CARTESIAN_POINT ( 'NONE',  ( 2.789999999999999147, 28.95078156989557527, 9.502838467758159879 ) ) ;
#28379 = DIRECTION ( 'NONE',  ( -1.000000000000000000, -0.000000000000000000, 0.000000000000000000 ) ) ;
#28380 = DIRECTION ( 'NONE',  ( 0.000000000000000000, 1.000000000000000000, -3.374343856708137958E-53 ) ) ;
#28382 = DIRECTION ( 'NONE',  ( 0.000000000000000000, 0.000000000000000000, 1.000000000000000000 ) ) ;
#28381 = LINE ( 'NONE', #12015, #33802 ) ;
#28383 = AXIS2_PLACEMENT_3D ( 'NONE', #30718, #6312, #16862 ) ;
#28384 = DIRECTION ( 'NONE',  ( 1.000000000000000000, 0.000000000000000000, 0.000000000000000000 ) ) ;
#28385 = EDGE_LOOP ( 'NONE', ( #34653, #26280, #30661, #7102 ) ) ;
#28386 = DIRECTION ( 'NONE',  ( 1.000000000000000000, 3.040835319149746528E-31, 1.232595164407830946E-32 ) ) ;
#28388 = CARTESIAN_POINT ( 'NONE',  ( -12.00000000000001066, -124.9999999999999432, -154.9999999999999716 ) ) ;
#28387 = FILL_AREA_STYLE_COLOUR ( '', #26298 ) ;
#28389 = AXIS2_PLACEMENT_3D ( 'NONE', #24622, #264, #7731 ) ;
#28390 = B_SPLINE_CURVE_WITH_KNOTS ( 'NONE', 3,
 ( #12483, #23327, #7113, #18013, #28837, #13698 ),
 .UNSPECIFIED., .F., .F.,
 ( 4, 2, 4 ),
 ( 4.404817130267440109E-07, 0.001874269701320914775, 0.003748098920928802889 ),
 .UNSPECIFIED. ) ;
#28391 = ORIENTED_EDGE ( 'NONE', *, *, #28841, .T. ) ;
#28392 = FACE_OUTER_BOUND ( 'NONE', #12884, .T. ) ;
#28393 = ORIENTED_EDGE ( 'NONE', *, *, #12670, .T. ) ;
#28394 = VECTOR ( 'NONE', #29049, 1000.000000000000000 ) ;
#28395 = VERTEX_POINT ( 'NONE', #19686 ) ;
#28396 = CARTESIAN_POINT ( 'NONE',  ( 104.2144883318369040, -5.687452395779748038, -4.889156772952023999 ) ) ;
#28397 = ORIENTED_EDGE ( 'NONE', *, *, #12592, .F. ) ;
#28398 = VERTEX_POINT ( 'NONE', #30533 ) ;
#28399 = CARTESIAN_POINT ( 'NONE',  ( -35.00000000000000000, -14.38258422898374533, 21.76353962326706082 ) ) ;
#28400 = DIRECTION ( 'NONE',  ( 1.000000000000000000, 0.000000000000000000, 0.000000000000000000 ) ) ;
#28401 = AXIS2_PLACEMENT_3D ( 'NONE', #6223, #30635, #8913 ) ;
#28402 = DIRECTION ( 'NONE',  ( -1.000000000000000000, 0.000000000000000000, 1.232595164407831220E-32 ) ) ;
#28403 = DIRECTION ( 'NONE',  ( -1.000000000000000000, 6.792721752314501023E-48, -3.697785493223492838E-32 ) ) ;
#28404 = ORIENTED_EDGE ( 'NONE', *, *, #24356, .T. ) ;
#28405 = ORIENTED_EDGE ( 'NONE', *, *, #12465, .T. ) ;
#28406 = EDGE_CURVE ( 'NONE', #16394, #245, #4602, .T. ) ;
#28407 = LINE ( 'NONE', #1354, #14572 ) ;
#28408 = CARTESIAN_POINT ( 'NONE',  ( -0.6763010051031078662, -1.505030548027689319, 0.000000000000000000 ) ) ;
#28409 = CARTESIAN_POINT ( 'NONE',  ( -20.00000000000007461, -109.0000000000000142, -162.9999999999999716 ) ) ;
#28410 = ADVANCED_FACE ( 'NONE', ( #33370 ), #27499, .F. ) ;
#28411 = CARTESIAN_POINT ( 'NONE',  ( -499.9999999999999432, -113.0000000000000000, -187.0000000000000000 ) ) ;
#28412 = CARTESIAN_POINT ( 'NONE',  ( -3.250000000000000000, 5.404196845913421754, 4.679999999999999716 ) ) ;
#28413 = AXIS2_PLACEMENT_3D ( 'NONE', #638, #3300, #11499 ) ;
#28414 = DIRECTION ( 'NONE',  ( 0.000000000000000000, 1.000000000000000000, 0.000000000000000000 ) ) ;
#28415 = EDGE_CURVE ( 'NONE', #9440, #19893, #21116, .T. ) ;
#28416 = CARTESIAN_POINT ( 'NONE',  ( -449.9999999999999432, 124.9999999999999432, -162.9999999999999716 ) ) ;
#28417 = VERTEX_POINT ( 'NONE', #26710 ) ;
#28418 = ADVANCED_FACE ( 'NONE', ( #28392 ), #20386, .T. ) ;
#28419 = DIRECTION ( 'NONE',  ( -0.000000000000000000, -0.000000000000000000, -1.000000000000000000 ) ) ;
#28420 = CARTESIAN_POINT ( 'NONE',  ( -442.0000000000000000, 105.0000000000000142, 107.9999999999999858 ) ) ;
#28421 = DIRECTION ( 'NONE',  ( 0.000000000000000000, 2.465190328815661892E-32, 1.000000000000000000 ) ) ;
#28422 = VERTEX_POINT ( 'NONE', #28906 ) ;
#28423 = LINE ( 'NONE', #1022, #6419 ) ;
#28424 = ORIENTED_EDGE ( 'NONE', *, *, #6531, .T. ) ;
#28425 = CARTESIAN_POINT ( 'NONE',  ( 2.765921099433441999, 4.286445725888479608, -30.79383171238939809 ) ) ;
#28426 = DIRECTION ( 'NONE',  ( -1.000000000000000000, -0.000000000000000000, -0.000000000000000000 ) ) ;
#28427 = EDGE_CURVE ( 'NONE', #12281, #27481, #31062, .T. ) ;
#28428 = ORIENTED_EDGE ( 'NONE', *, *, #5810, .T. ) ;
#28429 = CARTESIAN_POINT ( 'NONE',  ( -20.63749999999999929, 0.000000000000000000, 0.000000000000000000 ) ) ;
#28430 = CARTESIAN_POINT ( 'NONE',  ( -1.341640786499875171, 1.445083222993876839E-15, 11.80000000000000071 ) ) ;
#28431 = LINE ( 'NONE', #10039, #34249 ) ;
#28432 = ORIENTED_EDGE ( 'NONE', *, *, #440, .T. ) ;
#28433 = AXIS2_PLACEMENT_3D ( 'NONE', #13036, #34383, #13386 ) ;
#28434 = DIRECTION ( 'NONE',  ( -7.893605728314051750E-14, 1.618803117314786530E-15, 1.000000000000000000 ) ) ;
#28435 = PLANE ( 'NONE',  #22158 ) ;
#28436 = ORIENTED_EDGE ( 'NONE', *, *, #24584, .F. ) ;
#28437 = DIRECTION ( 'NONE',  ( -0.9289767198167909745, 0.3701381553399156199, -0.000000000000000000 ) ) ;
#28438 = CARTESIAN_POINT ( 'NONE',  ( 2.789999999999999147, 29.94779062842786743, 5.619744560739183825 ) ) ;
#28439 = DIRECTION ( 'NONE',  ( -1.000000000000000000, 0.000000000000000000, -0.000000000000000000 ) ) ;
#28440 = ITEM_DEFINED_TRANSFORMATION ( 'NONE', 'NONE', #33719,  #28566 ) ;
#28441 = ORIENTED_EDGE ( 'NONE', *, *, #19742, .T. ) ;
#28442 = ORIENTED_EDGE ( 'NONE', *, *, #21782, .F. ) ;
#28443 = ORIENTED_EDGE ( 'NONE', *, *, #809, .T. ) ;
#28444 = LINE ( 'NONE', #31287, #20883 ) ;
#28445 = EDGE_CURVE ( 'NONE', #22809, #11184, #34771, .T. ) ;
#28446 = DIRECTION ( 'NONE',  ( -1.000000000000000000, -3.469446951953834515E-18, 2.736911063134582149E-48 ) ) ;
#28447 = DIRECTION ( 'NONE',  ( -0.000000000000000000, -1.000000000000000000, -0.000000000000000000 ) ) ;
#28448 = CYLINDRICAL_SURFACE ( 'NONE', #4629, 3.999999999999982681 ) ;
#28449 = CARTESIAN_POINT ( 'NONE',  ( -15.99999999999998579, -145.0000000000000000, -162.9999999999999432 ) ) ;
#28450 = DIRECTION ( 'NONE',  ( -1.000000000000000000, -0.000000000000000000, -0.000000000000000000 ) ) ;
#28451 = ORIENTED_EDGE ( 'NONE', *, *, #29246, .T. ) ;
#28452 = EDGE_CURVE ( 'NONE', #392, #32678, #9524, .T. ) ;
#28453 = EDGE_CURVE ( 'NONE', #19961, #3900, #23951, .T. ) ;
#28454 = CARTESIAN_POINT ( 'NONE',  ( 102.1101915285661050, 4.971174042719112229, 11.47116230092015421 ) ) ;
#28455 = CIRCLE ( 'NONE', #2292, 7.999999999999979572 ) ;
#28456 = VERTEX_POINT ( 'NONE', #25710 ) ;
#28457 = DIRECTION ( 'NONE',  ( -1.000000000000000000, 0.000000000000000000, 0.000000000000000000 ) ) ;
#28458 = ADVANCED_FACE ( 'NONE', ( #12211 ), #23056, .T. ) ;
#28459 = EDGE_CURVE ( 'NONE', #8996, #24880, #5197, .T. ) ;
#28460 = CARTESIAN_POINT ( 'NONE',  ( 50.00050000000000239, 12.80000000000000071, -3.000000000000000000 ) ) ;
#28461 = ORIENTED_EDGE ( 'NONE', *, *, #18413, .T. ) ;
#28462 = CARTESIAN_POINT ( 'NONE',  ( -20.00000000000001776, -109.0000000000000142, 162.9999999999999716 ) ) ;
#28463 = DIRECTION ( 'NONE',  ( 0.000000000000000000, 0.5000000000000007772, -0.8660254037844381525 ) ) ;
#28464 = LINE ( 'NONE', #12630, #27518 ) ;
#28465 = CIRCLE ( 'NONE', #21647, 11.22499999999999787 ) ;
#28466 = AXIS2_PLACEMENT_3D ( 'NONE', #21632, #32475, #29821 ) ;
#28467 = CARTESIAN_POINT ( 'NONE',  ( 0.5248942429777062602, -1.320925567293482761, 33.35364885818385972 ) ) ;
#28468 = UNCERTAINTY_MEASURE_WITH_UNIT (LENGTH_MEASURE( 1.000000000000000082E-05 ), #14663, 'distance_accuracy_value', 'NONE');
#28469 = CARTESIAN_POINT ( 'NONE',  ( -130.6469666100234406, 6.000000000000000000, -62.49999999999999289 ) ) ;
#28470 = LINE ( 'NONE', #1419, #33638 ) ;
#28472 = ADVANCED_FACE ( 'NONE', ( #13205 ), #26062, .T. ) ;
#28471 = ORIENTED_EDGE ( 'NONE', *, *, #24499, .F. ) ;
#28473 = ORIENTED_EDGE ( 'NONE', *, *, #4352, .T. ) ;
#28474 = DIRECTION ( 'NONE',  ( -0.1063910735369017202, 0.9943243633099136947, -1.000770725407181676E-14 ) ) ;
#28475 = AXIS2_PLACEMENT_3D ( 'NONE', #1698, #9705, #23250 ) ;
#28476 = VERTEX_POINT ( 'NONE', #1507 ) ;
#28477 = AXIS2_PLACEMENT_3D ( 'NONE', #250, #24611, #3084 ) ;
#28478 = DIRECTION ( 'NONE',  ( -1.000000000000000000, 0.000000000000000000, 1.848892746611746966E-32 ) ) ;
#28479 = EDGE_CURVE ( 'NONE', #12696, #984, #18080, .T. ) ;
#28480 = EDGE_CURVE ( 'NONE', #10477, #15683, #9688, .T. ) ;
#28481 = FACE_OUTER_BOUND ( 'NONE', #28000, .T. ) ;
#28482 = CONTEXT_DEPENDENT_SHAPE_REPRESENTATION ( #7125, #26290 ) ;
#28483 = ORIENTED_EDGE ( 'NONE', *, *, #27637, .T. ) ;
#28484 = CARTESIAN_POINT ( 'NONE',  ( 1.039999999999999591, -25.27164158951584483, 23.36088151536909052 ) ) ;
#28485 = FILL_AREA_STYLE ('',( #18908 ) ) ;
#28487 = CARTESIAN_POINT ( 'NONE',  ( 0.000000000000000000, 0.000000000000000000, -0.7500000000000000000 ) ) ;
#28486 = CARTESIAN_POINT ( 'NONE',  ( -37.85301660235036536, 0.7430237821112573027, 15.81122994652406355 ) ) ;
#28489 = VERTEX_POINT ( 'NONE', #7007 ) ;
#28488 = CIRCLE ( 'NONE', #14302, 2.525000000000001243 ) ;
#28490 = EDGE_LOOP ( 'NONE', ( #6253, #6153, #21638, #4445 ) ) ;
#28491 = LINE ( 'NONE', #17492, #21390 ) ;
#28492 = VECTOR ( 'NONE', #26883, 1000.000000000000000 ) ;
#28493 = AXIS2_PLACEMENT_3D ( 'NONE', #93, #2581, #18976 ) ;
#28494 = DIRECTION ( 'NONE',  ( 0.000000000000000000, -1.131431318426415506E-52, -1.000000000000000000 ) ) ;
#28495 = DIRECTION ( 'NONE',  ( -1.000000000000000000, -0.000000000000000000, -0.000000000000000000 ) ) ;
#28496 = ORIENTED_EDGE ( 'NONE', *, *, #7283, .F. ) ;
#28497 = LINE ( 'NONE', #20489, #22641 ) ;
#28498 = EDGE_CURVE ( 'NONE', #29721, #12372, #34175, .T. ) ;
#28499 = EDGE_CURVE ( 'NONE', #3983, #33784, #15890, .T. ) ;
#28500 = B_SPLINE_CURVE_WITH_KNOTS ( 'NONE', 3,
 ( #5239, #18801, #5590, #27313, #19326, #24636 ),
 .UNSPECIFIED., .F., .F.,
 ( 4, 2, 4 ),
 ( 4.404817058690223214E-07, 0.001874269648070855032, 0.003748098814435841305 ),
 .UNSPECIFIED. ) ;
#28501 = ORIENTED_EDGE ( 'NONE', *, *, #5568, .F. ) ;
#28502 = AXIS2_PLACEMENT_3D ( 'NONE', #15023, #2180, #23365 ) ;
#28503 = DIRECTION ( 'NONE',  ( 0.000000000000000000, 0.000000000000000000, 1.000000000000000000 ) ) ;
#28504 = CARTESIAN_POINT ( 'NONE',  ( -11.99999999999998224, -134.9999999999999716, 187.0000000000000000 ) ) ;
#28505 = FACE_OUTER_BOUND ( 'NONE', #16992, .T. ) ;
#28507 = DIRECTION ( 'NONE',  ( 0.000000000000000000, -0.08715574274765885976, -0.9961946980917454342 ) ) ;
#28506 = DIRECTION ( 'NONE',  ( 0.000000000000000000, 0.000000000000000000, 1.000000000000000000 ) ) ;
#28508 =( REPRESENTATION_RELATIONSHIP ('NONE','NONE', #23037, #11185 ) REPRESENTATION_RELATIONSHIP_WITH_TRANSFORMATION ( #32758 )SHAPE_REPRESENTATION_RELATIONSHIP( ) );
#28509 = CARTESIAN_POINT ( 'NONE',  ( 0.000000000000000000, -7.666252171205264254, -29.49034198003815632 ) ) ;
#28510 = FACE_BOUND ( 'NONE', #19650, .T. ) ;
#28511 = ORIENTED_EDGE ( 'NONE', *, *, #887, .F. ) ;
#28512 = CARTESIAN_POINT ( 'NONE',  ( 129.3530333899765594, 6.000000000000000000, -57.49999999999999289 ) ) ;
#28513 = PLANE ( 'NONE',  #29652 ) ;
#28514 = PRODUCT_DEFINITION_SHAPE ( 'NONE', 'NONE',  #35148 ) ;
#28515 = EDGE_LOOP ( 'NONE', ( #33368, #13388, #1904, #26642 ) ) ;
#28516 = AXIS2_PLACEMENT_3D ( 'NONE', #22023, #3322, #24324 ) ;
#28517 = AXIS2_PLACEMENT_3D ( 'NONE', #14709, #3981, #21385 ) ;
#28518 = AXIS2_PLACEMENT_3D ( 'NONE', #28504, #14467, #28154 ) ;
#28519 = ORIENTED_EDGE ( 'NONE', *, *, #23153, .T. ) ;
#28521 = ORIENTED_EDGE ( 'NONE', *, *, #28371, .T. ) ;
#28520 = EDGE_CURVE ( 'NONE', #1376, #28825, #28734, .T. ) ;
#28522 = ADVANCED_FACE ( 'NONE', ( #32233, #28211 ), #23389, .F. ) ;
#28523 = EDGE_CURVE ( 'NONE', #30531, #7014, #7466, .T. ) ;
#28524 = CARTESIAN_POINT ( 'NONE',  ( -499.9999999999999432, 104.9999999999999858, 187.0000000000000000 ) ) ;
#28525 = ORIENTED_EDGE ( 'NONE', *, *, #6753, .F. ) ;
#28526 = EDGE_LOOP ( 'NONE', ( #35050, #24706, #877, #24069, #11347, #31254, #26537, #16915 ) ) ;
#28527 = ORIENTED_EDGE ( 'NONE', *, *, #15800, .T. ) ;
#28528 = CARTESIAN_POINT ( 'NONE',  ( -19.99999999999998934, 144.9999999999999716, -186.9999999999999716 ) ) ;
#28529 = EDGE_CURVE ( 'NONE', #33917, #12216, #3813, .T. ) ;
#28530 = CIRCLE ( 'NONE', #13193, 2.524999999999999467 ) ;
#28531 = ADVANCED_FACE ( 'NONE', ( #18727 ), #30262, .F. ) ;
#28532 = VERTEX_POINT ( 'NONE', #16057 ) ;
#28533 = DIRECTION ( 'NONE',  ( -1.000000000000000000, -0.000000000000000000, -0.000000000000000000 ) ) ;
#28534 = CARTESIAN_POINT ( 'NONE',  ( 22.89764159710611224, 17.63622956525712482, -87.50000000000000000 ) ) ;
#28535 = ORIENTED_EDGE ( 'NONE', *, *, #24939, .T. ) ;
#28536 = ORIENTED_EDGE ( 'NONE', *, *, #20685, .F. ) ;
#28537 = CARTESIAN_POINT ( 'NONE',  ( -12.00000000000003908, -134.9999999999999716, -194.9999999999999432 ) ) ;
#28538 = CARTESIAN_POINT ( 'NONE',  ( 0.5288002343768358759, -29.62362497318133947, 15.40519487321878778 ) ) ;
#28539 = CARTESIAN_POINT ( 'NONE',  ( 0.006892381647577837216, 18.40335333576913612, -24.78429060331921718 ) ) ;
#28540 = DIRECTION ( 'NONE',  ( 0.000000000000000000, 0.000000000000000000, 1.000000000000000000 ) ) ;
#28541 = CARTESIAN_POINT ( 'NONE',  ( 2.789999999999999147, 25.67797970382134309, 16.40405592474765939 ) ) ;
#28542 = ORIENTED_EDGE ( 'NONE', *, *, #19016, .F. ) ;
#28543 = CARTESIAN_POINT ( 'NONE',  ( 3.235562306570555532E-30, -1.691831803474591833, -67.50000000000000000 ) ) ;
#28544 = DIRECTION ( 'NONE',  ( 0.000000000000000000, 1.836970198721029441E-16, -1.000000000000000000 ) ) ;
#28545 = DIRECTION ( 'NONE',  ( -1.000000000000000000, 0.000000000000000000, -1.300283923313630633E-47 ) ) ;
#28546 = ORIENTED_EDGE ( 'NONE', *, *, #24293, .F. ) ;
#28547 = AXIS2_PLACEMENT_3D ( 'NONE', #30165, #24993, #6300 ) ;
#28548 = AXIS2_PLACEMENT_3D ( 'NONE', #28810, #9945, #18159 ) ;
#28549 = LINE ( 'NONE', #20712, #32128 ) ;
#28550 = CARTESIAN_POINT ( 'NONE',  ( 0.000000000000000000, 33.69708579775584667, 49.43553178847298568 ) ) ;
#28551 = FACE_OUTER_BOUND ( 'NONE', #30851, .T. ) ;
#28552 = CARTESIAN_POINT ( 'NONE',  ( -20.00000000000004619, -137.0000000000000000, -162.9999999999999716 ) ) ;
#28554 = DIRECTION ( 'NONE',  ( 0.000000000000000000, -0.000000000000000000, -1.000000000000000000 ) ) ;
#28553 = DIRECTION ( 'NONE',  ( -3.469446951953832974E-18, -1.000000000000000000, -7.888609052210116302E-31 ) ) ;
#28555 = DIRECTION ( 'NONE',  ( 1.000000000000000000, 0.000000000000000000, 0.000000000000000000 ) ) ;
#28556 = ORIENTED_EDGE ( 'NONE', *, *, #21132, .F. ) ;
#28557 = DIRECTION ( 'NONE',  ( 0.000000000000000000, 1.310824597558155437E-49, 1.000000000000000000 ) ) ;
#28559 = CARTESIAN_POINT ( 'NONE',  ( 5.021133111224162171, -25.61315202898005694, -87.50000000000000000 ) ) ;
#28558 = CARTESIAN_POINT ( 'NONE',  ( -349.0000000000000000, -135.0000000000000000, 128.0000000000000000 ) ) ;
#28560 = ORIENTED_EDGE ( 'NONE', *, *, #8197, .T. ) ;
#28561 =( REPRESENTATION_RELATIONSHIP ('NONE','NONE', #23037, #28231 ) REPRESENTATION_RELATIONSHIP_WITH_TRANSFORMATION ( #18045 )SHAPE_REPRESENTATION_RELATIONSHIP( ) );
#28562 = PRODUCT_DEFINITION_SHAPE ( 'NONE', 'NONE',  #35110 ) ;
#28563 = DIRECTION ( 'NONE',  ( 0.000000000000000000, 0.000000000000000000, 1.000000000000000000 ) ) ;
#28564 = VERTEX_POINT ( 'NONE', #26888 ) ;
#28565 = EDGE_CURVE ( 'NONE', #7091, #25547, #21675, .T. ) ;
#28566 = AXIS2_PLACEMENT_3D ( 'NONE', #26579, #2200, #13073 ) ;
#28567 = EDGE_CURVE ( 'NONE', #16094, #24969, #4883, .T. ) ;
#28568 = AXIS2_PLACEMENT_3D ( 'NONE', #28550, #6114, #33530 ) ;
#28569 = AXIS2_PLACEMENT_3D ( 'NONE', #33900, #20380, #9519 ) ;
#28570 = CIRCLE ( 'NONE', #8666, 7.999999999999979572 ) ;
#28571 = VERTEX_POINT ( 'NONE', #8192 ) ;
#28572 = CARTESIAN_POINT ( 'NONE',  ( 11.99999999999999645, -141.0000000000000000, -155.0000000000000284 ) ) ;
#28573 = ORIENTED_EDGE ( 'NONE', *, *, #20266, .T. ) ;
#28574 = ORIENTED_EDGE ( 'NONE', *, *, #23478, .T. ) ;
#28575 = CARTESIAN_POINT ( 'NONE',  ( 0.07094833748228242254, -18.14830959286913270, 25.98365187356515804 ) ) ;
#28576 = LINE ( 'NONE', #19263, #26664 ) ;
#28577 = CARTESIAN_POINT ( 'NONE',  ( 11.99999999999995559, -145.0000000000000000, 194.9999999999999716 ) ) ;
#28578 = CARTESIAN_POINT ( 'NONE',  ( -23.93921925319781963, 29.33115633223345142, 68.31122994652405112 ) ) ;
#28579 = ORIENTED_EDGE ( 'NONE', *, *, #20000, .F. ) ;
#28580 = ORIENTED_EDGE ( 'NONE', *, *, #32146, .T. ) ;
#28581 = PLANE ( 'NONE',  #24754 ) ;
#28582 = LINE ( 'NONE', #26077, #30559 ) ;
#28583 = DIRECTION ( 'NONE',  ( -1.000000000000000000, 0.000000000000000000, -1.300283923313630633E-47 ) ) ;
#28584 = LINE ( 'NONE', #17577, #20975 ) ;
#28585 = DIRECTION ( 'NONE',  ( -0.000000000000000000, -0.000000000000000000, -1.000000000000000000 ) ) ;
#28586 = CARTESIAN_POINT ( 'NONE',  ( -12.00000000000001066, -112.9999999999999858, -155.0000000000000284 ) ) ;
#28587 = DIRECTION ( 'NONE',  ( -1.000000000000000000, 0.000000000000000000, -0.000000000000000000 ) ) ;
#28588 = ORIENTED_EDGE ( 'NONE', *, *, #25046, .F. ) ;
#28589 = DIRECTION ( 'NONE',  ( 0.000000000000000000, -1.000000000000000000, -1.836970198721029934E-16 ) ) ;
#28590 = CARTESIAN_POINT ( 'NONE',  ( -27.76765758629847269, -16.97532223688792286, -36.68877005347593467 ) ) ;
#28591 = AXIS2_PLACEMENT_3D ( 'NONE', #15706, #23865, #21200 ) ;
#28592 = CARTESIAN_POINT ( 'NONE',  ( -70.00000000000000000, 4.559999999999908127, 172.9900000000000091 ) ) ;
#28593 = ORIENTED_EDGE ( 'NONE', *, *, #8387, .F. ) ;
#28594 = AXIS2_PLACEMENT_3D ( 'NONE', #26309, #21330, #24158 ) ;
#28595 = VECTOR ( 'NONE', #9297, 1000.000000000000000 ) ;
#28596 = CIRCLE ( 'NONE', #13252, 2.525000000000001688 ) ;
#28597 = DIRECTION ( 'NONE',  ( -0.000000000000000000, 1.000000000000000000, -0.000000000000000000 ) ) ;
#28598 = ORIENTED_EDGE ( 'NONE', *, *, #4490, .T. ) ;
#28599 = CARTESIAN_POINT ( 'NONE',  ( -12.00000000000001066, 144.9999999999999716, -175.0000000000000284 ) ) ;
#28600 = CARTESIAN_POINT ( 'NONE',  ( -109.6568079071416406, 2.122570655097208991, 12.31945284403700036 ) ) ;
#28601 = VERTEX_POINT ( 'NONE', #13551 ) ;
#28602 = CARTESIAN_POINT ( 'NONE',  ( -30.76765767668600660, -10.60922306139172555, 68.31122994652405112 ) ) ;
#28603 = DIRECTION ( 'NONE',  ( 0.8835120444460227151, -0.4684084406997905403, -8.604523463949019211E-17 ) ) ;
#28604 = EDGE_CURVE ( 'NONE', #32360, #18325, #5696, .T. ) ;
#28605 = ORIENTED_EDGE ( 'NONE', *, *, #30624, .F. ) ;
#28606 = ADVANCED_FACE ( 'NONE', ( #27417 ), #3025, .T. ) ;
#28607 = PRESENTATION_LAYER_ASSIGNMENT (  '', '', ( #34291 ) ) ;
#28608 = DIRECTION ( 'NONE',  ( 2.509304397856953769E-14, -1.077293903303772709E-14, 1.000000000000000000 ) ) ;
#28609 = CARTESIAN_POINT ( 'NONE',  ( 103.1320501907914888, -5.438347208236144148, 11.25609171608219938 ) ) ;
#28610 = ORIENTED_EDGE ( 'NONE', *, *, #33829, .F. ) ;
#28611 = LINE ( 'NONE', #20265, #34912 ) ;
#28612 = AXIS2_PLACEMENT_3D ( 'NONE', #13161, #5475, #4769 ) ;
#28613 = LINE ( 'NONE', #4550, #7888 ) ;
#28614 = VECTOR ( 'NONE', #14021, 1000.000000000000000 ) ;
#28615 = LINE ( 'NONE', #28086, #7643 ) ;
#28616 = CARTESIAN_POINT ( 'NONE',  ( -5.469264258321805627, 1.713938105891546382, 5.429999999999999716 ) ) ;
#28617 = ORIENTED_EDGE ( 'NONE', *, *, #13495, .F. ) ;
#28618 = ORIENTED_EDGE ( 'NONE', *, *, #27569, .T. ) ;
#28619 = VECTOR ( 'NONE', #11759, 1000.000000000000000 ) ;
#28620 = ORIENTED_EDGE ( 'NONE', *, *, #31740, .F. ) ;
#28621 = CARTESIAN_POINT ( 'NONE',  ( 2.765921099433441555, 24.20451283648857554, -19.51346322004903300 ) ) ;
#28622 = DIRECTION ( 'NONE',  ( 1.000000000000000000, 0.000000000000000000, 0.000000000000000000 ) ) ;
#28623 = CARTESIAN_POINT ( 'NONE',  ( 0.02407890056655825201, -31.05158812718220673, -1.559667679918931738 ) ) ;
#28624 = CARTESIAN_POINT ( 'NONE',  ( -410.0000000000000568, 137.0000000000000000, -155.0000000000000000 ) ) ;
#28625 = DIRECTION ( 'NONE',  ( 0.000000000000000000, 1.000000000000000000, -3.374343856708137958E-53 ) ) ;
#28626 = CARTESIAN_POINT ( 'NONE',  ( -25.07182831876307105, -28.36910952062234870, 68.31122994652405112 ) ) ;
#28627 = VERTEX_POINT ( 'NONE', #10874 ) ;
#28628 = CARTESIAN_POINT ( 'NONE',  ( 109.3087324328219978, 3.794064876973125333, 11.91123467351735954 ) ) ;
#28629 = VERTEX_POINT ( 'NONE', #24387 ) ;
#28630 = AXIS2_PLACEMENT_3D ( 'NONE', #3226, #568, #22280 ) ;
#28631 = DIRECTION ( 'NONE',  ( 0.000000000000000000, -1.310824597558155437E-49, -1.000000000000000000 ) ) ;
#28632 = ORIENTED_EDGE ( 'NONE', *, *, #19388, .T. ) ;
#28633 = DIRECTION ( 'NONE',  ( 1.000000000000000000, 3.040835319149746090E-31, 1.232595164407830946E-32 ) ) ;
#28634 = CARTESIAN_POINT ( 'NONE',  ( 2.789999999999999147, -20.92506858792771851, 22.14933852381669510 ) ) ;
#28635 = AXIS2_PLACEMENT_3D ( 'NONE', #4634, #7851, #5169 ) ;
#28636 = AXIS2_PLACEMENT_3D ( 'NONE', #34418, #23734, #20542 ) ;
#28637 = AXIS2_PLACEMENT_3D ( 'NONE', #33537, #20030, #798 ) ;
#28638 = DIRECTION ( 'NONE',  ( -0.000000000000000000, -0.000000000000000000, -1.000000000000000000 ) ) ;
#28639 = FACE_OUTER_BOUND ( 'NONE', #7132, .T. ) ;
#28640 = CARTESIAN_POINT ( 'NONE',  ( -361.0000000000000000, -125.0000000000000284, 112.0000000000000000 ) ) ;
#28641 = EDGE_CURVE ( 'NONE', #29194, #1101, #13674, .T. ) ;
#28642 = ORIENTED_EDGE ( 'NONE', *, *, #34671, .F. ) ;
#28643 = ORIENTED_EDGE ( 'NONE', *, *, #18553, .F. ) ;
#28644 = DIRECTION ( 'NONE',  ( -7.893605728314050488E-14, 1.618803117314786135E-15, 0.9999999999999998890 ) ) ;
#28645 = B_SPLINE_CURVE_WITH_KNOTS ( 'NONE', 3,
 ( #23532, #28700, #31711, #7319 ),
 .UNSPECIFIED., .F., .F.,
 ( 4, 4 ),
 ( 0.005298392425857884405, 0.005985260475359765499 ),
 .UNSPECIFIED. ) ;
#28646 = EDGE_CURVE ( 'NONE', #19641, #3175, #25610, .T. ) ;
#28647 = ORIENTED_EDGE ( 'NONE', *, *, #29030, .T. ) ;
#28648 = EDGE_CURVE ( 'NONE', #33070, #7332, #13898, .T. ) ;
#28649 = CARTESIAN_POINT ( 'NONE',  ( 2.765921099433441999, -29.68817180695669578, -9.232883799364548949 ) ) ;
#28650 = AXIS2_PLACEMENT_3D ( 'NONE', #7229, #31280, #15445 ) ;
#28651 = EDGE_CURVE ( 'NONE', #8202, #33289, #32569, .T. ) ;
#28652 = DIRECTION ( 'NONE',  ( 0.000000000000000000, 0.000000000000000000, -1.000000000000000000 ) ) ;
#28653 = EDGE_CURVE ( 'NONE', #27112, #19297, #377, .T. ) ;
#28654 = CONTEXT_DEPENDENT_SHAPE_REPRESENTATION ( #33288, #28562 ) ;
#28655 = ORIENTED_EDGE ( 'NONE', *, *, #4130, .F. ) ;
#28656 = DIRECTION ( 'NONE',  ( 0.7259954919231310644, -0.6876994588534230957, -1.263283411590317421E-16 ) ) ;
#28657 = DIRECTION ( 'NONE',  ( -1.000000000000000000, 0.000000000000000000, 0.000000000000000000 ) ) ;
#28658 = AXIS2_PLACEMENT_3D ( 'NONE', #32727, #26860, #32203 ) ;
#28659 = EDGE_CURVE ( 'NONE', #17344, #15610, #24452, .T. ) ;
#28660 = EDGE_CURVE ( 'NONE', #24520, #18645, #9228, .T. ) ;
#28662 = CARTESIAN_POINT ( 'NONE',  ( 2.789999999999999147, 27.98916443103621177, -15.38717335695007904 ) ) ;
#28661 = DIRECTION ( 'NONE',  ( 0.000000000000000000, 0.000000000000000000, -1.000000000000000000 ) ) ;
#28663 = VECTOR ( 'NONE', #14655, 1000.000000000000000 ) ;
#28664 = ORIENTED_EDGE ( 'NONE', *, *, #18724, .T. ) ;
#28665 = VERTEX_POINT ( 'NONE', #21903 ) ;
#28666 = VECTOR ( 'NONE', #4619, 1000.000000000000000 ) ;
#28667 = CARTESIAN_POINT ( 'NONE',  ( 11.99999999999999645, 144.9999999999999147, 162.9999999999999716 ) ) ;
#28668 = VECTOR ( 'NONE', #12995, 1000.000000000000000 ) ;
#28669 = CARTESIAN_POINT ( 'NONE',  ( 143.0000000000000568, -97.56119630548165844, -180.0000000000000000 ) ) ;
#28670 = DIRECTION ( 'NONE',  ( 0.9868265225415260300, 0.1617819965527648174, 0.000000000000000000 ) ) ;
#28671 = ORIENTED_EDGE ( 'NONE', *, *, #22428, .F. ) ;
#28672 = CYLINDRICAL_SURFACE ( 'NONE', #4342, 5.738084889453667792 ) ;
#28673 = ORIENTED_EDGE ( 'NONE', *, *, #18028, .T. ) ;
#28674 = CARTESIAN_POINT ( 'NONE',  ( 145.0000000000000568, 87.50000000000000000, -65.00000000000000000 ) ) ;
#28675 = PRESENTATION_STYLE_ASSIGNMENT (( #15337 ) ) ;
#28676 = PLANE ( 'NONE',  #22369 ) ;
#28678 = DIRECTION ( 'NONE',  ( -0.7259954919231303982, 0.6876994588534237618, 1.263283411590318407E-16 ) ) ;
#28677 = LINE ( 'NONE', #4278, #8227 ) ;
#28679 = FACE_OUTER_BOUND ( 'NONE', #5516, .T. ) ;
#28680 = CYLINDRICAL_SURFACE ( 'NONE', #12047, 2.033421858999711951 ) ;
#28681 = DIRECTION ( 'NONE',  ( -1.000000000000000000, 0.000000000000000000, 0.000000000000000000 ) ) ;
#28682 = CARTESIAN_POINT ( 'NONE',  ( -12.00000000000001066, 124.9999999999999716, 155.0000000000000000 ) ) ;
#28683 = CIRCLE ( 'NONE', #1977, 3.999999999999976019 ) ;
#28684 = DIRECTION ( 'NONE',  ( 0.000000000000000000, 0.000000000000000000, -1.000000000000000000 ) ) ;
#28685 = ORIENTED_EDGE ( 'NONE', *, *, #14375, .F. ) ;
#28686 = AXIS2_PLACEMENT_3D ( 'NONE', #19941, #17288, #11938 ) ;
#28687 = VERTEX_POINT ( 'NONE', #32752 ) ;
#28688 = ORIENTED_EDGE ( 'NONE', *, *, #16889, .T. ) ;
#28689 = EDGE_CURVE ( 'NONE', #23161, #30243, #8376, .T. ) ;
#28690 = EDGE_CURVE ( 'NONE', #2454, #7193, #25237, .T. ) ;
#28691 = CYLINDRICAL_SURFACE ( 'NONE', #17069, 16.19999999999999929 ) ;
#28692 = EDGE_CURVE ( 'NONE', #31670, #21641, #3527, .T. ) ;
#28693 = ORIENTED_EDGE ( 'NONE', *, *, #21853, .T. ) ;
#28694 = ORIENTED_EDGE ( 'NONE', *, *, #30379, .T. ) ;
#28695 = ORIENTED_EDGE ( 'NONE', *, *, #31270, .T. ) ;
#28696 = DIRECTION ( 'NONE',  ( -0.000000000000000000, 1.000000000000000000, -0.000000000000000000 ) ) ;
#28697 = CONTEXT_DEPENDENT_SHAPE_REPRESENTATION ( #12210, #29784 ) ;
#28698 = CIRCLE ( 'NONE', #32096, 4.000000000000003553 ) ;
#28699 = ORIENTED_EDGE ( 'NONE', *, *, #7630, .F. ) ;
#28700 = CARTESIAN_POINT ( 'NONE',  ( 2.789999999999998703, 14.57887998322662781, -26.97387222978612797 ) ) ;
#28701 = FACE_BOUND ( 'NONE', #16695, .T. ) ;
#28702 = ORIENTED_EDGE ( 'NONE', *, *, #22058, .F. ) ;
#28703 = EDGE_LOOP ( 'NONE', ( #7235, #27747, #10108, #24714, #29398, #17991 ) ) ;
#28704 = CARTESIAN_POINT ( 'NONE',  ( 0.1134162231544147831, -2.627030748427853002, 13.50000000000000000 ) ) ;
#28705 = FACE_OUTER_BOUND ( 'NONE', #26808, .T. ) ;
#28706 = VECTOR ( 'NONE', #2053, 1000.000000000000000 ) ;
#28707 = CARTESIAN_POINT ( 'NONE',  ( -70.00000000000000000, 4.559999999999908127, -177.7400000000000091 ) ) ;
#28709 = ADVANCED_FACE ( 'NONE', ( #1398 ), #20447, .F. ) ;
#28708 = LINE ( 'NONE', #18055, #8001 ) ;
#28710 = CARTESIAN_POINT ( 'NONE',  ( -414.0000000000000568, -112.9999999999999858, -174.9999999999999716 ) ) ;
#28711 = VERTEX_POINT ( 'NONE', #28624 ) ;
#28712 = CARTESIAN_POINT ( 'NONE',  ( 8.000000000000000000, 0.000000000000000000, 0.000000000000000000 ) ) ;
#28713 = VECTOR ( 'NONE', #12461, 1000.000000000000000 ) ;
#28714 = CARTESIAN_POINT ( 'NONE',  ( -442.0000000000000000, -105.0000000000000142, -109.9999999999999574 ) ) ;
#28715 = ORIENTED_EDGE ( 'NONE', *, *, #8382, .T. ) ;
#28716 = AXIS2_PLACEMENT_3D ( 'NONE', #9678, #13062, #23217 ) ;
#28717 = CARTESIAN_POINT ( 'NONE',  ( 1.040000000000001368, -33.26546734453825138, 8.820166447041648539 ) ) ;
#28719 = EDGE_CURVE ( 'NONE', #22002, #12565, #6371, .T. ) ;
#28718 = LINE ( 'NONE', #1, #24582 ) ;
#28720 = FILL_AREA_STYLE_COLOUR ( '', #25755 ) ;
#28721 = CARTESIAN_POINT ( 'NONE',  ( -499.9999999999999432, 108.9999999999999858, -187.0000000000000000 ) ) ;
#28723 = CARTESIAN_POINT ( 'NONE',  ( -104.6542607667447982, 5.115129524682072493, -5.485020507536669143 ) ) ;
#28722 = LINE ( 'NONE', #20884, #13904 ) ;
#28724 = ADVANCED_FACE ( 'NONE', ( #11917 ), #23124, .F. ) ;
#28725 = DIRECTION ( 'NONE',  ( 0.000000000000000000, -1.000000000000000000, -2.309213040847544338E-50 ) ) ;
#28726 = ORIENTED_EDGE ( 'NONE', *, *, #27562, .T. ) ;
#28727 = CARTESIAN_POINT ( 'NONE',  ( 103.1339222934114588, 5.429478283318185383, -11.25942253076638089 ) ) ;
#28729 = DIRECTION ( 'NONE',  ( -1.000000000000000000, 0.000000000000000000, 0.000000000000000000 ) ) ;
#28728 = DIRECTION ( 'NONE',  ( 1.000000000000000000, -0.000000000000000000, -0.000000000000000000 ) ) ;
#28730 = ADVANCED_FACE ( 'NONE', ( #17084 ), #2861, .T. ) ;
#28731 = VECTOR ( 'NONE', #12560, 1000.000000000000000 ) ;
#28732 = VERTEX_POINT ( 'NONE', #33966 ) ;
#28733 = CIRCLE ( 'NONE', #10550, 10.00000000000000000 ) ;
#28734 = LINE ( 'NONE', #34914, #27931 ) ;
#28735 = AXIS2_PLACEMENT_3D ( 'NONE', #34942, #24057, #12886 ) ;
#28736 = VERTEX_POINT ( 'NONE', #25955 ) ;
#28737 = EDGE_CURVE ( 'NONE', #23952, #22709, #3707, .T. ) ;
#28738 = ORIENTED_EDGE ( 'NONE', *, *, #31263, .T. ) ;
#28739 = DIRECTION ( 'NONE',  ( 1.000000000000000000, 0.000000000000000000, -1.848892746611746966E-32 ) ) ;
#28740 = EDGE_LOOP ( 'NONE', ( #13013, #765, #13213, #14219 ) ) ;
#28741 = ORIENTED_EDGE ( 'NONE', *, *, #9161, .F. ) ;
#28742 = DIRECTION ( 'NONE',  ( 0.000000000000000000, 1.000000000000000000, 0.000000000000000000 ) ) ;
#28743 = CIRCLE ( 'NONE', #25330, 4.000000000000003553 ) ;
#28744 = DIRECTION ( 'NONE',  ( -3.040835319149746090E-31, -1.000000000000000000, 0.000000000000000000 ) ) ;
#28745 = CYLINDRICAL_SURFACE ( 'NONE', #22816, 3.999999999999976019 ) ;
#28746 = ORIENTED_EDGE ( 'NONE', *, *, #3412, .T. ) ;
#28747 = VERTEX_POINT ( 'NONE', #30945 ) ;
#28748 = DIRECTION ( 'NONE',  ( 0.000000000000000000, -1.000000000000000000, 3.421138828918010427E-49 ) ) ;
#28749 = LINE ( 'NONE', #1175, #20321 ) ;
#28750 = CARTESIAN_POINT ( 'NONE',  ( 11.99999999999999645, 124.9999999999999716, 155.0000000000000000 ) ) ;
#28751 = DIRECTION ( 'NONE',  ( 0.000000000000000000, 0.000000000000000000, 1.000000000000000000 ) ) ;
#28752 = DIRECTION ( 'NONE',  ( 0.000000000000000000, 0.000000000000000000, -1.000000000000000000 ) ) ;
#28753 = VERTEX_POINT ( 'NONE', #14938 ) ;
#28754 = VECTOR ( 'NONE', #32809, 1000.000000000000000 ) ;
#28755 = PLANE ( 'NONE',  #17383 ) ;
#28756 = FACE_BOUND ( 'NONE', #1632, .T. ) ;
#28757 = ORIENTED_EDGE ( 'NONE', *, *, #28689, .T. ) ;
#28758 = CIRCLE ( 'NONE', #23653, 2.000000000000001776 ) ;
#28759 = DIRECTION ( 'NONE',  ( -0.7259954919231307313, 0.6876994588534234287, 0.000000000000000000 ) ) ;
#28760 = CARTESIAN_POINT ( 'NONE',  ( 2.789999999999999147, -29.63162325403024511, 6.967017504691655816 ) ) ;
#28761 = EDGE_CURVE ( 'NONE', #32672, #21866, #7405, .T. ) ;
#28762 = CARTESIAN_POINT ( 'NONE',  ( 7.700000000000000178, 0.000000000000000000, -10.30000000000000071 ) ) ;
#28763 = EDGE_LOOP ( 'NONE', ( #7989, #15294, #20440, #10538, #7703, #17113, #25925, #31484 ) ) ;
#28764 = EDGE_CURVE ( 'NONE', #17068, #25913, #14416, .T. ) ;
#28765 =( REPRESENTATION_RELATIONSHIP ('NONE','NONE', #23037, #15767 ) REPRESENTATION_RELATIONSHIP_WITH_TRANSFORMATION ( #29322 )SHAPE_REPRESENTATION_RELATIONSHIP( ) );
#28766 = CYLINDRICAL_SURFACE ( 'NONE', #8127, 4.000000000000003553 ) ;
#28767 = ORIENTED_EDGE ( 'NONE', *, *, #21011, .T. ) ;
#28769 = LINE ( 'NONE', #20761, #25931 ) ;
#28768 = DIRECTION ( 'NONE',  ( 0.000000000000000000, 1.131431318426415506E-52, 1.000000000000000000 ) ) ;
#28771 = AXIS2_PLACEMENT_3D ( 'NONE', #16045, #4980, #34722 ) ;
#28770 = CARTESIAN_POINT ( 'NONE',  ( 1.040000000000000036, 31.89769921723006263, -12.91988538846923973 ) ) ;
#28772 = AXIS2_PLACEMENT_3D ( 'NONE', #31076, #22720, #14542 ) ;
#28773 = ORIENTED_EDGE ( 'NONE', *, *, #273, .T. ) ;
#28774 = DIRECTION ( 'NONE',  ( 1.000000000000000000, 0.000000000000000000, 0.000000000000000000 ) ) ;
#28775 = EDGE_CURVE ( 'NONE', #33378, #31064, #30349, .T. ) ;
#28776 = CARTESIAN_POINT ( 'NONE',  ( -5.210000000000000853, 0.000000000000000000, 0.000000000000000000 ) ) ;
#28777 = ORIENTED_EDGE ( 'NONE', *, *, #1003, .T. ) ;
#28778 = AXIS2_PLACEMENT_3D ( 'NONE', #16427, #14098, #27256 ) ;
#28779 = DIRECTION ( 'NONE',  ( -0.4682816961312821213, 0.8835792285179693284, -1.947002203604375884E-14 ) ) ;
#28780 = ORIENTED_EDGE ( 'NONE', *, *, #33927, .F. ) ;
#28781 = LINE ( 'NONE', #26456, #10211 ) ;
#28782 = VERTEX_POINT ( 'NONE', #9230 ) ;
#28783 = AXIS2_PLACEMENT_3D ( 'NONE', #30113, #6064, #24238 ) ;
#28784 = DIRECTION ( 'NONE',  ( 0.000000000000000000, 0.000000000000000000, 1.000000000000000000 ) ) ;
#28785 = FILL_AREA_STYLE ('',( #31451 ) ) ;
#28786 = DIRECTION ( 'NONE',  ( -0.000000000000000000, 1.836970198721029688E-16, -1.000000000000000000 ) ) ;
#28787 = LINE ( 'NONE', #23444, #9696 ) ;
#28788 = EDGE_LOOP ( 'NONE', ( #31629, #9859, #2686 ) ) ;
#28789 = VERTEX_POINT ( 'NONE', #25421 ) ;
#28790 = EDGE_LOOP ( 'NONE', ( #17779, #6489, #10933, #22680 ) ) ;
#28791 = EDGE_CURVE ( 'NONE', #29040, #6216, #31290, .T. ) ;
#28792 = CARTESIAN_POINT ( 'NONE',  ( -19.99999999999998934, 4.559999999999908127, -172.9900000000000091 ) ) ;
#28793 = VECTOR ( 'NONE', #8233, 1000.000000000000000 ) ;
#28794 = CARTESIAN_POINT ( 'NONE',  ( 0.006871054928023897015, -3.550602046213657381, 30.66465032581540839 ) ) ;
#28795 = CARTESIAN_POINT ( 'NONE',  ( -15.99999999999998579, 124.9999999999999716, 187.0000000000000000 ) ) ;
#28796 = DIRECTION ( 'NONE',  ( -1.000000000000000000, 0.000000000000000000, 0.000000000000000000 ) ) ;
#28797 = PLANE ( 'NONE',  #12357 ) ;
#28798 = DIRECTION ( 'NONE',  ( 0.000000000000000000, -1.000000000000000000, 0.000000000000000000 ) ) ;
#28799 = ORIENTED_EDGE ( 'NONE', *, *, #5079, .T. ) ;
#28800 = PRODUCT_DEFINITION_SHAPE ( 'NONE', 'NONE',  #35162 ) ;
#28801 = AXIS2_PLACEMENT_3D ( 'NONE', #9978, #29012, #4607 ) ;
#28802 = EDGE_CURVE ( 'NONE', #3348, #33660, #16536, .T. ) ;
#28803 = DIRECTION ( 'NONE',  ( 0.000000000000000000, 0.000000000000000000, 1.000000000000000000 ) ) ;
#28804 = EDGE_CURVE ( 'NONE', #12748, #14760, #31847, .T. ) ;
#28805 = ORIENTED_EDGE ( 'NONE', *, *, #30594, .F. ) ;
#28806 = VECTOR ( 'NONE', #26825, 1000.000000000000000 ) ;
#28807 = EDGE_CURVE ( 'NONE', #31407, #763, #7482, .T. ) ;
#28808 = CARTESIAN_POINT ( 'NONE',  ( 2.265105833353615150, -24.85743842207130427, 22.27820639183311968 ) ) ;
#28809 = ORIENTED_EDGE ( 'NONE', *, *, #12159, .F. ) ;
#28810 = CARTESIAN_POINT ( 'NONE',  ( -12.00000000000003908, -134.9999999999999716, -162.9999999999999432 ) ) ;
#28811 = CARTESIAN_POINT ( 'NONE',  ( -143.0000000000000568, -167.8552739801376390, -46.75049602362128809 ) ) ;
#28812 = DIRECTION ( 'NONE',  ( 1.000000000000000000, 0.000000000000000000, -1.848892746611746966E-32 ) ) ;
#28813 = AXIS2_PLACEMENT_3D ( 'NONE', #7404, #18301, #14364 ) ;
#28814 = DIRECTION ( 'NONE',  ( -0.9868265225415261410, -0.1617819965527648174, 0.000000000000000000 ) ) ;
#28815 = ORIENTED_EDGE ( 'NONE', *, *, #6455, .T. ) ;
#28816 = ORIENTED_EDGE ( 'NONE', *, *, #18501, .F. ) ;
#28817 = CARTESIAN_POINT ( 'NONE',  ( 789.1951788766738218, 1035.989936556434031, 1753.598338701303419 ) ) ;
#28818 = EDGE_LOOP ( 'NONE', ( #6733, #21955 ) ) ;
#28819 = AXIS2_PLACEMENT_3D ( 'NONE', #7738, #25778, #1407 ) ;
#28820 = PLANE ( 'NONE',  #22077 ) ;
#28821 = AXIS2_PLACEMENT_3D ( 'NONE', #16692, #24147, #24320 ) ;
#28822 = AXIS2_PLACEMENT_3D ( 'NONE', #9981, #2490, #20838 ) ;
#28823 = CARTESIAN_POINT ( 'NONE',  ( 7.700000000000000178, 0.000000000000000000, 0.000000000000000000 ) ) ;
#28824 = CARTESIAN_POINT ( 'NONE',  ( 0.02407890056655695096, 11.80989368511462523, 28.76039115933989976 ) ) ;
#28825 = VERTEX_POINT ( 'NONE', #27917 ) ;
#28826 = LINE ( 'NONE', #27336, #6569 ) ;
#28827 = DIRECTION ( 'NONE',  ( 0.000000000000000000, 1.000000000000000000, -0.000000000000000000 ) ) ;
#28828 = CIRCLE ( 'NONE', #13497, 5.115020388170798959 ) ;
#28830 = DIRECTION ( 'NONE',  ( -0.000000000000000000, 1.836970198721029934E-16, -1.000000000000000000 ) ) ;
#28829 = CARTESIAN_POINT ( 'NONE',  ( -20.00000000000004619, -113.0000000000000000, -194.9999999999999432 ) ) ;
#28831 = ORIENTED_EDGE ( 'NONE', *, *, #19077, .F. ) ;
#28832 = ORIENTED_EDGE ( 'NONE', *, *, #23121, .F. ) ;
#28833 = CARTESIAN_POINT ( 'NONE',  ( 4.979875012683822710, -33.69708579775584667, 49.43553178847298568 ) ) ;
#28834 = ADVANCED_FACE ( 'NONE', ( #875 ), #28448, .F. ) ;
#28835 = VERTEX_POINT ( 'NONE', #9418 ) ;
#28836 = ADVANCED_FACE ( 'NONE', ( #17620 ), #2094, .T. ) ;
#28837 = CARTESIAN_POINT ( 'NONE',  ( 2.719051674337184199, 19.10378521888278058, -25.28945800968145363 ) ) ;
#28838 = DIRECTION ( 'NONE',  ( -0.000000000000000000, 1.000000000000000000, -0.000000000000000000 ) ) ;
#28839 = ORIENTED_EDGE ( 'NONE', *, *, #10853, .T. ) ;
#28840 = DIRECTION ( 'NONE',  ( 0.000000000000000000, 0.000000000000000000, 1.000000000000000000 ) ) ;
#28841 = EDGE_CURVE ( 'NONE', #19925, #4470, #1180, .T. ) ;
#28842 = PRODUCT_DEFINITION_SHAPE ( 'NONE', 'NONE',  #35114 ) ;
#28843 = ORIENTED_EDGE ( 'NONE', *, *, #23003, .T. ) ;
#28844 = EDGE_CURVE ( 'NONE', #10173, #1134, #34130, .T. ) ;
#28845 = CARTESIAN_POINT ( 'NONE',  ( -499.9999999999999432, -113.0000000000000000, -190.9999999999999716 ) ) ;
#28846 = CYLINDRICAL_SURFACE ( 'NONE', #4059, 1.999999999999999112 ) ;
#28847 = LINE ( 'NONE', #18192, #27492 ) ;
#28849 = CARTESIAN_POINT ( 'NONE',  ( -110.1150203881707910, -1.604996202923496961E-20, 7.500000000000000000 ) ) ;
#28848 = CARTESIAN_POINT ( 'NONE',  ( -347.0000000000000000, -125.0000000000000284, 181.0000000000000000 ) ) ;
#28850 = VECTOR ( 'NONE', #25433, 1000.000000000000000 ) ;
#28851 = DIRECTION ( 'NONE',  ( -0.000000000000000000, -0.000000000000000000, -1.000000000000000000 ) ) ;
#28852 = CARTESIAN_POINT ( 'NONE',  ( -418.0000000000000000, 104.9999999999999858, -190.9999999999999716 ) ) ;
#28853 = DIRECTION ( 'NONE',  ( -1.000000000000000000, 0.000000000000000000, -5.546364386991661285E-52 ) ) ;
#28854 = DIRECTION ( 'NONE',  ( 0.000000000000000000, 1.000000000000000000, 0.000000000000000000 ) ) ;
#28855 = ADVANCED_FACE ( 'NONE', ( #12965 ), #20021, .T. ) ;
#28856 = ADVANCED_FACE ( 'NONE', ( #26651 ), #26824, .F. ) ;
#28857 = AXIS2_PLACEMENT_3D ( 'NONE', #20913, #4001, #4179 ) ;
#28858 = ORIENTED_EDGE ( 'NONE', *, *, #23306, .T. ) ;
#28859 =( NAMED_UNIT ( * ) PLANE_ANGLE_UNIT ( ) SI_UNIT ( $, .RADIAN. ) );
#28860 = ORIENTED_EDGE ( 'NONE', *, *, #4129, .T. ) ;
#28861 = VERTEX_POINT ( 'NONE', #34488 ) ;
#28862 = AXIS2_PLACEMENT_3D ( 'NONE', #21215, #10187, #21037 ) ;
#28863 = DIRECTION ( 'NONE',  ( -1.000000000000000000, 0.000000000000000000, 0.000000000000000000 ) ) ;
#28864 = ORIENTED_EDGE ( 'NONE', *, *, #13987, .T. ) ;
#28865 = VERTEX_POINT ( 'NONE', #5098 ) ;
#28866 = VERTEX_POINT ( 'NONE', #29330 ) ;
#28867 = PLANE ( 'NONE',  #32684 ) ;
#28868 = CONTEXT_DEPENDENT_SHAPE_REPRESENTATION ( #30375, #20667 ) ;
#28869 = AXIS2_PLACEMENT_3D ( 'NONE', #34711, #8000, #27051 ) ;
#28870 = AXIS2_PLACEMENT_3D ( 'NONE', #14006, #19350, #17045 ) ;
#28871 = EDGE_LOOP ( 'NONE', ( #13008, #21032, #12480, #28353 ) ) ;
#28872 = DIRECTION ( 'NONE',  ( 8.498729137172956618E-17, 0.000000000000000000, 1.000000000000000000 ) ) ;
#28873 = CARTESIAN_POINT ( 'NONE',  ( 19.99999999999998934, -124.9999999999999432, -186.9999999999999716 ) ) ;
#28874 = ORIENTED_EDGE ( 'NONE', *, *, #5373, .T. ) ;
#28875 = VERTEX_POINT ( 'NONE', #4922 ) ;
#28876 = DIRECTION ( 'NONE',  ( -0.000000000000000000, -1.836970198721029688E-16, 1.000000000000000000 ) ) ;
#28877 = PLANE ( 'NONE',  #14133 ) ;
#28878 = CARTESIAN_POINT ( 'NONE',  ( -8.331222508929960727E-14, -29.22921979676802451, -9.265873697119378249 ) ) ;
#28879 = LINE ( 'NONE', #4479, #30183 ) ;
#28880 = CARTESIAN_POINT ( 'NONE',  ( 212.5000000000000000, 0.000000000000000000, 0.000000000000000000 ) ) ;
#28881 = VERTEX_POINT ( 'NONE', #18661 ) ;
#28882 = VECTOR ( 'NONE', #16251, 1000.000000000000000 ) ;
#28883 = CARTESIAN_POINT ( 'NONE',  ( -35.00000000000000000, 8.360858262960562115, -23.84547010402785006 ) ) ;
#28884 = DIRECTION ( 'NONE',  ( 0.000000000000000000, 1.000000000000000000, 0.000000000000000000 ) ) ;
#28885 = CARTESIAN_POINT ( 'NONE',  ( 19.99999999999998934, 4.559999999999909015, -168.2400000000000091 ) ) ;
#28886 = ORIENTED_EDGE ( 'NONE', *, *, #23478, .F. ) ;
#28887 = EDGE_CURVE ( 'NONE', #33691, #15781, #29095, .T. ) ;
#28888 = FACE_OUTER_BOUND ( 'NONE', #5800, .T. ) ;
#28889 = CARTESIAN_POINT ( 'NONE',  ( 143.0000000000000568, -187.5436536988702017, -180.0000000000000284 ) ) ;
#28890 = ADVANCED_FACE ( 'NONE', ( #10460, #23636, #7070 ), #2261, .F. ) ;
#28891 = AXIS2_PLACEMENT_3D ( 'NONE', #34004, #6594, #920 ) ;
#28892 = CARTESIAN_POINT ( 'NONE',  ( 105.0002580737914286, 5.748131698890998287, -4.817519326574049465 ) ) ;
#28894 = DIRECTION ( 'NONE',  ( 3.697785493223492838E-32, 1.934419779023891545E-16, -1.000000000000000000 ) ) ;
#28893 = DIRECTION ( 'NONE',  ( 1.000000000000000000, 0.000000000000000000, 0.000000000000000000 ) ) ;
#28895 = VECTOR ( 'NONE', #2860, 1000.000000000000000 ) ;
#28896 = ADVANCED_FACE ( 'NONE', ( #13135 ), #12446, .F. ) ;
#28897 = ADVANCED_FACE ( 'NONE', ( #4743 ), #31808, .F. ) ;
#28898 = CARTESIAN_POINT ( 'NONE',  ( 11.99999999999999645, 140.9999999999999716, 155.0000000000000000 ) ) ;
#28899 = ORIENTED_EDGE ( 'NONE', *, *, #27241, .F. ) ;
#28900 = CARTESIAN_POINT ( 'NONE',  ( 100.8156339766184146, 3.930740943550895761, -11.86668706373619209 ) ) ;
#28902 = LINE ( 'NONE', #7707, #22556 ) ;
#28901 = SURFACE_SIDE_STYLE ('',( #10033 ) ) ;
#28903 = CIRCLE ( 'NONE', #12459, 32.54542015209056416 ) ;
#28904 = ORIENTED_EDGE ( 'NONE', *, *, #19305, .T. ) ;
#28905 = PRODUCT_DEFINITION_SHAPE ( 'NONE', 'NONE',  #35247 ) ;
#28906 = CARTESIAN_POINT ( 'NONE',  ( 11.99999999999995559, -145.0000000000000000, -154.9999999999999716 ) ) ;
#28907 = ORIENTED_EDGE ( 'NONE', *, *, #19386, .T. ) ;
#28908 = EDGE_CURVE ( 'NONE', #22409, #29056, #12543, .T. ) ;
#28909 = AXIS2_PLACEMENT_3D ( 'NONE', #18663, #13137, #21831 ) ;
#28910 = ORIENTED_EDGE ( 'NONE', *, *, #19154, .F. ) ;
#28911 = PLANE ( 'NONE',  #23611 ) ;
#28912 = ORIENTED_EDGE ( 'NONE', *, *, #367, .F. ) ;
#28913 = ORIENTED_EDGE ( 'NONE', *, *, #22745, .F. ) ;
#28914 = DIRECTION ( 'NONE',  ( 0.000000000000000000, 0.000000000000000000, 1.000000000000000000 ) ) ;
#28915 = EDGE_CURVE ( 'NONE', #24841, #9803, #20789, .T. ) ;
#28916 = AXIS2_PLACEMENT_3D ( 'NONE', #21533, #26689, #2656 ) ;
#28918 = ADVANCED_FACE ( 'NONE', ( #31634 ), #18492, .F. ) ;
#28917 = DIRECTION ( 'NONE',  ( 0.000000000000000000, -1.000000000000000000, 0.000000000000000000 ) ) ;
#28919 = DIRECTION ( 'NONE',  ( -1.000000000000000000, -0.000000000000000000, -0.000000000000000000 ) ) ;
#28920 = ORIENTED_EDGE ( 'NONE', *, *, #6575, .F. ) ;
#28921 = ORIENTED_EDGE ( 'NONE', *, *, #32625, .T. ) ;
#28922 = CARTESIAN_POINT ( 'NONE',  ( -500.0000000000000000, -115.0000000000000000, -155.0000000000000000 ) ) ;
#28923 = LINE ( 'NONE', #11070, #3251 ) ;
#28924 = DIRECTION ( 'NONE',  ( -0.000000000000000000, -0.000000000000000000, -1.000000000000000000 ) ) ;
#28925 = DIRECTION ( 'NONE',  ( 0.000000000000000000, 0.000000000000000000, -1.000000000000000000 ) ) ;
#28926 = DIRECTION ( 'NONE',  ( -0.000000000000000000, 0.000000000000000000, 1.000000000000000000 ) ) ;
#28927 = ORIENTED_EDGE ( 'NONE', *, *, #17651, .F. ) ;
#28928 = ORIENTED_EDGE ( 'NONE', *, *, #33065, .T. ) ;
#28929 = MECHANICAL_DESIGN_GEOMETRIC_PRESENTATION_REPRESENTATION (  '', ( #9037 ), #11332 ) ;
#28930 = CARTESIAN_POINT ( 'NONE',  ( 19.99999999999998934, -32.99999999999997158, -175.0000000000000000 ) ) ;
#28931 = CARTESIAN_POINT ( 'NONE',  ( 0.02407890056655695096, -21.56796757982826307, 22.39322359481599278 ) ) ;
#28932 = ORIENTED_EDGE ( 'NONE', *, *, #31648, .F. ) ;
#28933 = DIRECTION ( 'NONE',  ( 0.000000000000000000, 1.000000000000000000, 0.000000000000000000 ) ) ;
#28934 = LINE ( 'NONE', #26608, #21166 ) ;
#28935 = AXIS2_PLACEMENT_3D ( 'NONE', #24102, #26959, #26605 ) ;
#28936 = DIRECTION ( 'NONE',  ( 0.000000000000000000, 1.131431318426415506E-52, 1.000000000000000000 ) ) ;
#28937 = ORIENTED_EDGE ( 'NONE', *, *, #5759, .F. ) ;
#28938 = EDGE_CURVE ( 'NONE', #28204, #20346, #18148, .T. ) ;
#28939 = EDGE_CURVE ( 'NONE', #15487, #29934, #15291, .T. ) ;
#28940 = CARTESIAN_POINT ( 'NONE',  ( 0.000000000000000000, 6.992329373473909019E-15, 49.43553178847298568 ) ) ;
#28941 = ORIENTED_EDGE ( 'NONE', *, *, #24038, .T. ) ;
#28943 = FACE_OUTER_BOUND ( 'NONE', #7585, .T. ) ;
#28942 = SURFACE_STYLE_USAGE ( .BOTH. , #29114 ) ;
#28944 = DIRECTION ( 'NONE',  ( 0.000000000000000000, 0.000000000000000000, 1.000000000000000000 ) ) ;
#28945 = EDGE_CURVE ( 'NONE', #17061, #33511, #1048, .T. ) ;
#28946 = AXIS2_PLACEMENT_3D ( 'NONE', #17875, #20188, #25331 ) ;
#28947 = ORIENTED_EDGE ( 'NONE', *, *, #9489, .F. ) ;
#28948 = CARTESIAN_POINT ( 'NONE',  ( -418.0000000000000000, -125.0000000000000000, 107.9999999999999858 ) ) ;
#28949 = LINE ( 'NONE', #15435, #26448 ) ;
#28950 = EDGE_LOOP ( 'NONE', ( #28270, #4116, #10837, #31779, #11911, #1732 ) ) ;
#28951=STYLED_ITEM('',(#35268),#10823);
#28952 = DIRECTION ( 'NONE',  ( -0.1063910735369225230, 0.9943243633099118073, -1.000770725407345128E-14 ) ) ;
#28953 = ORIENTED_EDGE ( 'NONE', *, *, #31646, .T. ) ;
#28954 = CARTESIAN_POINT ( 'NONE',  ( 2.783107534982237841, -0.3207854480225766913, -30.86813304286363646 ) ) ;
#28955 = ORIENTED_EDGE ( 'NONE', *, *, #32697, .F. ) ;
#28956 = DIRECTION ( 'NONE',  ( 1.000000000000000000, -0.000000000000000000, -0.000000000000000000 ) ) ;
#28957 = VECTOR ( 'NONE', #34831, 1000.000000000000000 ) ;
#28958 = EDGE_CURVE ( 'NONE', #18391, #28976, #17359, .T. ) ;
#28959 = DIRECTION ( 'NONE',  ( 0.000000000000000000, 0.000000000000000000, -1.000000000000000000 ) ) ;
#28960 = ADVANCED_FACE ( 'NONE', ( #2434 ), #13317, .F. ) ;
#28961 = DIRECTION ( 'NONE',  ( -0.000000000000000000, -0.000000000000000000, -1.000000000000000000 ) ) ;
#28962 = CARTESIAN_POINT ( 'NONE',  ( 0.7564103424913883877, 33.71046419695405660, -3.724096820061226332 ) ) ;
#28963 = ITEM_DEFINED_TRANSFORMATION ( 'NONE', 'NONE', #34873,  #28566 ) ;
#28964 = ORIENTED_EDGE ( 'NONE', *, *, #17905, .F. ) ;
#28965 = ORIENTED_EDGE ( 'NONE', *, *, #13144, .T. ) ;
#28966 = ORIENTED_EDGE ( 'NONE', *, *, #33429, .F. ) ;
#28967 = ADVANCED_FACE ( 'NONE', ( #24144 ), #17005, .T. ) ;
#28968 = DIRECTION ( 'NONE',  ( 0.000000000000000000, 1.000000000000000000, 0.000000000000000000 ) ) ;
#28970 = EDGE_CURVE ( 'NONE', #27456, #5322, #21627, .T. ) ;
#28969 = CARTESIAN_POINT ( 'NONE',  ( 3.235562306570555532E-30, 1.325223266901699007E-14, -67.50000000000000000 ) ) ;
#28971 = AXIS2_PLACEMENT_3D ( 'NONE', #35072, #10852, #16034 ) ;
#28972 = DIRECTION ( 'NONE',  ( 0.000000000000000000, 0.000000000000000000, -1.000000000000000000 ) ) ;
#28974 = CARTESIAN_POINT ( 'NONE',  ( 129.3530333899765594, -6.000000000000000000, 62.49999999999999289 ) ) ;
#28973 =( REPRESENTATION_RELATIONSHIP ('NONE','NONE', #23037, #15767 ) REPRESENTATION_RELATIONSHIP_WITH_TRANSFORMATION ( #5651 )SHAPE_REPRESENTATION_RELATIONSHIP( ) );
#28975 = DIRECTION ( 'NONE',  ( 0.000000000000000000, 0.000000000000000000, -1.000000000000000000 ) ) ;
#28976 = VERTEX_POINT ( 'NONE', #13481 ) ;
#28977 = EDGE_CURVE ( 'NONE', #17491, #5593, #29853, .T. ) ;
#28978 = CYLINDRICAL_SURFACE ( 'NONE', #12868, 3.999999999999976019 ) ;
#28979 = PLANE ( 'NONE',  #1252 ) ;
#28980 = FACE_OUTER_BOUND ( 'NONE', #19438, .T. ) ;
#28981 = ORIENTED_EDGE ( 'NONE', *, *, #926, .F. ) ;
#28982 = CARTESIAN_POINT ( 'NONE',  ( 2.789999999999999147, 20.79173593595296055, -22.27454621808740853 ) ) ;
#28983 = ORIENTED_EDGE ( 'NONE', *, *, #32376, .F. ) ;
#28984 = FACE_OUTER_BOUND ( 'NONE', #25603, .T. ) ;
#28985 = CARTESIAN_POINT ( 'NONE',  ( 0.5288002349688907255, -17.23487904370236734, -28.59786932736749421 ) ) ;
#28986 = AXIS2_PLACEMENT_3D ( 'NONE', #25623, #1254, #4074 ) ;
#28987 = DIRECTION ( 'NONE',  ( -0.000000000000000000, 1.836970198721029934E-16, -1.000000000000000000 ) ) ;
#28988 = CARTESIAN_POINT ( 'NONE',  ( 0.02407890056655564992, -0.3931553186911057041, -31.08824725498900676 ) ) ;
#28989 = CARTESIAN_POINT ( 'NONE',  ( -355.0000000000000000, 130.9999999999999716, 109.9999999999999858 ) ) ;
#28990 = ORIENTED_EDGE ( 'NONE', *, *, #31875, .F. ) ;
#28991 = VERTEX_POINT ( 'NONE', #30856 ) ;
#28992 = CARTESIAN_POINT ( 'NONE',  ( 773.9812636465261448, 1178.178243072741452, 1753.598338701303646 ) ) ;
#28993 = ORIENTED_EDGE ( 'NONE', *, *, #17549, .T. ) ;
#28994 = ADVANCED_FACE ( 'NONE', ( #25153 ), #16341, .F. ) ;
#28995 = EDGE_CURVE ( 'NONE', #13078, #3245, #22686, .T. ) ;
#28996 = DIRECTION ( 'NONE',  ( -0.3193015301359796165, 0.9476531711828025673, 0.000000000000000000 ) ) ;
#28997 = EDGE_CURVE ( 'NONE', #33799, #12627, #23347, .T. ) ;
#28998 = CARTESIAN_POINT ( 'NONE',  ( -12.25939112814508825, 30.14816249862101927, 68.31122994652405112 ) ) ;
#28999 = CARTESIAN_POINT ( 'NONE',  ( 19.99999999999998934, -137.0000000000000000, 174.9999999999999432 ) ) ;
#29000 = ORIENTED_EDGE ( 'NONE', *, *, #22135, .F. ) ;
#29001 = DIRECTION ( 'NONE',  ( 0.000000000000000000, 2.309213040847544338E-50, 1.000000000000000000 ) ) ;
#29002 = VECTOR ( 'NONE', #9262, 1000.000000000000000 ) ;
#29004 = DIRECTION ( 'NONE',  ( 0.000000000000000000, -0.000000000000000000, 1.000000000000000000 ) ) ;
#29003 = CARTESIAN_POINT ( 'NONE',  ( 2.265105769669975455, 26.54141775410149862, 20.24262527923012911 ) ) ;
#29005 = ORIENTED_EDGE ( 'NONE', *, *, #15508, .T. ) ;
#29006 = ORIENTED_EDGE ( 'NONE', *, *, #5873, .F. ) ;
#29007 = CARTESIAN_POINT ( 'NONE',  ( 2.719010690716784140, 21.26205330531154658, -23.50467731722535447 ) ) ;
#29008 = ORIENTED_EDGE ( 'NONE', *, *, #20071, .T. ) ;
#29009 = CARTESIAN_POINT ( 'NONE',  ( 0.000000000000000000, 3.524919873834583163E-15, 68.31122994652405112 ) ) ;
#29010 = CARTESIAN_POINT ( 'NONE',  ( -12.00000000000001066, -60.99999999999996447, -154.9999999999999716 ) ) ;
#29011 = EDGE_LOOP ( 'NONE', ( #17079, #4194 ) ) ;
#29012 = DIRECTION ( 'NONE',  ( 0.000000000000000000, -1.000000000000000000, -5.053935297177146739E-49 ) ) ;
#29013 = AXIS2_PLACEMENT_3D ( 'NONE', #16413, #193, #11232 ) ;
#29014 = ORIENTED_EDGE ( 'NONE', *, *, #19110, .T. ) ;
#29015 = CARTESIAN_POINT ( 'NONE',  ( 2.789999999999999147, 0.000000000000000000, 0.000000000000000000 ) ) ;
#29016 = CARTESIAN_POINT ( 'NONE',  ( -7.218132304338721994, -1.866624223957557671, 0.000000000000000000 ) ) ;
#29017 = LINE ( 'NONE', #31517, #32588 ) ;
#29019 = DIRECTION ( 'NONE',  ( 0.000000000000000000, 0.000000000000000000, 1.000000000000000000 ) ) ;
#29018 = PLANE ( 'NONE',  #11092 ) ;
#29020 = CARTESIAN_POINT ( 'NONE',  ( -20.00000000000001776, -137.0000000000000000, -194.9999999999999432 ) ) ;
#29021 = CARTESIAN_POINT ( 'NONE',  ( 0.000000000000000000, 33.69708579775584667, 49.43553178847298568 ) ) ;
#29022 = CARTESIAN_POINT ( 'NONE',  ( 1.040000000000000702, -10.37741591188916779, 32.81304455236864470 ) ) ;
#29023 = CIRCLE ( 'NONE', #3461, 7.999999999999979572 ) ;
#29024 = CARTESIAN_POINT ( 'NONE',  ( -15.99999999999998579, -112.9999999999999858, -155.0000000000000284 ) ) ;
#29025 = AXIS2_PLACEMENT_3D ( 'NONE', #1389, #33424, #8866 ) ;
#29026 = EDGE_LOOP ( 'NONE', ( #30757, #17200, #2793, #9254 ) ) ;
#29027 = ORIENTED_EDGE ( 'NONE', *, *, #858, .T. ) ;
#29028 = VERTEX_POINT ( 'NONE', #22503 ) ;
#29029 = ADVANCED_FACE ( 'NONE', ( #7952 ), #25332, .F. ) ;
#29030 = EDGE_CURVE ( 'NONE', #5316, #21613, #27173, .T. ) ;
#29031 = VECTOR ( 'NONE', #3269, 1000.000000000000000 ) ;
#29032 = CARTESIAN_POINT ( 'NONE',  ( 1.039999999999999813, 14.89726405156260114, -31.02351007835961383 ) ) ;
#29033 = VECTOR ( 'NONE', #27142, 1000.000000000000227 ) ;
#29034 = ORIENTED_EDGE ( 'NONE', *, *, #10081, .F. ) ;
#29035 = VECTOR ( 'NONE', #23781, 1000.000000000000000 ) ;
#29036 = VERTEX_POINT ( 'NONE', #11837 ) ;
#29037 = ORIENTED_EDGE ( 'NONE', *, *, #7655, .F. ) ;
#29038 = EDGE_CURVE ( 'NONE', #30641, #7395, #24319, .T. ) ;
#29039 = CARTESIAN_POINT ( 'NONE',  ( 26.97014235612466493, -26.57093094961043889, 68.31122994652405112 ) ) ;
#29040 = VERTEX_POINT ( 'NONE', #9136 ) ;
#29041 = CARTESIAN_POINT ( 'NONE',  ( -117.4999999999997442, 0.000000000000000000, 0.000000000000000000 ) ) ;
#29042 = FACE_BOUND ( 'NONE', #6826, .T. ) ;
#29043 = EDGE_LOOP ( 'NONE', ( #12118, #7781, #1866, #27154 ) ) ;
#29044 = ORIENTED_EDGE ( 'NONE', *, *, #10371, .F. ) ;
#29045 = DIRECTION ( 'NONE',  ( 0.000000000000000000, 0.000000000000000000, -1.000000000000000000 ) ) ;
#29047 = CARTESIAN_POINT ( 'NONE',  ( 0.000000000000000000, 0.000000000000000000, 0.000000000000000000 ) ) ;
#29046 = AXIS2_PLACEMENT_3D ( 'NONE', #28880, #4480, #15372 ) ;
#29048 = EDGE_CURVE ( 'NONE', #26364, #19238, #14145, .T. ) ;
#29049 = DIRECTION ( 'NONE',  ( 1.000000000000000000, 0.000000000000000000, 0.000000000000000000 ) ) ;
#29050 = CARTESIAN_POINT ( 'NONE',  ( 0.1835381919199922940, 14.82544181992975396, 28.66416816974143345 ) ) ;
#29051 = DIRECTION ( 'NONE',  ( -0.000000000000000000, 5.053935297177146739E-49, 1.000000000000000000 ) ) ;
#29052 = ORIENTED_EDGE ( 'NONE', *, *, #6022, .F. ) ;
#29053 = VECTOR ( 'NONE', #33916, 1000.000000000000000 ) ;
#29054 = DIRECTION ( 'NONE',  ( 0.000000000000000000, -0.000000000000000000, 1.000000000000000000 ) ) ;
#29055 = CARTESIAN_POINT ( 'NONE',  ( 29.83064097883987742, 23.32756518004832813, 68.31122994652405112 ) ) ;
#29056 = VERTEX_POINT ( 'NONE', #33167 ) ;
#29057 = DIRECTION ( 'NONE',  ( 0.000000000000000000, 2.465190328815661892E-32, 1.000000000000000000 ) ) ;
#29058 = DIRECTION ( 'NONE',  ( -0.000000000000000000, 1.000000000000000000, -0.000000000000000000 ) ) ;
#29059 = CARTESIAN_POINT ( 'NONE',  ( 108.4984947220250291, 4.562308164568303681, -5.958384794357583836 ) ) ;
#29061 = DIRECTION ( 'NONE',  ( -1.000000000000000000, -0.000000000000000000, -0.000000000000000000 ) ) ;
#29060 = CARTESIAN_POINT ( 'NONE',  ( -29.68486519896224962, 23.49918569563710946, 68.31122994652405112 ) ) ;
#29062 = AXIS2_PLACEMENT_3D ( 'NONE', #28325, #14807, #18014 ) ;
#29063 = CIRCLE ( 'NONE', #673, 22.50000000000000355 ) ;
#29064 = LINE ( 'NONE', #4324, #1925 ) ;
#29066 = ORIENTED_EDGE ( 'NONE', *, *, #12755, .T. ) ;
#29065 = AXIS2_PLACEMENT_3D ( 'NONE', #23788, #7930, #10791 ) ;
#29068 =( GEOMETRIC_REPRESENTATION_CONTEXT ( 3 ) GLOBAL_UNCERTAINTY_ASSIGNED_CONTEXT ( ( #3584 ) ) GLOBAL_UNIT_ASSIGNED_CONTEXT ( ( #34719, #10332, #31681 ) ) REPRESENTATION_CONTEXT ( 'NONE', 'WORKASPACE' ) );
#29067 = CARTESIAN_POINT ( 'NONE',  ( 105.3784337476560040, 5.728791326347600688, -11.10996872791849199 ) ) ;
#29070 = CARTESIAN_POINT ( 'NONE',  ( -418.0000000000000000, -105.0000000000000142, -69.99999999999998579 ) ) ;
#29069 = CARTESIAN_POINT ( 'NONE',  ( 7.699999999999998401, 0.000000000000000000, 0.000000000000000000 ) ) ;
#29071 = ORIENTED_EDGE ( 'NONE', *, *, #27807, .F. ) ;
#29072 = CARTESIAN_POINT ( 'NONE',  ( 0.02407890056655651728, -15.32140196853772984, 27.05343472112986092 ) ) ;
#29073 = ORIENTED_EDGE ( 'NONE', *, *, #24986, .F. ) ;
#29074 = ADVANCED_FACE ( 'NONE', ( #19667 ), #30512, .T. ) ;
#29075 = AXIS2_PLACEMENT_3D ( 'NONE', #31712, #12177, #6802 ) ;
#29076 = ORIENTED_EDGE ( 'NONE', *, *, #16893, .T. ) ;
#29077 = CARTESIAN_POINT ( 'NONE',  ( 0.000000000000000000, 0.000000000000000000, 4.679999999999999716 ) ) ;
#29078 = ORIENTED_EDGE ( 'NONE', *, *, #26819, .T. ) ;
#29079 = ORIENTED_EDGE ( 'NONE', *, *, #30128, .F. ) ;
#29080 = EDGE_CURVE ( 'NONE', #7524, #23016, #29607, .T. ) ;
#29081 = CARTESIAN_POINT ( 'NONE',  ( 2.773602559888816987, 28.19409568634637964, -12.86837344186502818 ) ) ;
#29082 = PRODUCT_DEFINITION_SHAPE ( 'NONE', 'NONE',  #35159 ) ;
#29083 = EDGE_CURVE ( 'NONE', #27224, #24780, #18263, .T. ) ;
#29084 = AXIS2_PLACEMENT_3D ( 'NONE', #8897, #17106, #27939 ) ;
#29085 = DIRECTION ( 'NONE',  ( 1.000000000000000000, 0.000000000000000000, 0.000000000000000000 ) ) ;
#29086 = VECTOR ( 'NONE', #27575, 1000.000000000000000 ) ;
#29087 = DIRECTION ( 'NONE',  ( 0.7960930657056433102, 0.6051742151937656855, 0.000000000000000000 ) ) ;
#29088 = EDGE_CURVE ( 'NONE', #8531, #15586, #1653, .T. ) ;
#29089 = ORIENTED_EDGE ( 'NONE', *, *, #3327, .T. ) ;
#29090 = EDGE_CURVE ( 'NONE', #16627, #29871, #28708, .T. ) ;
#29091 = ORIENTED_EDGE ( 'NONE', *, *, #14831, .F. ) ;
#29092 = AXIS2_PLACEMENT_3D ( 'NONE', #2069, #14916, #1377 ) ;
#29093 = DIRECTION ( 'NONE',  ( -0.000000000000000000, 1.836970198721029934E-16, -1.000000000000000000 ) ) ;
#29094 = CARTESIAN_POINT ( 'NONE',  ( 0.000000000000000000, 25.67797970382135375, 16.40405592474768426 ) ) ;
#29095 = CIRCLE ( 'NONE', #33643, 3.999999999999976019 ) ;
#29096 = FACE_OUTER_BOUND ( 'NONE', #20212, .T. ) ;
#29097 = EDGE_CURVE ( 'NONE', #8552, #17675, #31376, .T. ) ;
#29098 = DIRECTION ( 'NONE',  ( 0.3701381553399132329, 0.9289767198167918627, -0.000000000000000000 ) ) ;
#29099 = DIRECTION ( 'NONE',  ( 1.000000000000000000, 0.000000000000000000, -0.000000000000000000 ) ) ;
#29100 = UNCERTAINTY_MEASURE_WITH_UNIT (LENGTH_MEASURE( 1.000000000000000082E-05 ), #16721, 'distance_accuracy_value', 'NONE');
#29101 = VERTEX_POINT ( 'NONE', #12704 ) ;
#29102 = ORIENTED_EDGE ( 'NONE', *, *, #22595, .T. ) ;
#29103 = CARTESIAN_POINT ( 'NONE',  ( 143.0000000000000568, -85.49999999999998579, 63.00000000000000000 ) ) ;
#29104 = DIRECTION ( 'NONE',  ( 1.000000000000000000, 0.000000000000000000, 0.000000000000000000 ) ) ;
#29105 = ORIENTED_EDGE ( 'NONE', *, *, #29895, .T. ) ;
#29106 = DIRECTION ( 'NONE',  ( 0.000000000000000000, -1.000000000000000000, -1.131431318426415506E-52 ) ) ;
#29107 = CARTESIAN_POINT ( 'NONE',  ( 145.0000000000000568, -175.8248315648716016, -46.05325008164005851 ) ) ;
#29108 = FACE_OUTER_BOUND ( 'NONE', #20474, .T. ) ;
#29109 = ORIENTED_EDGE ( 'NONE', *, *, #27770, .F. ) ;
#29110 = CYLINDRICAL_SURFACE ( 'NONE', #17792, 16.19999999999999929 ) ;
#29111 = ORIENTED_EDGE ( 'NONE', *, *, #4717, .T. ) ;
#29112 = DIRECTION ( 'NONE',  ( 0.000000000000000000, 0.000000000000000000, 1.000000000000000000 ) ) ;
#29113 = ORIENTED_EDGE ( 'NONE', *, *, #22413, .T. ) ;
#29115 = CARTESIAN_POINT ( 'NONE',  ( 0.000000000000000000, 2.281310696040539424E-14, -36.68877005347592757 ) ) ;
#29114 = SURFACE_SIDE_STYLE ('',( #12937 ) ) ;
#29116 = CARTESIAN_POINT ( 'NONE',  ( -108.8519183384634061, 3.381649300054699214, 12.03636906590513078 ) ) ;
#29117 = B_SPLINE_CURVE_WITH_KNOTS ( 'NONE', 3,
 ( #17258, #15278, #20604, #33956, #12084, #15101 ),
 .UNSPECIFIED., .F., .F.,
 ( 4, 2, 4 ),
 ( 2.036796643444265524E-07, 0.001873401978039416615, 0.003746600276414489058 ),
 .UNSPECIFIED. ) ;
#29118 = AXIS2_PLACEMENT_3D ( 'NONE', #28073, #12726, #15566 ) ;
#29120 = ORIENTED_EDGE ( 'NONE', *, *, #11534, .T. ) ;
#29119 = AXIS2_PLACEMENT_3D ( 'NONE', #23041, #6468, #14513 ) ;
#29121 = AXIS2_PLACEMENT_3D ( 'NONE', #35004, #4899, #5426 ) ;
#29122 = DIRECTION ( 'NONE',  ( 0.000000000000000000, 1.310824597558155437E-49, 1.000000000000000000 ) ) ;
#29123 = DIRECTION ( 'NONE',  ( 0.000000000000000000, 2.309213040847544338E-50, 1.000000000000000000 ) ) ;
#29124 = ORIENTED_EDGE ( 'NONE', *, *, #11981, .F. ) ;
#29125 = CARTESIAN_POINT ( 'NONE',  ( 767.7573892341928286, 1236.346186647595232, 1753.598338701303419 ) ) ;
#29126 = EDGE_LOOP ( 'NONE', ( #18775, #772, #30204, #18087 ) ) ;
#29127 = CARTESIAN_POINT ( 'NONE',  ( 2.765921099433441555, -0.3931553186911057041, -31.08824725498900676 ) ) ;
#29128 = VERTEX_POINT ( 'NONE', #20189 ) ;
#29129 = CARTESIAN_POINT ( 'NONE',  ( 2.783107615553614078, -15.15194214258576011, -26.89541087693596211 ) ) ;
#29130 = CARTESIAN_POINT ( 'NONE',  ( 12.00000000000001066, 144.9999999999999716, 155.0000000000000000 ) ) ;
#29131 = DIRECTION ( 'NONE',  ( 1.000000000000000000, 0.000000000000000000, 0.000000000000000000 ) ) ;
#29132 = CARTESIAN_POINT ( 'NONE',  ( -19.99999999999998934, 144.9999999999999716, 162.9999999999999716 ) ) ;
#29133 = CONTEXT_DEPENDENT_SHAPE_REPRESENTATION ( #17872, #14886 ) ;
#29134 = EDGE_CURVE ( 'NONE', #20735, #17606, #25508, .T. ) ;
#29135 = ORIENTED_EDGE ( 'NONE', *, *, #19549, .T. ) ;
#29136 = EDGE_CURVE ( 'NONE', #173, #34313, #34146, .T. ) ;
#29137 = VERTEX_POINT ( 'NONE', #20361 ) ;
#29138 = VERTEX_POINT ( 'NONE', #14684 ) ;
#29139 = CARTESIAN_POINT ( 'NONE',  ( 0.000000000000000000, 0.000000000000000000, 20.00000000000000000 ) ) ;
#29140 = CARTESIAN_POINT ( 'NONE',  ( 12.00000000000003908, -115.0000000000000000, -158.9999999999999716 ) ) ;
#29141 =( GEOMETRIC_REPRESENTATION_CONTEXT ( 3 ) GLOBAL_UNCERTAINTY_ASSIGNED_CONTEXT ( ( #16059 ) ) GLOBAL_UNIT_ASSIGNED_CONTEXT ( ( #29921, #11053, #4990 ) ) REPRESENTATION_CONTEXT ( 'NONE', 'WORKASPACE' ) );
#29142 = LINE ( 'NONE', #13316, #24150 ) ;
#29144 = CARTESIAN_POINT ( 'NONE',  ( -19.99999999999998934, 4.559999999999908127, 172.9900000000000091 ) ) ;
#29143 = B_SPLINE_CURVE_WITH_KNOTS ( 'NONE', 3,
 ( #7423, #2266, #15464, #7598, #20796, #18318 ),
 .UNSPECIFIED., .F., .F.,
 ( 4, 2, 4 ),
 ( 4.404817164049666791E-07, 0.001874269726455598173, 0.003748098971194791310 ),
 .UNSPECIFIED. ) ;
#29145 = CIRCLE ( 'NONE', #13805, 9.999999999999998224 ) ;
#29146 = AXIS2_PLACEMENT_3D ( 'NONE', #8232, #31906, #4852 ) ;
#29147 = LINE ( 'NONE', #10278, #13461 ) ;
#29148 = VECTOR ( 'NONE', #23935, 1000.000000000000000 ) ;
#29149 = DIRECTION ( 'NONE',  ( 0.000000000000000000, 0.000000000000000000, 1.000000000000000000 ) ) ;
#29150 = ORIENTED_EDGE ( 'NONE', *, *, #19374, .F. ) ;
#29151 = CARTESIAN_POINT ( 'NONE',  ( 0.7564103408419841079, -24.35732449877335881, -23.60053042972057824 ) ) ;
#29152 = CARTESIAN_POINT ( 'NONE',  ( 99.77797576327679963, 2.385570507987203825, 12.27149918290385244 ) ) ;
#29153 = EDGE_CURVE ( 'NONE', #35009, #10400, #15021, .T. ) ;
#29154 = PLANE ( 'NONE',  #14915 ) ;
#29155 = ORIENTED_EDGE ( 'NONE', *, *, #16645, .F. ) ;
#29156 = SHAPE_REPRESENTATION ( 'motor shaft', ( #28566 ), #30284 ) ;
#29157 = CARTESIAN_POINT ( 'NONE',  ( 0.5328044427895346491, -5.227541351202838804, -13.49999999999999822 ) ) ;
#29158 = ORIENTED_EDGE ( 'NONE', *, *, #3903, .T. ) ;
#29159 = LINE ( 'NONE', #26487, #25096 ) ;
#29160 = EDGE_CURVE ( 'NONE', #13520, #7154, #25684, .T. ) ;
#29161 = CARTESIAN_POINT ( 'NONE',  ( 0.000000000000000000, 0.000000000000000000, 3.180000000000000160 ) ) ;
#29162 = EDGE_CURVE ( 'NONE', #22441, #19038, #20871, .T. ) ;
#29163 = ADVANCED_FACE ( 'NONE', ( #1139 ), #28368, .T. ) ;
#29164 = AXIS2_PLACEMENT_3D ( 'NONE', #31727, #18402, #26567 ) ;
#29165 = ORIENTED_EDGE ( 'NONE', *, *, #15825, .T. ) ;
#29166 = CARTESIAN_POINT ( 'NONE',  ( -9.978866888775733912, -11.61907005722761177, -87.50000000000000000 ) ) ;
#29167 = DIRECTION ( 'NONE',  ( 1.000000000000000000, 0.000000000000000000, 0.000000000000000000 ) ) ;
#29168 = DIRECTION ( 'NONE',  ( 0.000000000000000000, 0.000000000000000000, -1.000000000000000000 ) ) ;
#29169 = EDGE_CURVE ( 'NONE', #12730, #21780, #55, .T. ) ;
#29170 = ORIENTED_EDGE ( 'NONE', *, *, #21886, .T. ) ;
#29171 = AXIS2_PLACEMENT_3D ( 'NONE', #28992, #28308, #7622 ) ;
#29172 = EDGE_LOOP ( 'NONE', ( #5093, #9480, #33449, #15578 ) ) ;
#29173 = VECTOR ( 'NONE', #21503, 1000.000000000000000 ) ;
#29174 = DIRECTION ( 'NONE',  ( -7.044735254993868097E-14, 2.921932232757580011E-14, 0.9999999999999998890 ) ) ;
#29175 = TOROIDAL_SURFACE ( 'NONE', #30306, 30.47050528711512030, 8.000000000000000000 ) ;
#29176 = ORIENTED_EDGE ( 'NONE', *, *, #3849, .T. ) ;
#29177 = CARTESIAN_POINT ( 'NONE',  ( -499.9999999999999432, 112.9999999999999574, -187.0000000000000000 ) ) ;
#29178 = DIRECTION ( 'NONE',  ( -0.000000000000000000, 1.836970198721029934E-16, -1.000000000000000000 ) ) ;
#29179 = FACE_OUTER_BOUND ( 'NONE', #1526, .T. ) ;
#29180 = CONTEXT_DEPENDENT_SHAPE_REPRESENTATION ( #10789, #15221 ) ;
#29181 = EDGE_CURVE ( 'NONE', #13343, #4555, #3960, .T. ) ;
#29182 = APPLICATION_CONTEXT ( 'automotive_design' ) ;
#29183 = ORIENTED_EDGE ( 'NONE', *, *, #28007, .F. ) ;
#29184 = CARTESIAN_POINT ( 'NONE',  ( 5.021133111224162171, -25.61315202898005694, -87.50000000000000000 ) ) ;
#29185 = AXIS2_PLACEMENT_3D ( 'NONE', #33481, #24932, #399 ) ;
#29187 = CARTESIAN_POINT ( 'NONE',  ( 22.10765473302597073, -14.55883922869198344, -77.50000000000000000 ) ) ;
#29186 = CARTESIAN_POINT ( 'NONE',  ( -6.500000000000000000, 0.000000000000000000, -0.7500000000000000000 ) ) ;
#29188 = ORIENTED_EDGE ( 'NONE', *, *, #11333, .T. ) ;
#29189 = ORIENTED_EDGE ( 'NONE', *, *, #7251, .T. ) ;
#29190 = CARTESIAN_POINT ( 'NONE',  ( 5.713835024271039842, 32.03991982186465748, 68.31122994652405112 ) ) ;
#29191 = VERTEX_POINT ( 'NONE', #12521 ) ;
#29192 = CARTESIAN_POINT ( 'NONE',  ( 10.17231796313411429, 13.56412600238610189, -77.50000000000000000 ) ) ;
#29193 = CARTESIAN_POINT ( 'NONE',  ( -418.0000000000000000, 105.0000000000000142, 194.9999999999999716 ) ) ;
#29194 = VERTEX_POINT ( 'NONE', #34047 ) ;
#29195 = AXIS2_PLACEMENT_3D ( 'NONE', #21207, #23870, #2164 ) ;
#29196 = CYLINDRICAL_SURFACE ( 'NONE', #24241, 4.000000000000003553 ) ;
#29197 = CIRCLE ( 'NONE', #23500, 3.999999999999976019 ) ;
#29198 = B_SPLINE_CURVE_WITH_KNOTS ( 'NONE', 3,
 ( #14268, #30458, #31162, #19785, #19612, #9266, #22797, #27954, #3389, #33115, #20132, #912, #9454, #27778, #1261, #11780, #22630, #8731, #33647, #556, #33469, #17487, #19956, #6761, #22271, #30808, #28137, #28317, #6585, #733, #3908, #14800, #25627, #11411, #12130, #22971, #6050, #33826, #25098, #23320 ),
 .UNSPECIFIED., .F., .F.,
 ( 4, 2, 2, 2, 2, 2, 2, 2, 2, 2, 2, 2, 2, 2, 2, 2, 2, 2, 2, 4 ),
 ( 0.01617148595533311056, 0.01667647242675793923, 0.01718145889818276789, 0.01819143184103242522, 0.01869641831245725735, 0.01920140478388208602, 0.02021137772673176763, 0.02122135066958145272, 0.02223132361243113433, 0.02324129655528081595, 0.02425126949813049756, 0.02526124244098017918, 0.02627121538382986080, 0.02728118832667954241, 0.02829116126952922403, 0.02879614774095407698, 0.02930113421237893340, 0.03031110715522863930, 0.03132108009807835214, 0.03233105304092805804 ),
 .UNSPECIFIED. ) ;
#29199 = VECTOR ( 'NONE', #9250, 1000.000000000000000 ) ;
#29200 = PRODUCT_DEFINITION_SHAPE ( 'NONE', 'NONE',  #35221 ) ;
#29201 = EDGE_LOOP ( 'NONE', ( #23712, #5528, #8884, #18244 ) ) ;
#29202 = EDGE_CURVE ( 'NONE', #5838, #18998, #9664, .T. ) ;
#29203 = LINE ( 'NONE', #26701, #18060 ) ;
#29204 = DIRECTION ( 'NONE',  ( 0.000000000000000000, -1.310824597558155437E-49, -1.000000000000000000 ) ) ;
#29205 = FACE_OUTER_BOUND ( 'NONE', #28950, .T. ) ;
#29206 = EDGE_CURVE ( 'NONE', #27900, #18998, #28879, .T. ) ;
#29208 = LINE ( 'NONE', #34366, #4285 ) ;
#29207 = DIRECTION ( 'NONE',  ( -1.000000000000000000, -0.000000000000000000, -0.000000000000000000 ) ) ;
#29209 = EDGE_CURVE ( 'NONE', #32109, #24914, #26037, .T. ) ;
#29210 = CARTESIAN_POINT ( 'NONE',  ( 12.00000000000001066, -134.9999999999999716, 162.9999999999999716 ) ) ;
#29211 = DIRECTION ( 'NONE',  ( 1.000000000000000000, 0.000000000000000000, 0.000000000000000000 ) ) ;
#29212 = CARTESIAN_POINT ( 'NONE',  ( 2.897437953906695165E-16, -0.2191908000481288532, 30.66081142815914973 ) ) ;
#29213 = DIRECTION ( 'NONE',  ( 1.000000000000000000, 0.000000000000000000, 0.000000000000000000 ) ) ;
#29214 = AXIS2_PLACEMENT_3D ( 'NONE', #2773, #23955, #12954 ) ;
#29215 = ORIENTED_EDGE ( 'NONE', *, *, #16942, .F. ) ;
#29216 = DIRECTION ( 'NONE',  ( 7.283623369766538980E-15, -7.009213243398816248E-15, 0.9999999999999998890 ) ) ;
#29217 = ORIENTED_EDGE ( 'NONE', *, *, #23244, .T. ) ;
#29218 = EDGE_LOOP ( 'NONE', ( #6184, #19061, #13162, #14958 ) ) ;
#29219 = CARTESIAN_POINT ( 'NONE',  ( 2.606461977389332940, 19.62374805819733581, 25.61906966869699431 ) ) ;
#29220 = AXIS2_PLACEMENT_3D ( 'NONE', #31688, #34368, #12849 ) ;
#29221 = LINE ( 'NONE', #13212, #11955 ) ;
#29222 = DIRECTION ( 'NONE',  ( 0.000000000000000000, 0.000000000000000000, 1.000000000000000000 ) ) ;
#29223 = ORIENTED_EDGE ( 'NONE', *, *, #18375, .T. ) ;
#29224 = EDGE_LOOP ( 'NONE', ( #33800, #15258, #25231, #588 ) ) ;
#29225 = DIRECTION ( 'NONE',  ( 1.000000000000000000, 0.000000000000000000, -0.000000000000000000 ) ) ;
#29226 = CARTESIAN_POINT ( 'NONE',  ( 8.000000000000000000, 0.000000000000000000, 0.000000000000000000 ) ) ;
#29227 = VECTOR ( 'NONE', #29178, 1000.000000000000000 ) ;
#29228 = LINE ( 'NONE', #4824, #15859 ) ;
#29229 = CARTESIAN_POINT ( 'NONE',  ( 2.789999999999999147, 17.98401995359633077, 24.59729088254962548 ) ) ;
#29230 = VERTEX_POINT ( 'NONE', #23539 ) ;
#29231 = VERTEX_POINT ( 'NONE', #15371 ) ;
#29232 =( REPRESENTATION_RELATIONSHIP ('NONE','NONE', #23037, #28231 ) REPRESENTATION_RELATIONSHIP_WITH_TRANSFORMATION ( #1299 )SHAPE_REPRESENTATION_RELATIONSHIP( ) );
#29233 = CARTESIAN_POINT ( 'NONE',  ( 0.5248942108473680923, 5.490830290250059420, -32.92508943594307880 ) ) ;
#29234 = CARTESIAN_POINT ( 'NONE',  ( 2.787883829527677548, 27.86222219983571335, -12.86217335695008046 ) ) ;
#29235 = CARTESIAN_POINT ( 'NONE',  ( -105.0000000000000000, 0.000000000000000000, 60.00000000000000000 ) ) ;
#29236 = DIRECTION ( 'NONE',  ( 0.000000000000000000, 1.000000000000000000, 1.310824597558155437E-49 ) ) ;
#29237 = LINE ( 'NONE', #1485, #26793 ) ;
#29238 = ORIENTED_EDGE ( 'NONE', *, *, #18110, .F. ) ;
#29239 = CARTESIAN_POINT ( 'NONE',  ( -45.00000000000000000, 42.49491490430484220, -36.69637551990492597 ) ) ;
#29240 = DIRECTION ( 'NONE',  ( -1.000000000000000000, 0.000000000000000000, 0.000000000000000000 ) ) ;
#29241 = AXIS2_PLACEMENT_3D ( 'NONE', #33011, #27328, #28041 ) ;
#29242 = VECTOR ( 'NONE', #26153, 1000.000000000000000 ) ;
#29243 = DIRECTION ( 'NONE',  ( 0.000000000000000000, 0.000000000000000000, -1.000000000000000000 ) ) ;
#29244 = EDGE_CURVE ( 'NONE', #10045, #14714, #9838, .T. ) ;
#29245 = CARTESIAN_POINT ( 'NONE',  ( 2.789999999999999147, -29.69698570178027808, 11.75786841620004175 ) ) ;
#29246 = EDGE_CURVE ( 'NONE', #13296, #12696, #28431, .T. ) ;
#29247 = CARTESIAN_POINT ( 'NONE',  ( 110.1126341753765416, 2.611822472857947108, -7.032742872185955285 ) ) ;
#29248 = EDGE_CURVE ( 'NONE', #23973, #17221, #20703, .T. ) ;
#29250 = DIRECTION ( 'NONE',  ( 0.000000000000000000, 0.000000000000000000, 1.000000000000000000 ) ) ;
#29249 = CARTESIAN_POINT ( 'NONE',  ( 2.033800788961415140, 21.20694131899045942, 26.46705060818966260 ) ) ;
#29251 = ADVANCED_FACE ( 'NONE', ( #31719 ), #7326, .T. ) ;
#29252 = CIRCLE ( 'NONE', #24682, 1.999999999999999556 ) ;
#29253 = CYLINDRICAL_SURFACE ( 'NONE', #794, 4.750000000000004441 ) ;
#29254 = VERTEX_POINT ( 'NONE', #2344 ) ;
#29255 = PRODUCT_RELATED_PRODUCT_CATEGORY ( 'part', '', ( #5768 ) ) ;
#29256 = CARTESIAN_POINT ( 'NONE',  ( 99.44953031585586700, 1.503590720865120911, -12.41481623251361555 ) ) ;
#29258 = CARTESIAN_POINT ( 'NONE',  ( -1.059638217015129409E-14, 11.36060796471277001, -7.322849800245817775 ) ) ;
#29257 =( NAMED_UNIT ( * ) SI_UNIT ( $, .STERADIAN. ) SOLID_ANGLE_UNIT ( ) );
#29259 = ORIENTED_EDGE ( 'NONE', *, *, #31, .F. ) ;
#29260 = CARTESIAN_POINT ( 'NONE',  ( -12.00000000000001243, 134.9999999999999432, -154.9999999999999716 ) ) ;
#29261 = ORIENTED_EDGE ( 'NONE', *, *, #23739, .T. ) ;
#29262 = VECTOR ( 'NONE', #32101, 1000.000000000000000 ) ;
#29263 = ORIENTED_EDGE ( 'NONE', *, *, #24735, .F. ) ;
#29264 = DIRECTION ( 'NONE',  ( 0.000000000000000000, 0.000000000000000000, 1.000000000000000000 ) ) ;
#29265 = ORIENTED_EDGE ( 'NONE', *, *, #5677, .F. ) ;
#29266 = B_SPLINE_CURVE_WITH_KNOTS ( 'NONE', 3,
 ( #31194, #1467, #17859, #6793 ),
 .UNSPECIFIED., .F., .F.,
 ( 4, 4 ),
 ( 2.436748180515341377E-07, 0.0006879797535939411769 ),
 .UNSPECIFIED. ) ;
#29267 = VERTEX_POINT ( 'NONE', #29414 ) ;
#29268 = DIRECTION ( 'NONE',  ( -0.000000000000000000, -1.000000000000000000, -0.000000000000000000 ) ) ;
#29269 = AXIS2_PLACEMENT_3D ( 'NONE', #28969, #20615, #12273 ) ;
#29270 = CARTESIAN_POINT ( 'NONE',  ( -12.00000000000001066, 144.9999999999999716, 155.0000000000000000 ) ) ;
#29271 = VECTOR ( 'NONE', #20249, 1000.000000000000000 ) ;
#29272 = DIRECTION ( 'NONE',  ( -0.000000000000000000, -0.000000000000000000, -1.000000000000000000 ) ) ;
#29273 = DIRECTION ( 'NONE',  ( -0.000000000000000000, 1.000000000000000000, 0.000000000000000000 ) ) ;
#29274 = VERTEX_POINT ( 'NONE', #12882 ) ;
#29275 = ORIENTED_EDGE ( 'NONE', *, *, #26350, .F. ) ;
#29276 = AXIS2_PLACEMENT_3D ( 'NONE', #17638, #7086, #1759 ) ;
#29277 = CYLINDRICAL_SURFACE ( 'NONE', #19678, 16.19999999999999574 ) ;
#29278 = DIRECTION ( 'NONE',  ( -3.040835319149746090E-31, -1.000000000000000000, 0.000000000000000000 ) ) ;
#29279 = CYLINDRICAL_SURFACE ( 'NONE', #22057, 2.524999999999999467 ) ;
#29280 = CIRCLE ( 'NONE', #13944, 2.033421858999710619 ) ;
#29281 = FACE_OUTER_BOUND ( 'NONE', #10189, .T. ) ;
#29282 = DIRECTION ( 'NONE',  ( 1.000000000000000000, 0.000000000000000000, 0.000000000000000000 ) ) ;
#29283 = ORIENTED_EDGE ( 'NONE', *, *, #31959, .F. ) ;
#29284 = DIRECTION ( 'NONE',  ( -0.000000000000000000, -0.000000000000000000, 1.000000000000000000 ) ) ;
#29285 = DIRECTION ( 'NONE',  ( 0.000000000000000000, 0.000000000000000000, 1.000000000000000000 ) ) ;
#29286 = VERTEX_POINT ( 'NONE', #4648 ) ;
#29287 = EDGE_CURVE ( 'NONE', #6968, #20076, #15541, .T. ) ;
#29288 = CARTESIAN_POINT ( 'NONE',  ( 22.10765473302597073, -12.47301499840864025, -77.50000000000000000 ) ) ;
#29289 = DIRECTION ( 'NONE',  ( -0.000000000000000000, -1.836970198721029688E-16, 1.000000000000000000 ) ) ;
#29290 = EDGE_CURVE ( 'NONE', #30714, #12639, #23720, .T. ) ;
#29291 = CARTESIAN_POINT ( 'NONE',  ( 1.749999999999999778, -10.37741591188916424, 32.81304455236865181 ) ) ;
#29292 = VERTEX_POINT ( 'NONE', #5361 ) ;
#29293 = FACE_BOUND ( 'NONE', #27227, .T. ) ;
#29294 = EDGE_LOOP ( 'NONE', ( #15958, #10207, #7273, #1014 ) ) ;
#29295 = VECTOR ( 'NONE', #13041, 1000.000000000000000 ) ;
#29296 = VECTOR ( 'NONE', #5795, 1000.000000000000000 ) ;
#29297 = CARTESIAN_POINT ( 'NONE',  ( -35.00000000000000000, 16.36947364650383818, 36.69637551990492597 ) ) ;
#29298 = VERTEX_POINT ( 'NONE', #7504 ) ;
#29299 = EDGE_CURVE ( 'NONE', #11793, #19626, #23882, .T. ) ;
#29300 = CARTESIAN_POINT ( 'NONE',  ( -12.00000000000001066, 144.9999999999999716, 162.9999999999999716 ) ) ;
#29301 = VECTOR ( 'NONE', #8834, 1000.000000000000114 ) ;
#29302 = FACE_OUTER_BOUND ( 'NONE', #14946, .T. ) ;
#29303 = ORIENTED_EDGE ( 'NONE', *, *, #11773, .F. ) ;
#29304 = EDGE_CURVE ( 'NONE', #34809, #18790, #24053, .T. ) ;
#29305 = CIRCLE ( 'NONE', #1455, 32.54542015209055705 ) ;
#29306 = FACE_OUTER_BOUND ( 'NONE', #10581, .T. ) ;
#29307 = VECTOR ( 'NONE', #25897, 1000.000000000000000 ) ;
#29308 = PLANE ( 'NONE',  #5751 ) ;
#29309 = B_SPLINE_CURVE_WITH_KNOTS ( 'NONE', 3,
 ( #20087, #30930, #8512, #6001, #2985, #686 ),
 .UNSPECIFIED., .F., .F.,
 ( 4, 2, 4 ),
 ( 4.404817102045565444E-07, 0.001874269680285066582, 0.003748098878859928897 ),
 .UNSPECIFIED. ) ;
#29310 = ADVANCED_FACE ( 'NONE', ( #5180 ), #33, .T. ) ;
#29311 = ORIENTED_EDGE ( 'NONE', *, *, #1651, .F. ) ;
#29312 = EDGE_CURVE ( 'NONE', #32956, #10280, #32050, .T. ) ;
#29313 = DIRECTION ( 'NONE',  ( -0.1063910735369225230, 0.9943243633099118073, -1.000770725407345128E-14 ) ) ;
#29314 = ORIENTED_EDGE ( 'NONE', *, *, #3412, .F. ) ;
#29315 = CARTESIAN_POINT ( 'NONE',  ( 110.2199516832989730, -2.390228624448382799, 12.27061385718275943 ) ) ;
#29316 = EDGE_LOOP ( 'NONE', ( #32573, #4246, #17928, #32664 ) ) ;
#29317 = CARTESIAN_POINT ( 'NONE',  ( -35.55956070192387841, -17.65143121711728469, 5.690671783530174999 ) ) ;
#29318 =( NAMED_UNIT ( * ) SI_UNIT ( $, .STERADIAN. ) SOLID_ANGLE_UNIT ( ) );
#29319 = AXIS2_PLACEMENT_3D ( 'NONE', #9090, #6403, #24312 ) ;
#29320 = CARTESIAN_POINT ( 'NONE',  ( -345.0000000000000000, -125.0000000000000284, 168.9999999999999716 ) ) ;
#29321 = DIRECTION ( 'NONE',  ( -1.000000000000000000, 0.000000000000000000, -1.300283923313630633E-47 ) ) ;
#29322 = ITEM_DEFINED_TRANSFORMATION ( 'NONE', 'NONE', #18386,  #28566 ) ;
#29323 = VERTEX_POINT ( 'NONE', #31885 ) ;
#29324 = VERTEX_POINT ( 'NONE', #21579 ) ;
#29325 = ORIENTED_EDGE ( 'NONE', *, *, #11924, .T. ) ;
#29326 = CARTESIAN_POINT ( 'NONE',  ( -445.9999999999999432, -104.9999999999999858, -162.9999999999999716 ) ) ;
#29327 = VECTOR ( 'NONE', #26912, 1000.000000000000000 ) ;
#29328 = LINE ( 'NONE', #31977, #33060 ) ;
#29329 = FACE_OUTER_BOUND ( 'NONE', #19375, .T. ) ;
#29330 = CARTESIAN_POINT ( 'NONE',  ( -35.00000000000000000, 8.360858262960560339, 23.84547010402786427 ) ) ;
#29331 = CARTESIAN_POINT ( 'NONE',  ( -20.00000000000004619, -134.9999999999999716, -162.9999999999999432 ) ) ;
#29332 =( LENGTH_UNIT ( ) NAMED_UNIT ( * ) SI_UNIT ( .MILLI., .METRE. ) );
#29333 = ORIENTED_EDGE ( 'NONE', *, *, #20887, .T. ) ;
#29334 = CIRCLE ( 'NONE', #10586, 13.50000000000000178 ) ;
#29335 = CARTESIAN_POINT ( 'NONE',  ( 19.99999999999998934, -145.0000000000000000, -162.9999999999999432 ) ) ;
#29336 = FACE_OUTER_BOUND ( 'NONE', #12927, .T. ) ;
#29337 = DIRECTION ( 'NONE',  ( 0.000000000000000000, 1.000000000000000000, -6.123233995736766036E-17 ) ) ;
#29338 = ORIENTED_EDGE ( 'NONE', *, *, #23185, .F. ) ;
#29339 = CARTESIAN_POINT ( 'NONE',  ( 25.76952721012209224, 19.87802405277948736, 49.43553178847298568 ) ) ;
#29340 = ORIENTED_EDGE ( 'NONE', *, *, #25046, .T. ) ;
#29341 = CARTESIAN_POINT ( 'NONE',  ( -107.2773118281637039, 4.592153980832013538, -11.62674774045203208 ) ) ;
#29342 = EDGE_CURVE ( 'NONE', #15960, #15610, #34753, .T. ) ;
#29343 = DIRECTION ( 'NONE',  ( -0.7071067811865513475, 8.659560562354884787E-17, -0.7071067811865435759 ) ) ;
#29344 = AXIS2_PLACEMENT_3D ( 'NONE', #23025, #18051, #6982 ) ;
#29345 = VERTEX_POINT ( 'NONE', #10365 ) ;
#29346 = ADVANCED_FACE ( 'NONE', ( #32068 ), #26731, .F. ) ;
#29347 = EDGE_CURVE ( 'NONE', #5081, #11199, #13224, .T. ) ;
#29348 = DIRECTION ( 'NONE',  ( 0.000000000000000000, 0.000000000000000000, -1.000000000000000000 ) ) ;
#29349 = FACE_BOUND ( 'NONE', #3775, .T. ) ;
#29350 = CARTESIAN_POINT ( 'NONE',  ( 15.99999999999998579, -145.0000000000000000, -162.9999999999999432 ) ) ;
#29351 = AXIS2_PLACEMENT_3D ( 'NONE', #19448, #27615, #3229 ) ;
#29352 = ORIENTED_EDGE ( 'NONE', *, *, #19455, .T. ) ;
#29353 = VERTEX_POINT ( 'NONE', #18221 ) ;
#29354 = DIRECTION ( 'NONE',  ( 0.4341965393420280095, 0.9008181643502790603, 4.266700380305212277E-15 ) ) ;
#29355 = ORIENTED_EDGE ( 'NONE', *, *, #17469, .F. ) ;
#29356 = CIRCLE ( 'NONE', #14016, 1.649999999999999911 ) ;
#29357 = DIRECTION ( 'NONE',  ( 1.000000000000000000, 0.000000000000000000, 0.000000000000000000 ) ) ;
#29358 = ADVANCED_FACE ( 'NONE', ( #10896 ), #34938, .T. ) ;
#29359 = CARTESIAN_POINT ( 'NONE',  ( 1.040000000000000924, 0.000000000000000000, 0.000000000000000000 ) ) ;
#29360 = DIRECTION ( 'NONE',  ( 1.000000000000000000, 0.000000000000000000, -1.848892746611746966E-32 ) ) ;
#29361 = CARTESIAN_POINT ( 'NONE',  ( 106.9039025905678955, -5.425683864377651489, 5.182047996533464485 ) ) ;
#29362 = ORIENTED_EDGE ( 'NONE', *, *, #22508, .F. ) ;
#29363 = DIRECTION ( 'NONE',  ( 1.000000000000000000, 0.000000000000000000, 0.000000000000000000 ) ) ;
#29364 = EDGE_CURVE ( 'NONE', #27823, #245, #8661, .T. ) ;
#29365 = EDGE_CURVE ( 'NONE', #1870, #28564, #28465, .T. ) ;
#29366 = VECTOR ( 'NONE', #33121, 1000.000000000000000 ) ;
#29368 = FACE_OUTER_BOUND ( 'NONE', #20286, .T. ) ;
#29367 = CARTESIAN_POINT ( 'NONE',  ( -5.021133111224679091, 28.08988295778447508, -67.50000000000000000 ) ) ;
#29369 = EDGE_CURVE ( 'NONE', #26816, #34740, #8558, .T. ) ;
#29370 = VERTEX_POINT ( 'NONE', #10194 ) ;
#29371 = EDGE_LOOP ( 'NONE', ( #6190, #5954, #1166, #3876 ) ) ;
#29372 = DIRECTION ( 'NONE',  ( -0.000000000000000000, -1.836970198721029688E-16, 1.000000000000000000 ) ) ;
#29373 = ORIENTED_EDGE ( 'NONE', *, *, #10170, .T. ) ;
#29374 = EDGE_CURVE ( 'NONE', #6935, #17160, #13572, .T. ) ;
#29375 = DIRECTION ( 'NONE',  ( 0.000000000000000000, 0.000000000000000000, 1.000000000000000000 ) ) ;
#29376 = DIRECTION ( 'NONE',  ( 0.7071067811865512365, 8.659560562354889717E-17, 0.7071067811865439090 ) ) ;
#29377 = ORIENTED_EDGE ( 'NONE', *, *, #29780, .T. ) ;
#29378 = LINE ( 'NONE', #32216, #24316 ) ;
#29379 = DIRECTION ( 'NONE',  ( 0.000000000000000000, -1.000000000000000000, 0.000000000000000000 ) ) ;
#29380 = ORIENTED_EDGE ( 'NONE', *, *, #8435, .F. ) ;
#29381 = CIRCLE ( 'NONE', #26450, 4.682234377621698584 ) ;
#29382 = CARTESIAN_POINT ( 'NONE',  ( 11.99999999999999645, 134.9999999999998863, 162.9999999999999716 ) ) ;
#29383 = CARTESIAN_POINT ( 'NONE',  ( 5.021133111224265200, -15.68591377522703390, -87.50000000000000000 ) ) ;
#29385 = DIRECTION ( 'NONE',  ( 0.000000000000000000, 0.000000000000000000, 1.000000000000000000 ) ) ;
#29384 = CARTESIAN_POINT ( 'NONE',  ( 145.0000000000000568, -87.50000000000000000, 65.00000000000000000 ) ) ;
#29386 = EDGE_CURVE ( 'NONE', #2950, #6306, #14234, .T. ) ;
#29387 = EDGE_CURVE ( 'NONE', #17403, #19022, #18915, .T. ) ;
#29388 = DIRECTION ( 'NONE',  ( -0.000000000000000000, -1.000000000000000000, -0.000000000000000000 ) ) ;
#29389 = LINE ( 'NONE', #12677, #5933 ) ;
#29390 = DIRECTION ( 'NONE',  ( 0.000000000000000000, 0.000000000000000000, -1.000000000000000000 ) ) ;
#29391 = CIRCLE ( 'NONE', #14048, 3.999999999999976019 ) ;
#29392 = CIRCLE ( 'NONE', #969, 7.999999999999979572 ) ;
#29393 = CIRCLE ( 'NONE', #486, 11.22499999999999787 ) ;
#29394 = B_SPLINE_CURVE_WITH_KNOTS ( 'NONE', 3,
 ( #4147, #15208, #12369, #12198 ),
 .UNSPECIFIED., .F., .F.,
 ( 4, 4 ),
 ( 0.005298392425857880068, 0.005985260475359764631 ),
 .UNSPECIFIED. ) ;
#29395 = EDGE_LOOP ( 'NONE', ( #29555, #5202, #28953, #1983 ) ) ;
#29396 = DIRECTION ( 'NONE',  ( -7.179331560892316428E-15, 7.104906041323685364E-15, -0.9999999999999998890 ) ) ;
#29397 = EDGE_LOOP ( 'NONE', ( #28060, #1187, #4175, #13996, #26764, #28809, #31713 ) ) ;
#29398 = ORIENTED_EDGE ( 'NONE', *, *, #3652, .T. ) ;
#29399 = CARTESIAN_POINT ( 'NONE',  ( -31.87924797510909869, -6.551177101682124970, 68.31122994652405112 ) ) ;
#29400 = DIRECTION ( 'NONE',  ( 0.000000000000000000, -1.000000000000000000, 0.000000000000000000 ) ) ;
#29401 = ORIENTED_EDGE ( 'NONE', *, *, #21472, .T. ) ;
#29402 = VERTEX_POINT ( 'NONE', #24575 ) ;
#29403 = DIRECTION ( 'NONE',  ( 0.000000000000000000, 1.836970198721029441E-16, -1.000000000000000000 ) ) ;
#29404 = SURFACE_STYLE_FILL_AREA ( #7672 ) ;
#29405 = ADVANCED_FACE ( 'NONE', ( #14100 ), #16783, .F. ) ;
#29406 = ADVANCED_FACE ( 'NONE', ( #19624 ), #22107, .T. ) ;
#29407 = CARTESIAN_POINT ( 'NONE',  ( 1.394999999999999574, -33.26546734453813059, -8.820166447042129931 ) ) ;
#29408 = ORIENTED_EDGE ( 'NONE', *, *, #30005, .T. ) ;
#29409 = EDGE_LOOP ( 'NONE', ( #23351, #178, #16138, #3387, #18179 ) ) ;
#29410 = CARTESIAN_POINT ( 'NONE',  ( 23.93847777447631131, 22.04889236939138542, 49.43553178847298568 ) ) ;
#29411 = DIRECTION ( 'NONE',  ( 1.000000000000000000, 0.000000000000000000, 0.000000000000000000 ) ) ;
#29412 = EDGE_CURVE ( 'NONE', #30243, #32960, #24472, .T. ) ;
#29413 = CARTESIAN_POINT ( 'NONE',  ( -355.0000000000000000, 134.9999999999999716, 126.0000000000000000 ) ) ;
#29414 = CARTESIAN_POINT ( 'NONE',  ( -8.000000000000000000, 1.941065176648554701E-15, 15.69999999999999929 ) ) ;
#29415 = CARTESIAN_POINT ( 'NONE',  ( 11.62236370382047745, -30.39942490923500884, 68.31122994652405112 ) ) ;
#29416 = EDGE_LOOP ( 'NONE', ( #7408, #17557, #11745, #34529 ) ) ;
#29418 = CIRCLE ( 'NONE', #32803, 3.999999999999976019 ) ;
#29417 = CARTESIAN_POINT ( 'NONE',  ( -5.469264258321805627, 1.713938105891546382, 3.180000000000000160 ) ) ;
#29420 = LINE ( 'NONE', #2183, #31574 ) ;
#29419 = CIRCLE ( 'NONE', #19748, 3.999999999999976019 ) ;
#29421 = FACE_OUTER_BOUND ( 'NONE', #6739, .T. ) ;
#29422 = EDGE_CURVE ( 'NONE', #31845, #4999, #30467, .T. ) ;
#29423 = FACE_OUTER_BOUND ( 'NONE', #33005, .T. ) ;
#29424 = DIRECTION ( 'NONE',  ( 0.000000000000000000, 0.000000000000000000, -1.000000000000000000 ) ) ;
#29425 = CARTESIAN_POINT ( 'NONE',  ( -19.99999999999998934, -134.9999999999999716, 187.0000000000000000 ) ) ;
#29426 = CIRCLE ( 'NONE', #30546, 4.750000000000004441 ) ;
#29428 = CARTESIAN_POINT ( 'NONE',  ( -100.9340356286931097, 3.171022835462805389, -6.816853140736490957 ) ) ;
#29427 = DIRECTION ( 'NONE',  ( -1.000000000000000000, 0.000000000000000000, -0.000000000000000000 ) ) ;
#29429 = DIRECTION ( 'NONE',  ( 0.000000000000000000, 0.000000000000000000, -1.000000000000000000 ) ) ;
#29430 = VERTEX_POINT ( 'NONE', #24763 ) ;
#29431 = CARTESIAN_POINT ( 'NONE',  ( 110.2220242367232146, 2.385570507987203825, -12.27149918290385600 ) ) ;
#29433 = LINE ( 'NONE', #20548, #33905 ) ;
#29432 = CARTESIAN_POINT ( 'NONE',  ( -15.99999999999998579, 144.9999999999999716, 162.9999999999999716 ) ) ;
#29434 = VECTOR ( 'NONE', #32449, 1000.000000000000000 ) ;
#29435 = ORIENTED_EDGE ( 'NONE', *, *, #3654, .T. ) ;
#29436 = CARTESIAN_POINT ( 'NONE',  ( 2.765921099433442887, -23.70329957282599764, 20.11932597908820242 ) ) ;
#29437 = EDGE_CURVE ( 'NONE', #1125, #5515, #5885, .T. ) ;
#29438 = ORIENTED_EDGE ( 'NONE', *, *, #522, .F. ) ;
#29439 = AXIS2_PLACEMENT_3D ( 'NONE', #34941, #23723, #10557 ) ;
#29440 = VECTOR ( 'NONE', #27581, 1000.000000000000000 ) ;
#29441 =( REPRESENTATION_RELATIONSHIP ('NONE','NONE', #23037, #15767 ) REPRESENTATION_RELATIONSHIP_WITH_TRANSFORMATION ( #19044 )SHAPE_REPRESENTATION_RELATIONSHIP( ) );
#29442 = ORIENTED_EDGE ( 'NONE', *, *, #6730, .F. ) ;
#29443 = FACE_BOUND ( 'NONE', #17280, .T. ) ;
#29444 = ORIENTED_EDGE ( 'NONE', *, *, #27993, .F. ) ;
#29445 = ORIENTED_EDGE ( 'NONE', *, *, #22548, .T. ) ;
#29446 = DIRECTION ( 'NONE',  ( 0.000000000000000000, 1.131431318426415506E-52, 1.000000000000000000 ) ) ;
#29447 = EDGE_CURVE ( 'NONE', #35, #32367, #21090, .T. ) ;
#29448 = AXIS2_PLACEMENT_3D ( 'NONE', #30320, #28005, #14322 ) ;
#29449 = EDGE_CURVE ( 'NONE', #29973, #2835, #29941, .T. ) ;
#29450 = ADVANCED_FACE ( 'NONE', ( #21927 ), #19273, .F. ) ;
#29451 = CARTESIAN_POINT ( 'NONE',  ( 145.0000000000000568, 85.49999999999998579, 65.00000000000000000 ) ) ;
#29452 = CYLINDRICAL_SURFACE ( 'NONE', #29618, 4.000000000000003553 ) ;
#29453 = ORIENTED_EDGE ( 'NONE', *, *, #7789, .T. ) ;
#29454 = ORIENTED_EDGE ( 'NONE', *, *, #29290, .T. ) ;
#29455 = CARTESIAN_POINT ( 'NONE',  ( -442.0000000000000000, -105.0000000000000142, 155.0000000000000000 ) ) ;
#29456 = CARTESIAN_POINT ( 'NONE',  ( -32.71222340678873053, 19.07754906224035807, -36.68877005347593467 ) ) ;
#29457 = LINE ( 'NONE', #2560, #34549 ) ;
#29458 = CARTESIAN_POINT ( 'NONE',  ( 1.395000000000002238, -33.39989884085097316, 8.296590337300143503 ) ) ;
#29459 = DIRECTION ( 'NONE',  ( 0.000000000000000000, -0.1253332335642985129, -0.9921147013144785420 ) ) ;
#29460 = EDGE_LOOP ( 'NONE', ( #20469, #9122, #19093, #2981, #4464, #3749, #16031, #15468 ) ) ;
#29461 = LINE ( 'NONE', #23592, #8810 ) ;
#29462 = AXIS2_PLACEMENT_3D ( 'NONE', #34214, #20696, #18743 ) ;
#29463 = DIRECTION ( 'NONE',  ( -1.000000000000000000, -3.040835319149746090E-31, -1.232595164407830946E-32 ) ) ;
#29464 = ORIENTED_EDGE ( 'NONE', *, *, #13875, .T. ) ;
#29465 = PLANE ( 'NONE',  #387 ) ;
#29466 = CARTESIAN_POINT ( 'NONE',  ( -410.0000000000000568, 105.0000000000000142, -101.9999999999999858 ) ) ;
#29467 = CYLINDRICAL_SURFACE ( 'NONE', #35088, 16.19999999999999929 ) ;
#29468 = ORIENTED_EDGE ( 'NONE', *, *, #30130, .T. ) ;
#29469 = PLANE ( 'NONE',  #1308 ) ;
#29470 = VERTEX_POINT ( 'NONE', #27965 ) ;
#29471 = VECTOR ( 'NONE', #15488, 1000.000000000000000 ) ;
#29472 = VECTOR ( 'NONE', #33256, 1000.000000000000000 ) ;
#29473 = CARTESIAN_POINT ( 'NONE',  ( -12.00000000000001066, 144.9999999999999147, 162.9999999999999716 ) ) ;
#29474 = ORIENTED_EDGE ( 'NONE', *, *, #11577, .F. ) ;
#29476 = DIRECTION ( 'NONE',  ( 0.000000000000000000, 0.000000000000000000, 1.000000000000000000 ) ) ;
#29475 = CARTESIAN_POINT ( 'NONE',  ( 0.000000000000000000, -3.728217946242704972, -30.24156218513559580 ) ) ;
#29477 = LINE ( 'NONE', #16313, #26757 ) ;
#29478 = AXIS2_PLACEMENT_3D ( 'NONE', #33438, #17453, #30769 ) ;
#29479 = ORIENTED_EDGE ( 'NONE', *, *, #8435, .T. ) ;
#29480 = CARTESIAN_POINT ( 'NONE',  ( 11.99999999999999645, 124.9999999999999716, 162.9999999999999716 ) ) ;
#29481 = CYLINDRICAL_SURFACE ( 'NONE', #2360, 2.500000000000002220 ) ;
#29482 = ORIENTED_EDGE ( 'NONE', *, *, #9151, .F. ) ;
#29483 = VECTOR ( 'NONE', #29901, 1000.000000000000000 ) ;
#29484 = AXIS2_PLACEMENT_3D ( 'NONE', #2337, #13216, #12514 ) ;
#29485 = DIRECTION ( 'NONE',  ( -7.893605728314051750E-14, 1.618803117314786530E-15, 1.000000000000000000 ) ) ;
#29486 = EDGE_CURVE ( 'NONE', #20346, #11447, #25289, .T. ) ;
#29487 = ORIENTED_EDGE ( 'NONE', *, *, #10768, .F. ) ;
#29488 = DIRECTION ( 'NONE',  ( 5.546364386991661285E-52, 0.000000000000000000, 1.000000000000000000 ) ) ;
#29489 = VERTEX_POINT ( 'NONE', #19443 ) ;
#29490 = CARTESIAN_POINT ( 'NONE',  ( 19.99999999999996092, -134.9999999999999716, -162.9999999999999432 ) ) ;
#29491 = ADVANCED_FACE ( 'NONE', ( #3571 ), #27611, .F. ) ;
#29492 = CARTESIAN_POINT ( 'NONE',  ( 0.5344654698446009711, -9.073918974790316838, -11.28351131189991285 ) ) ;
#29493 = AXIS2_PLACEMENT_3D ( 'NONE', #23442, #1726, #4213 ) ;
#29494 = ADVANCED_FACE ( 'NONE', ( #27786 ), #3049, .T. ) ;
#29495 = CARTESIAN_POINT ( 'NONE',  ( -108.7214454096172460, -3.512874579320472979, -6.627714125729964323 ) ) ;
#29496 = DIRECTION ( 'NONE',  ( -0.000000000000000000, -1.836970198721029688E-16, 1.000000000000000000 ) ) ;
#29497 = ORIENTED_EDGE ( 'NONE', *, *, #18980, .T. ) ;
#29498 = ORIENTED_EDGE ( 'NONE', *, *, #34474, .F. ) ;
#29499 = PRODUCT_DEFINITION_SHAPE ( 'NONE', 'NONE',  #35216 ) ;
#29500 = VERTEX_POINT ( 'NONE', #19797 ) ;
#29501 = CARTESIAN_POINT ( 'NONE',  ( 9.199999999999999289, 13.50000000000000178, 0.000000000000000000 ) ) ;
#29502 = EDGE_CURVE ( 'NONE', #32236, #15484, #17157, .T. ) ;
#29503 = CARTESIAN_POINT ( 'NONE',  ( -499.9999999999999432, 104.9999999999999858, 162.9999999999999716 ) ) ;
#29504 = CARTESIAN_POINT ( 'NONE',  ( -45.42888529050880209, 14.20380584968301640, 33.22126893951599413 ) ) ;
#29505 = CIRCLE ( 'NONE', #28909, 7.999999999999952038 ) ;
#29506 = DIRECTION ( 'NONE',  ( -1.000000000000000000, 0.000000000000000000, -1.292961597001347186E-16 ) ) ;
#29507 = DIRECTION ( 'NONE',  ( 1.232595164407830946E-32, 7.496237820289040735E-63, -1.000000000000000000 ) ) ;
#29508 = LINE ( 'NONE', #13318, #7189 ) ;
#29509 = CARTESIAN_POINT ( 'NONE',  ( -36.80830595996284416, 8.862931941313791029, -36.68877005347593467 ) ) ;
#29510 = ORIENTED_EDGE ( 'NONE', *, *, #33501, .F. ) ;
#29511 = CYLINDRICAL_SURFACE ( 'NONE', #17436, 2.525000000000001243 ) ;
#29512 = EDGE_CURVE ( 'NONE', #12400, #19207, #30644, .T. ) ;
#29513 = FACE_OUTER_BOUND ( 'NONE', #26594, .T. ) ;
#29514 = DIRECTION ( 'NONE',  ( -0.000000000000000000, -0.000000000000000000, 1.000000000000000000 ) ) ;
#29515 = VERTEX_POINT ( 'NONE', #25105 ) ;
#29516 = VECTOR ( 'NONE', #28830, 1000.000000000000000 ) ;
#29517 = CARTESIAN_POINT ( 'NONE',  ( 0.02407890056655781832, 31.00221527374952046, -2.344426712874310148 ) ) ;
#29518 = ORIENTED_EDGE ( 'NONE', *, *, #8722, .T. ) ;
#29519 = CARTESIAN_POINT ( 'NONE',  ( -30.91434716440808117, 10.17386417614055638, -36.68877005347593467 ) ) ;
#29520 = CARTESIAN_POINT ( 'NONE',  ( 11.99999999999999645, 124.9999999999999716, 162.9999999999999716 ) ) ;
#29521 = AXIS2_PLACEMENT_3D ( 'NONE', #8472, #2946, #9007 ) ;
#29522 = VERTEX_POINT ( 'NONE', #740 ) ;
#29523 = DIRECTION ( 'NONE',  ( -0.1617819965527647619, -0.9868265225415261410, -1.812770913216290044E-16 ) ) ;
#29524 = CARTESIAN_POINT ( 'NONE',  ( 2.789999999999999147, -15.32140196853772984, 27.05343472112986092 ) ) ;
#29525 = ORIENTED_EDGE ( 'NONE', *, *, #23432, .F. ) ;
#29526 = AXIS2_PLACEMENT_3D ( 'NONE', #10775, #32119, #26778 ) ;
#29527 = ORIENTED_EDGE ( 'NONE', *, *, #32103, .F. ) ;
#29528 = DIRECTION ( 'NONE',  ( -0.1063910735369017202, 0.9943243633099136947, -1.000770725407181676E-14 ) ) ;
#29529 = PLANE ( 'NONE',  #12733 ) ;
#29530 = ORIENTED_EDGE ( 'NONE', *, *, #33939, .T. ) ;
#29531 = DIRECTION ( 'NONE',  ( -1.000000000000000000, -0.000000000000000000, -0.000000000000000000 ) ) ;
#29532 = EDGE_CURVE ( 'NONE', #9246, #10430, #6232, .T. ) ;
#29533 = DIRECTION ( 'NONE',  ( 0.000000000000000000, 0.000000000000000000, 1.000000000000000000 ) ) ;
#29534 = VECTOR ( 'NONE', #17534, 1000.000000000000000 ) ;
#29535 = DIRECTION ( 'NONE',  ( -1.000000000000000000, 0.000000000000000000, -0.000000000000000000 ) ) ;
#29536 = CARTESIAN_POINT ( 'NONE',  ( 102.4159735622909722, -5.136475861867761061, 5.468785347707075140 ) ) ;
#29537 = ORIENTED_EDGE ( 'NONE', *, *, #27031, .F. ) ;
#29538 = ADVANCED_FACE ( 'NONE', ( #20485 ), #3920, .F. ) ;
#29539 = DIRECTION ( 'NONE',  ( 0.000000000000000000, 0.000000000000000000, 1.000000000000000000 ) ) ;
#29540 = EDGE_CURVE ( 'NONE', #10055, #18879, #30992, .T. ) ;
#29542 = CARTESIAN_POINT ( 'NONE',  ( -499.9999999999999432, 136.9999999999999432, 162.9999999999999716 ) ) ;
#29541 = DIRECTION ( 'NONE',  ( -3.469446951953832974E-18, -1.000000000000000000, -7.888609052210116302E-31 ) ) ;
#29543 = ORIENTED_EDGE ( 'NONE', *, *, #12271, .T. ) ;
#29544 = ORIENTED_EDGE ( 'NONE', *, *, #24168, .T. ) ;
#29545 = EDGE_CURVE ( 'NONE', #8598, #109, #31335, .T. ) ;
#29546 = ADVANCED_FACE ( 'NONE', ( #15330 ), #12484, .F. ) ;
#29547 = DIRECTION ( 'NONE',  ( 0.000000000000000000, 0.000000000000000000, 1.000000000000000000 ) ) ;
#29548 = EDGE_LOOP ( 'NONE', ( #59, #23722, #1998, #12871 ) ) ;
#29549 = DIRECTION ( 'NONE',  ( 1.000000000000000000, 0.000000000000000000, -0.000000000000000000 ) ) ;
#29550 = CARTESIAN_POINT ( 'NONE',  ( 1.040000000000000924, 0.000000000000000000, 0.000000000000000000 ) ) ;
#29551 = ORIENTED_EDGE ( 'NONE', *, *, #24735, .T. ) ;
#29552 = VECTOR ( 'NONE', #23210, 1000.000000000000000 ) ;
#29553 = LINE ( 'NONE', #15870, #18114 ) ;
#29554 = DIRECTION ( 'NONE',  ( -1.000000000000000000, 0.000000000000000000, -1.300283923313630633E-47 ) ) ;
#29555 = ORIENTED_EDGE ( 'NONE', *, *, #31273, .F. ) ;
#29556 = DIRECTION ( 'NONE',  ( -0.000000000000000000, 0.000000000000000000, 1.000000000000000000 ) ) ;
#29557 = LINE ( 'NONE', #22249, #9766 ) ;
#29558 = EDGE_CURVE ( 'NONE', #27628, #28173, #1775, .T. ) ;
#29559 = CARTESIAN_POINT ( 'NONE',  ( -349.0000000000000000, -125.0000000000000284, 130.0000000000000000 ) ) ;
#29560 = CARTESIAN_POINT ( 'NONE',  ( -442.0000000000000000, -125.0000000000000000, 100.0000000000000000 ) ) ;
#29561 = DIRECTION ( 'NONE',  ( -1.000000000000000000, -0.000000000000000000, -0.000000000000000000 ) ) ;
#29562 = FACE_OUTER_BOUND ( 'NONE', #26066, .T. ) ;
#29563 = CARTESIAN_POINT ( 'NONE',  ( -430.0000000000000000, 130.9999999999999716, 126.0000000000000000 ) ) ;
#29564 = ADVANCED_FACE ( 'NONE', ( #33837 ), #17714, .T. ) ;
#29565 = ORIENTED_EDGE ( 'NONE', *, *, #1510, .T. ) ;
#29566 = ADVANCED_FACE ( 'NONE', ( #12138 ), #34178, .T. ) ;
#29567 = DIRECTION ( 'NONE',  ( 0.000000000000000000, 1.000000000000000000, 0.000000000000000000 ) ) ;
#29568 = DIRECTION ( 'NONE',  ( -6.982962677686266711E-15, -6.982962677686339286E-15, 1.000000000000000000 ) ) ;
#29569 = PRODUCT_DEFINITION_CONTEXT ( 'detailed design', #21229, 'design' ) ;
#29570 = EDGE_LOOP ( 'NONE', ( #20125, #32097, #14487, #4123 ) ) ;
#29571 = EDGE_LOOP ( 'NONE', ( #25777, #4693, #33209, #27723 ) ) ;
#29572 = VECTOR ( 'NONE', #26544, 1000.000000000000000 ) ;
#29573 = LINE ( 'NONE', #29399, #34111 ) ;
#29574 = DIRECTION ( 'NONE',  ( 0.6953438540009243551, -0.7186772048027831872, 1.201189489407537883E-14 ) ) ;
#29575 = ORIENTED_EDGE ( 'NONE', *, *, #16204, .F. ) ;
#29576 = DIRECTION ( 'NONE',  ( 0.000000000000000000, 0.000000000000000000, 1.000000000000000000 ) ) ;
#29577 = ITEM_DEFINED_TRANSFORMATION ( 'NONE', 'NONE', #15003,  #28566 ) ;
#29578 = CARTESIAN_POINT ( 'NONE',  ( 0.000000000000000000, 33.69708579775584667, -36.68877005347592757 ) ) ;
#29579 = VERTEX_POINT ( 'NONE', #4269 ) ;
#29580 = ORIENTED_EDGE ( 'NONE', *, *, #12797, .T. ) ;
#29581 = EDGE_CURVE ( 'NONE', #8689, #26511, #22984, .T. ) ;
#29582 = EDGE_CURVE ( 'NONE', #14714, #30633, #21113, .T. ) ;
#29583 = DIRECTION ( 'NONE',  ( 1.000000000000000000, 3.040835319149746528E-31, 1.232595164407830946E-32 ) ) ;
#29584 = CARTESIAN_POINT ( 'NONE',  ( 0.000000000000000000, 2.005524111408194088, 31.87689292423238996 ) ) ;
#29585 = CARTESIAN_POINT ( 'NONE',  ( 1.394999999999999574, -10.37741591188871659, -32.81304455236878681 ) ) ;
#29586 = DIRECTION ( 'NONE',  ( -0.000000000000000000, 1.836970198721029934E-16, -1.000000000000000000 ) ) ;
#29587 = LINE ( 'NONE', #5182, #30197 ) ;
#29588 = VERTEX_POINT ( 'NONE', #9799 ) ;
#29589 = CARTESIAN_POINT ( 'NONE',  ( -500.0000000000000000, -105.0000000000000142, 187.0000000000000000 ) ) ;
#29590 = FACE_OUTER_BOUND ( 'NONE', #10358, .T. ) ;
#29591 = DIRECTION ( 'NONE',  ( 0.000000000000000000, -1.000000000000000000, 0.000000000000000000 ) ) ;
#29592 = AXIS2_PLACEMENT_3D ( 'NONE', #20961, #4394, #23806 ) ;
#29593 = DIRECTION ( 'NONE',  ( -1.000000000000000000, -0.000000000000000000, -0.000000000000000000 ) ) ;
#29594 = ADVANCED_FACE ( 'NONE', ( #9277, #1612 ), #31170, .T. ) ;
#29595 = DIRECTION ( 'NONE',  ( -1.000000000000000000, -0.000000000000000000, -0.000000000000000000 ) ) ;
#29597 = CARTESIAN_POINT ( 'NONE',  ( 32.05156013847309993, -20.15193397489277771, 49.43553178847298568 ) ) ;
#29596 = CARTESIAN_POINT ( 'NONE',  ( 0.000000000000000000, 0.000000000000000000, 0.000000000000000000 ) ) ;
#29598 = CARTESIAN_POINT ( 'NONE',  ( -35.00000000000000000, 16.36473396058513075, -36.68877005347592757 ) ) ;
#29599 = ORIENTED_EDGE ( 'NONE', *, *, #17946, .T. ) ;
#29600 = FACE_OUTER_BOUND ( 'NONE', #11372, .T. ) ;
#29602 = DIRECTION ( 'NONE',  ( -1.232595164407830946E-32, 0.000000000000000000, -1.000000000000000000 ) ) ;
#29601 = CARTESIAN_POINT ( 'NONE',  ( -361.0000000000000000, 134.9999999999999716, 112.0000000000000000 ) ) ;
#29603 = EDGE_CURVE ( 'NONE', #13768, #29101, #27928, .T. ) ;
#29604 = EDGE_CURVE ( 'NONE', #6574, #17675, #25819, .T. ) ;
#29605 = EDGE_CURVE ( 'NONE', #13484, #2324, #23164, .T. ) ;
#29606 = ORIENTED_EDGE ( 'NONE', *, *, #32256, .T. ) ;
#29607 = CIRCLE ( 'NONE', #22801, 7.500000000000000000 ) ;
#29608 = CARTESIAN_POINT ( 'NONE',  ( -12.00000000000001066, -112.9999999999999858, 155.0000000000000000 ) ) ;
#29609 = VECTOR ( 'NONE', #9029, 1000.000000000000000 ) ;
#29610 = ADVANCED_FACE ( 'NONE', ( #14639, #31510 ), #15155, .F. ) ;
#29611 = ORIENTED_EDGE ( 'NONE', *, *, #5899, .T. ) ;
#29612 = ORIENTED_EDGE ( 'NONE', *, *, #33754, .T. ) ;
#29613 = PLANE ( 'NONE',  #24104 ) ;
#29614 = ORIENTED_EDGE ( 'NONE', *, *, #18930, .F. ) ;
#29615 = VERTEX_POINT ( 'NONE', #19966 ) ;
#29616 = AXIS2_PLACEMENT_3D ( 'NONE', #34267, #12564, #20915 ) ;
#29617 = CARTESIAN_POINT ( 'NONE',  ( -361.0000000000000000, -125.0000000000000284, 168.9999999999999716 ) ) ;
#29618 = AXIS2_PLACEMENT_3D ( 'NONE', #32628, #10932, #29620 ) ;
#29619 = CARTESIAN_POINT ( 'NONE',  ( -12.00000000000001066, -28.99999999999999645, -175.0000000000000000 ) ) ;
#29620 = DIRECTION ( 'NONE',  ( 0.000000000000000000, 0.000000000000000000, 1.000000000000000000 ) ) ;
#29621 = VERTEX_POINT ( 'NONE', #30816 ) ;
#29622 = ORIENTED_EDGE ( 'NONE', *, *, #5118, .T. ) ;
#29623 = DIRECTION ( 'NONE',  ( 0.000000000000000000, 1.000000000000000000, 5.145227585319922065E-49 ) ) ;
#29624 = DIRECTION ( 'NONE',  ( -0.000000000000000000, 1.836970198721029934E-16, -1.000000000000000000 ) ) ;
#29625 = DIRECTION ( 'NONE',  ( 0.000000000000000000, 0.000000000000000000, 1.000000000000000000 ) ) ;
#29626 = DIRECTION ( 'NONE',  ( -0.000000000000000000, -0.000000000000000000, -1.000000000000000000 ) ) ;
#29627 = ORIENTED_EDGE ( 'NONE', *, *, #12540, .F. ) ;
#29628 = DIRECTION ( 'NONE',  ( -0.000000000000000000, -0.000000000000000000, -1.000000000000000000 ) ) ;
#29629 = CARTESIAN_POINT ( 'NONE',  ( 8.000000000000000000, 0.000000000000000000, 0.000000000000000000 ) ) ;
#29630 = EDGE_LOOP ( 'NONE', ( #15264, #12032 ) ) ;
#29631 = AXIS2_PLACEMENT_3D ( 'NONE', #34072, #10534, #24031 ) ;
#29632 = AXIS2_PLACEMENT_3D ( 'NONE', #5673, #10518, #30083 ) ;
#29633 = LINE ( 'NONE', #24447, #18520 ) ;
#29634 = DIRECTION ( 'NONE',  ( 0.000000000000000000, 0.000000000000000000, 1.000000000000000000 ) ) ;
#29635 = DIRECTION ( 'NONE',  ( -1.000000000000000000, 0.000000000000000000, 0.000000000000000000 ) ) ;
#29636 = EDGE_LOOP ( 'NONE', ( #34975, #5340, #18267, #24055 ) ) ;
#29637 = FACE_OUTER_BOUND ( 'NONE', #8208, .T. ) ;
#29638 = EDGE_LOOP ( 'NONE', ( #14641, #13210, #10996, #11493 ) ) ;
#29639 = DIRECTION ( 'NONE',  ( -0.000000000000000000, 1.836970198721029934E-16, -1.000000000000000000 ) ) ;
#29640 = ORIENTED_EDGE ( 'NONE', *, *, #18289, .T. ) ;
#29641 = LINE ( 'NONE', #15787, #14869 ) ;
#29642 = CARTESIAN_POINT ( 'NONE',  ( 0.000000000000000000, 2.281310696040539424E-14, -36.68877005347594178 ) ) ;
#29643 = AXIS2_PLACEMENT_3D ( 'NONE', #22679, #11830, #30504 ) ;
#29644 = EDGE_CURVE ( 'NONE', #15534, #5282, #8339, .T. ) ;
#29645 = EDGE_CURVE ( 'NONE', #22922, #32630, #5143, .T. ) ;
#29646 = VERTEX_POINT ( 'NONE', #7462 ) ;
#29647 = APPLICATION_CONTEXT ( 'automotive_design' ) ;
#29648 =( NAMED_UNIT ( * ) PLANE_ANGLE_UNIT ( ) SI_UNIT ( $, .RADIAN. ) );
#29649 = B_SPLINE_CURVE_WITH_KNOTS ( 'NONE', 3,
 ( #14724, #12048, #20745, #18096, #17922, #17741 ),
 .UNSPECIFIED., .F., .F.,
 ( 4, 2, 4 ),
 ( 4.404817002931014679E-07, 0.001874269606490522972, 0.003748098731280752587 ),
 .UNSPECIFIED. ) ;
#29650 = CARTESIAN_POINT ( 'NONE',  ( -418.0000000000000000, -125.0000000000000000, 194.9999999999999716 ) ) ;
#29651 = VERTEX_POINT ( 'NONE', #4605 ) ;
#29652 = AXIS2_PLACEMENT_3D ( 'NONE', #28682, #20163, #17678 ) ;
#29653 = AXIS2_PLACEMENT_3D ( 'NONE', #8170, #11382, #22238 ) ;
#29654 = VECTOR ( 'NONE', #327, 1000.000000000000000 ) ;
#29656 = ORIENTED_EDGE ( 'NONE', *, *, #1959, .F. ) ;
#29655 = AXIS2_PLACEMENT_3D ( 'NONE', #4400, #26296, #21317 ) ;
#29657 = DIRECTION ( 'NONE',  ( 0.000000000000000000, 1.000000000000000000, 2.309213040847544338E-50 ) ) ;
#29658 = CARTESIAN_POINT ( 'NONE',  ( -499.9999999999999432, 108.9999999999999858, 187.0000000000000000 ) ) ;
#29659 = ORIENTED_EDGE ( 'NONE', *, *, #32145, .T. ) ;
#29660 = CIRCLE ( 'NONE', #33083, 32.54542015209057126 ) ;
#29661 = CARTESIAN_POINT ( 'NONE',  ( 2.789999999999999591, -14.96303950468899480, -26.76267923430003393 ) ) ;
#29662 = FACE_OUTER_BOUND ( 'NONE', #18963, .T. ) ;
#29663 = CARTESIAN_POINT ( 'NONE',  ( -108.8307179568225109, -3.393468573754154782, -6.689828017866635612 ) ) ;
#29664 = FACE_OUTER_BOUND ( 'NONE', #14237, .T. ) ;
#29665 = VERTEX_POINT ( 'NONE', #23496 ) ;
#29666 = ORIENTED_EDGE ( 'NONE', *, *, #27232, .F. ) ;
#29667 = EDGE_LOOP ( 'NONE', ( #30337, #28405, #21421, #20082 ) ) ;
#29668 = DIRECTION ( 'NONE',  ( -1.000000000000000000, -0.000000000000000000, -0.000000000000000000 ) ) ;
#29669 = DIRECTION ( 'NONE',  ( -0.000000000000000000, -1.000000000000000000, -0.000000000000000000 ) ) ;
#29671 = AXIS2_PLACEMENT_3D ( 'NONE', #15634, #18308, #12962 ) ;
#29670 = DIRECTION ( 'NONE',  ( 0.000000000000000000, 0.000000000000000000, -1.000000000000000000 ) ) ;
#29672 = DIRECTION ( 'NONE',  ( 0.000000000000000000, 0.000000000000000000, 1.000000000000000000 ) ) ;
#29673 = DIRECTION ( 'NONE',  ( -0.02866416272524431944, -0.5286793732840951998, 0.8483374835754913246 ) ) ;
#29674 = LINE ( 'NONE', #16165, #34516 ) ;
#29675 = DIRECTION ( 'NONE',  ( 0.000000000000000000, 0.000000000000000000, -1.000000000000000000 ) ) ;
#29676 = VERTEX_POINT ( 'NONE', #2138 ) ;
#29677 = CARTESIAN_POINT ( 'NONE',  ( 2.789999999999999147, -8.112136323389137260, 30.01377904834206589 ) ) ;
#29678 = DIRECTION ( 'NONE',  ( -3.469446951953832974E-18, -1.000000000000000000, -7.888609052210116302E-31 ) ) ;
#29679 = VECTOR ( 'NONE', #27588, 1000.000000000000000 ) ;
#29680 = CARTESIAN_POINT ( 'NONE',  ( -20.00000000000007461, -113.0000000000000000, -159.0000000000000000 ) ) ;
#29681 = ORIENTED_EDGE ( 'NONE', *, *, #17797, .T. ) ;
#29682 = VECTOR ( 'NONE', #15779, 1000.000000000000114 ) ;
#29683 = VECTOR ( 'NONE', #8284, 1000.000000000000227 ) ;
#29684 = CARTESIAN_POINT ( 'NONE',  ( 105.0000000000000000, 0.000000000000000000, 60.00000000000000000 ) ) ;
#29685 = ORIENTED_EDGE ( 'NONE', *, *, #26740, .T. ) ;
#29686 = DIRECTION ( 'NONE',  ( -0.000000000000000000, 1.000000000000000000, -0.000000000000000000 ) ) ;
#29687 = EDGE_CURVE ( 'NONE', #509, #19620, #10326, .T. ) ;
#29688 = PLANE ( 'NONE',  #30927 ) ;
#29689 = EDGE_CURVE ( 'NONE', #32490, #1130, #34356, .T. ) ;
#29690 = ORIENTED_EDGE ( 'NONE', *, *, #3155, .F. ) ;
#29691 = DIRECTION ( 'NONE',  ( -1.000000000000000000, 0.000000000000000000, -0.000000000000000000 ) ) ;
#29692 = DIRECTION ( 'NONE',  ( 0.000000000000000000, 1.000000000000000000, 5.145227585319922065E-49 ) ) ;
#29694 = DIRECTION ( 'NONE',  ( 1.000000000000000000, 0.000000000000000000, 0.000000000000000000 ) ) ;
#29693 = PRODUCT_RELATED_PRODUCT_CATEGORY ( 'part', '', ( #695 ) ) ;
#29695 = VERTEX_POINT ( 'NONE', #15689 ) ;
#29696 = ORIENTED_EDGE ( 'NONE', *, *, #29824, .F. ) ;
#29697 = DIRECTION ( 'NONE',  ( 0.5270880874649396253, -0.8498106542357255488, 7.655505697817509428E-15 ) ) ;
#29698 = DIRECTION ( 'NONE',  ( -1.000000000000000000, 0.000000000000000000, -0.000000000000000000 ) ) ;
#29699 = ORIENTED_EDGE ( 'NONE', *, *, #18346, .F. ) ;
#29700 = DIRECTION ( 'NONE',  ( 0.000000000000000000, -1.000000000000000000, -1.836970198721029934E-16 ) ) ;
#29701 = AXIS2_PLACEMENT_3D ( 'NONE', #33053, #30045, #5638 ) ;
#29702 = FILL_AREA_STYLE ('',( #7977 ) ) ;
#29703 = VECTOR ( 'NONE', #24724, 1000.000000000000000 ) ;
#29704 = CARTESIAN_POINT ( 'NONE',  ( 0.000000000000000000, -25.77598557799239742, -16.24962337825829195 ) ) ;
#29705 = CARTESIAN_POINT ( 'NONE',  ( 1.394999999999999574, 34.17636915695680244, -4.045051921974837761 ) ) ;
#29707 = VECTOR ( 'NONE', #18411, 1000.000000000000000 ) ;
#29706 = CONTEXT_DEPENDENT_SHAPE_REPRESENTATION ( #23313, #3470 ) ;
#29708 = VERTEX_POINT ( 'NONE', #34533 ) ;
#29709 = VECTOR ( 'NONE', #24109, 1000.000000000000000 ) ;
#29710 = ORIENTED_EDGE ( 'NONE', *, *, #27569, .F. ) ;
#29711 = CARTESIAN_POINT ( 'NONE',  ( 19.99999999999998934, 144.9999999999999716, -186.9999999999999716 ) ) ;
#29713 = DIRECTION ( 'NONE',  ( -0.2675283385292215321, -0.9635499925192227977, -0.000000000000000000 ) ) ;
#29712 = FACE_OUTER_BOUND ( 'NONE', #21727, .T. ) ;
#29714 = ORIENTED_EDGE ( 'NONE', *, *, #15853, .F. ) ;
#29715 = EDGE_LOOP ( 'NONE', ( #31654, #33593, #26578, #9969, #19580, #13737, #4925, #7490, #21521, #13865 ) ) ;
#29716 = CARTESIAN_POINT ( 'NONE',  ( -418.0000000000000000, -125.0000000000000000, 190.9999999999999716 ) ) ;
#29717 = ORIENTED_EDGE ( 'NONE', *, *, #21132, .T. ) ;
#29718 = CARTESIAN_POINT ( 'NONE',  ( -361.0000000000000000, -135.0000000000000000, 128.0000000000000000 ) ) ;
#29719 = CARTESIAN_POINT ( 'NONE',  ( 32.81769769215652133, 18.87860345536237006, 68.31122994652405112 ) ) ;
#29720 = VERTEX_POINT ( 'NONE', #32211 ) ;
#29721 = VERTEX_POINT ( 'NONE', #13012 ) ;
#29722 = CARTESIAN_POINT ( 'NONE',  ( 1.749999999999999778, -24.90160365674886478, 23.75493189058330756 ) ) ;
#29723 = LINE ( 'NONE', #16220, #8633 ) ;
#29724 = ORIENTED_EDGE ( 'NONE', *, *, #14068, .F. ) ;
#29725 = DIRECTION ( 'NONE',  ( 0.000000000000000000, 1.000000000000000000, 0.000000000000000000 ) ) ;
#29726 = DIRECTION ( 'NONE',  ( 1.000000000000000000, 0.000000000000000000, 0.000000000000000000 ) ) ;
#29727 = EDGE_CURVE ( 'NONE', #17530, #22891, #28488, .T. ) ;
#29728 = LINE ( 'NONE', #16224, #17837 ) ;
#29730 = DIRECTION ( 'NONE',  ( 1.000000000000000000, 0.000000000000000000, 0.000000000000000000 ) ) ;
#29729 = AXIS2_PLACEMENT_3D ( 'NONE', #30446, #25445, #3204 ) ;
#29731 = AXIS2_PLACEMENT_3D ( 'NONE', #32514, #27352, #8137 ) ;
#29732 = AXIS2_PLACEMENT_3D ( 'NONE', #3549, #8371, #16934 ) ;
#29733 = AXIS2_PLACEMENT_3D ( 'NONE', #17711, #20026, #28022 ) ;
#29734 = CYLINDRICAL_SURFACE ( 'NONE', #27362, 34.41491905851385269 ) ;
#29735 = CYLINDRICAL_SURFACE ( 'NONE', #20744, 4.750000000000004441 ) ;
#29737 = EDGE_CURVE ( 'NONE', #18467, #30469, #13184, .T. ) ;
#29736 = CARTESIAN_POINT ( 'NONE',  ( -5.210000000000000853, 0.000000000000000000, 0.000000000000000000 ) ) ;
#29738 = ORIENTED_EDGE ( 'NONE', *, *, #28567, .T. ) ;
#29739 = EDGE_CURVE ( 'NONE', #11787, #13964, #9177, .T. ) ;
#29740 = DIRECTION ( 'NONE',  ( 0.000000000000000000, 0.000000000000000000, -1.000000000000000000 ) ) ;
#29741 = DIRECTION ( 'NONE',  ( 0.9241025011561869729, 0.3821446942676031133, -3.823589569486765865E-15 ) ) ;
#29742 = ORIENTED_EDGE ( 'NONE', *, *, #20389, .F. ) ;
#29743 = ORIENTED_EDGE ( 'NONE', *, *, #18799, .T. ) ;
#29744 = EDGE_CURVE ( 'NONE', #11473, #6935, #80, .T. ) ;
#29745 = VECTOR ( 'NONE', #23888, 1000.000000000000000 ) ;
#29746 = LINE ( 'NONE', #14087, #22179 ) ;
#29747 = CARTESIAN_POINT ( 'NONE',  ( 822.4753423408578783, 1297.757510667704310, 1753.598338701303419 ) ) ;
#29748 = VERTEX_POINT ( 'NONE', #35073 ) ;
#29749 = CARTESIAN_POINT ( 'NONE',  ( -449.9999999999999432, 105.0000000000000142, 132.0000000000000000 ) ) ;
#29750 = B_SPLINE_CURVE_WITH_KNOTS ( 'NONE', 3,
 ( #32510, #19716, #8135, #5281 ),
 .UNSPECIFIED., .F., .F.,
 ( 4, 4 ),
 ( 2.080333525987768553E-07, 0.0006879438135628904464 ),
 .UNSPECIFIED. ) ;
#29751 = AXIS2_PLACEMENT_3D ( 'NONE', #28817, #6754, #12295 ) ;
#29752 = CARTESIAN_POINT ( 'NONE',  ( -49.20661276131353645, 21.27332514515927286, 0.4570320086110524205 ) ) ;
#29753 = AXIS2_PLACEMENT_3D ( 'NONE', #11138, #26970, #13981 ) ;
#29754 = ORIENTED_EDGE ( 'NONE', *, *, #20498, .T. ) ;
#29755 = ORIENTED_EDGE ( 'NONE', *, *, #28014, .F. ) ;
#29756 = FACE_OUTER_BOUND ( 'NONE', #3879, .T. ) ;
#29757 = DIRECTION ( 'NONE',  ( -1.000000000000000000, 6.792721752314501023E-48, -3.697785493223492838E-32 ) ) ;
#29758 = FACE_OUTER_BOUND ( 'NONE', #23144, .T. ) ;
#29759 = DIRECTION ( 'NONE',  ( 1.000000000000000000, 0.000000000000000000, 0.000000000000000000 ) ) ;
#29760 = DIRECTION ( 'NONE',  ( -0.000000000000000000, 1.000000000000000000, -0.000000000000000000 ) ) ;
#29761 = ORIENTED_EDGE ( 'NONE', *, *, #12173, .T. ) ;
#29762 = PLANE ( 'NONE',  #12939 ) ;
#29763 = LINE ( 'NONE', #402, #14578 ) ;
#29764 = FACE_BOUND ( 'NONE', #17527, .T. ) ;
#29765 = CARTESIAN_POINT ( 'NONE',  ( -410.0000000000000568, -104.9999999999999716, -187.0000000000000000 ) ) ;
#29766 = DIRECTION ( 'NONE',  ( -1.000000000000000000, 0.000000000000000000, 0.000000000000000000 ) ) ;
#29767 = DIRECTION ( 'NONE',  ( -1.000000000000000000, -0.000000000000000000, -0.000000000000000000 ) ) ;
#29769 = LINE ( 'NONE', #409, #31037 ) ;
#29768 = FACE_OUTER_BOUND ( 'NONE', #11562, .T. ) ;
#29770 = AXIS2_PLACEMENT_3D ( 'NONE', #8564, #3572, #25106 ) ;
#29771 = CARTESIAN_POINT ( 'NONE',  ( 11.99999999999999645, 124.9999999999999716, 159.0000000000000000 ) ) ;
#29772 = ORIENTED_EDGE ( 'NONE', *, *, #30694, .F. ) ;
#29773 = CARTESIAN_POINT ( 'NONE',  ( -10.00000000000000000, 0.000000000000000000, 0.000000000000000000 ) ) ;
#29775 = DIRECTION ( 'NONE',  ( -0.000000000000000000, 0.000000000000000000, 1.000000000000000000 ) ) ;
#29774 = LINE ( 'NONE', #5384, #15514 ) ;
#29776 = EDGE_CURVE ( 'NONE', #591, #16412, #18355, .T. ) ;
#29777 = AXIS2_PLACEMENT_3D ( 'NONE', #14751, #14575, #31277 ) ;
#29779 = VERTEX_POINT ( 'NONE', #24013 ) ;
#29778 = AXIS2_PLACEMENT_3D ( 'NONE', #2713, #24247, #32955 ) ;
#29780 = EDGE_CURVE ( 'NONE', #8977, #34561, #32026, .T. ) ;
#29781 = EDGE_CURVE ( 'NONE', #3900, #10873, #20833, .T. ) ;
#29782 = AXIS2_PLACEMENT_3D ( 'NONE', #5467, #34866, #10476 ) ;
#29783 = FACE_OUTER_BOUND ( 'NONE', #33903, .T. ) ;
#29784 = PRODUCT_DEFINITION_SHAPE ( 'NONE', 'NONE',  #35205 ) ;
#29785 = EDGE_LOOP ( 'NONE', ( #15686, #19269, #34919, #13453, #17342 ) ) ;
#29786 = ORIENTED_EDGE ( 'NONE', *, *, #32576, .F. ) ;
#29787 = CARTESIAN_POINT ( 'NONE',  ( 23.31255882915078814, -22.70966696615089830, 68.31122994652405112 ) ) ;
#29788 = ORIENTED_EDGE ( 'NONE', *, *, #31875, .T. ) ;
#29789 = VERTEX_POINT ( 'NONE', #29010 ) ;
#29790 = CARTESIAN_POINT ( 'NONE',  ( -500.0000000000000000, -105.0000000000000142, 162.9999999999999716 ) ) ;
#29791 = EDGE_CURVE ( 'NONE', #24353, #22184, #25359, .T. ) ;
#29792 = CIRCLE ( 'NONE', #13871, 2.000000000000001776 ) ;
#29793 = CARTESIAN_POINT ( 'NONE',  ( 2.789999999999999147, 26.03801215795517621, 16.98986790278620873 ) ) ;
#29794 = FACE_OUTER_BOUND ( 'NONE', #25718, .T. ) ;
#29795 = ORIENTED_EDGE ( 'NONE', *, *, #27108, .T. ) ;
#29796 = ORIENTED_EDGE ( 'NONE', *, *, #11369, .T. ) ;
#29797 = FACE_OUTER_BOUND ( 'NONE', #33461, .T. ) ;
#29798 =( NAMED_UNIT ( * ) SI_UNIT ( $, .STERADIAN. ) SOLID_ANGLE_UNIT ( ) );
#29799 = AXIS2_PLACEMENT_3D ( 'NONE', #23158, #3913, #28661 ) ;
#29800 = EDGE_CURVE ( 'NONE', #25155, #33086, #4968, .T. ) ;
#29801 = CARTESIAN_POINT ( 'NONE',  ( 101.2096900042061804, -4.324196401257808908, -11.73154709691606179 ) ) ;
#29802 = CARTESIAN_POINT ( 'NONE',  ( 22.89764159710613001, 8.346743312457581609, -87.50000000000000000 ) ) ;
#29803 = VERTEX_POINT ( 'NONE', #7997 ) ;
#29804 = SURFACE_SIDE_STYLE ('',( #26048 ) ) ;
#29805 = EDGE_CURVE ( 'NONE', #28395, #17606, #1961, .T. ) ;
#29806 = CARTESIAN_POINT ( 'NONE',  ( -23.48826533576967179, -5.175545323022858746, -16.02576232019386993 ) ) ;
#29807 = VECTOR ( 'NONE', #18928, 999.9999999999998863 ) ;
#29808 = DIRECTION ( 'NONE',  ( 0.000000000000000000, 1.000000000000000000, 0.000000000000000000 ) ) ;
#29809 = VERTEX_POINT ( 'NONE', #21367 ) ;
#29810 = AXIS2_PLACEMENT_3D ( 'NONE', #8157, #26853, #18693 ) ;
#29811 = FACE_OUTER_BOUND ( 'NONE', #958, .T. ) ;
#29812 = EDGE_CURVE ( 'NONE', #5593, #1001, #30207, .T. ) ;
#29813 = LINE ( 'NONE', #18965, #18894 ) ;
#29814 = DIRECTION ( 'NONE',  ( 1.000000000000000000, 0.000000000000000000, 0.000000000000000000 ) ) ;
#29815 = LINE ( 'NONE', #16307, #30879 ) ;
#29816 = VERTEX_POINT ( 'NONE', #29719 ) ;
#29817 = DIRECTION ( 'NONE',  ( 1.000000000000000000, 0.000000000000000000, 0.000000000000000000 ) ) ;
#29818 = ORIENTED_EDGE ( 'NONE', *, *, #21690, .T. ) ;
#29820 = CARTESIAN_POINT ( 'NONE',  ( -12.00000000000003908, -145.0000000000000000, -162.9999999999999432 ) ) ;
#29819 = DIRECTION ( 'NONE',  ( 0.000000000000000000, 0.000000000000000000, -1.000000000000000000 ) ) ;
#29821 = DIRECTION ( 'NONE',  ( 0.000000000000000000, 0.000000000000000000, 1.000000000000000000 ) ) ;
#29822 = AXIS2_PLACEMENT_3D ( 'NONE', #31583, #7186, #28914 ) ;
#29823 = ORIENTED_EDGE ( 'NONE', *, *, #34970, .F. ) ;
#29824 = EDGE_CURVE ( 'NONE', #16094, #9347, #21671, .T. ) ;
#29825 = EDGE_CURVE ( 'NONE', #13030, #2206, #16035, .T. ) ;
#29826 = CARTESIAN_POINT ( 'NONE',  ( 11.99999999999999645, -55.00000000000000711, -162.9999999999999432 ) ) ;
#29827 = DIRECTION ( 'NONE',  ( 0.000000000000000000, 1.131431318426415506E-52, 1.000000000000000000 ) ) ;
#29828 = AXIS2_PLACEMENT_3D ( 'NONE', #33792, #20274, #23968 ) ;
#29829 = ORIENTED_EDGE ( 'NONE', *, *, #10528, .T. ) ;
#29830 = EDGE_CURVE ( 'NONE', #1305, #7253, #853, .T. ) ;
#29831 = PRESENTATION_LAYER_ASSIGNMENT (  '', '', ( #9941 ) ) ;
#29832 = CIRCLE ( 'NONE', #7079, 34.41491905851385269 ) ;
#29833 = EDGE_LOOP ( 'NONE', ( #31025, #16599, #7564, #16739, #3567, #4083 ) ) ;
#29834 = DIRECTION ( 'NONE',  ( -0.000000000000000000, 1.836970198721029934E-16, -1.000000000000000000 ) ) ;
#29835 = CARTESIAN_POINT ( 'NONE',  ( -100.5859555588355079, 2.605551551359105211, 7.039079951515508249 ) ) ;
#29836 = ORIENTED_EDGE ( 'NONE', *, *, #32339, .F. ) ;
#29837 = ORIENTED_EDGE ( 'NONE', *, *, #2390, .F. ) ;
#29838 = DIRECTION ( 'NONE',  ( 0.000000000000000000, -1.131431318426415506E-52, -1.000000000000000000 ) ) ;
#29839 = CARTESIAN_POINT ( 'NONE',  ( 1.205771365940050854, -7.794228634059966687, -13.49999999999999822 ) ) ;
#29840 = FACE_OUTER_BOUND ( 'NONE', #10286, .T. ) ;
#29841 = LINE ( 'NONE', #13644, #13116 ) ;
#29842 = EDGE_LOOP ( 'NONE', ( #34342, #11556 ) ) ;
#29843 = ORIENTED_EDGE ( 'NONE', *, *, #18852, .F. ) ;
#29844 = LINE ( 'NONE', #21824, #5973 ) ;
#29845 = CARTESIAN_POINT ( 'NONE',  ( 18.63894936814906345, 26.67946662374789213, 68.31122994652405112 ) ) ;
#29846 = B_SPLINE_CURVE_WITH_KNOTS ( 'NONE', 3,
 ( #32725, #8349, #27738, #21217, #33074, #22405 ),
 .UNSPECIFIED., .F., .F.,
 ( 4, 2, 4 ),
 ( 4.404817209422835260E-07, 0.001874269760234689892, 0.003748099038748437580 ),
 .UNSPECIFIED. ) ;
#29847 = FACE_OUTER_BOUND ( 'NONE', #32531, .T. ) ;
#29848 = DIRECTION ( 'NONE',  ( 0.000000000000000000, 0.000000000000000000, -1.000000000000000000 ) ) ;
#29849 = EDGE_CURVE ( 'NONE', #11336, #26209, #13152, .T. ) ;
#29850 = EDGE_CURVE ( 'NONE', #35062, #17587, #13530, .T. ) ;
#29851 = VECTOR ( 'NONE', #1086, 1000.000000000000000 ) ;
#29852 = CARTESIAN_POINT ( 'NONE',  ( 0.000000000000000000, 0.000000000000000000, 4.679999999999999716 ) ) ;
#29853 = LINE ( 'NONE', #21657, #6258 ) ;
#29854 = CARTESIAN_POINT ( 'NONE',  ( -143.0000000000000568, -85.49999999999998579, 51.88904920397798293 ) ) ;
#29855 = DIRECTION ( 'NONE',  ( 0.000000000000000000, 1.836970198721029441E-16, -1.000000000000000000 ) ) ;
#29856 = ORIENTED_EDGE ( 'NONE', *, *, #11064, .F. ) ;
#29857 = VECTOR ( 'NONE', #3100, 1000.000000000000000 ) ;
#29858 = VECTOR ( 'NONE', #5618, 1000.000000000000000 ) ;
#29859 = DIRECTION ( 'NONE',  ( 1.000000000000000000, 0.000000000000000000, 0.000000000000000000 ) ) ;
#29860 = FACE_OUTER_BOUND ( 'NONE', #19752, .T. ) ;
#29861 = APPLICATION_CONTEXT ( 'automotive_design' ) ;
#29862 = CARTESIAN_POINT ( 'NONE',  ( 0.000000000000000000, 0.000000000000000000, 0.000000000000000000 ) ) ;
#29863 = ORIENTED_EDGE ( 'NONE', *, *, #33727, .F. ) ;
#29864 = VECTOR ( 'NONE', #26102, 1000.000000000000000 ) ;
#29865 = EDGE_CURVE ( 'NONE', #32903, #11385, #33015, .T. ) ;
#29866 = CARTESIAN_POINT ( 'NONE',  ( -499.9999999999999432, 136.9999999999999432, 187.0000000000000000 ) ) ;
#29867 = VERTEX_POINT ( 'NONE', #19758 ) ;
#29869 = CLOSED_SHELL ( 'NONE', ( #2158, #24645, #11330, #11980, #34063, #24642, #22665, #23419, #12058, #28472, #19254, #24559, #7443, #12034, #6904, #27273, #28275, #28522, #24100, #23467, #21803 ) ) ;
#29868 = CARTESIAN_POINT ( 'NONE',  ( 15.99999999999998579, 124.9999999999999716, 187.0000000000000000 ) ) ;
#29870 = DIRECTION ( 'NONE',  ( 0.000000000000000000, 0.000000000000000000, 1.000000000000000000 ) ) ;
#29871 = VERTEX_POINT ( 'NONE', #11030 ) ;
#29872 = CARTESIAN_POINT ( 'NONE',  ( -12.00000000000001066, 134.9999999999999432, -186.9999999999999716 ) ) ;
#29873 = CARTESIAN_POINT ( 'NONE',  ( 0.02407890056655825201, 14.63235270440936731, 27.43224275967444470 ) ) ;
#29874 = CARTESIAN_POINT ( 'NONE',  ( 2.783128942445853404, -26.23443237966589692, 16.26905388445657508 ) ) ;
#29875 = ORIENTED_EDGE ( 'NONE', *, *, #3094, .F. ) ;
#29876 = CIRCLE ( 'NONE', #11137, 7.999999999999979572 ) ;
#29877 = ORIENTED_EDGE ( 'NONE', *, *, #29805, .T. ) ;
#29878 = CARTESIAN_POINT ( 'NONE',  ( 772.5981804437851679, 1191.104452756041610, 1753.598338701303419 ) ) ;
#29879 = DIRECTION ( 'NONE',  ( 1.000000000000000000, 0.000000000000000000, 0.000000000000000000 ) ) ;
#29880 = ADVANCED_FACE ( 'NONE', ( #27397 ), #22415, .T. ) ;
#29881 = EDGE_LOOP ( 'NONE', ( #32999, #30592, #1468, #33812 ) ) ;
#29882 = VECTOR ( 'NONE', #28012, 1000.000000000000000 ) ;
#29883 = CARTESIAN_POINT ( 'NONE',  ( -430.0000000000000000, -119.0000000000000000, 113.9999999999999858 ) ) ;
#29884 = CARTESIAN_POINT ( 'NONE',  ( 11.99999999999999645, -141.0000000000000000, -155.0000000000000284 ) ) ;
#29885 = CARTESIAN_POINT ( 'NONE',  ( -99.92078033151290128, -0.6954373895739828226, 7.475453221064620735 ) ) ;
#29886 = CONTEXT_DEPENDENT_SHAPE_REPRESENTATION ( #5766, #17154 ) ;
#29887 = ORIENTED_EDGE ( 'NONE', *, *, #33632, .F. ) ;
#29888 = VERTEX_POINT ( 'NONE', #19232 ) ;
#29889 = CARTESIAN_POINT ( 'NONE',  ( 1.991296462759135633, -32.48444414290481319, 49.43553178847298568 ) ) ;
#29890 = CIRCLE ( 'NONE', #20224, 10.30000000000000071 ) ;
#29891 = ADVANCED_FACE ( 'NONE', ( #25063 ), #5843, .T. ) ;
#29892 = DIRECTION ( 'NONE',  ( 1.000000000000000000, 0.000000000000000000, -0.000000000000000000 ) ) ;
#29893 = EDGE_CURVE ( 'NONE', #6460, #12542, #32907, .T. ) ;
#29894 = VECTOR ( 'NONE', #34972, 1000.000000000000114 ) ;
#29895 = EDGE_CURVE ( 'NONE', #30046, #21299, #22827, .T. ) ;
#29896 = DIRECTION ( 'NONE',  ( 0.000000000000000000, 0.000000000000000000, 1.000000000000000000 ) ) ;
#29897 = ORIENTED_EDGE ( 'NONE', *, *, #31697, .F. ) ;
#29898 = VERTEX_POINT ( 'NONE', #33267 ) ;
#29899 = DIRECTION ( 'NONE',  ( 0.000000000000000000, -1.000000000000000000, 3.374343856708137958E-53 ) ) ;
#29900 = EDGE_LOOP ( 'NONE', ( #28726, #14240, #4265, #27556 ) ) ;
#29901 = DIRECTION ( 'NONE',  ( 0.000000000000000000, -7.888609052210118054E-31, -1.000000000000000000 ) ) ;
#29902 = DIRECTION ( 'NONE',  ( -0.000000000000000000, -0.000000000000000000, -1.000000000000000000 ) ) ;
#29903 = ORIENTED_EDGE ( 'NONE', *, *, #26483, .F. ) ;
#29904 = EDGE_LOOP ( 'NONE', ( #25327, #32178, #27379, #1122 ) ) ;
#29905 = VECTOR ( 'NONE', #3432, 1000.000000000000227 ) ;
#29906 = FACE_OUTER_BOUND ( 'NONE', #16633, .T. ) ;
#29907 = DIRECTION ( 'NONE',  ( 0.000000000000000000, 0.000000000000000000, -1.000000000000000000 ) ) ;
#29908 = VERTEX_POINT ( 'NONE', #706 ) ;
#29909 = VECTOR ( 'NONE', #27264, 1000.000000000000000 ) ;
#29910 = DIRECTION ( 'NONE',  ( 1.000000000000000000, -0.000000000000000000, -0.000000000000000000 ) ) ;
#29911 = LINE ( 'NONE', #10865, #15474 ) ;
#29912 = CARTESIAN_POINT ( 'NONE',  ( 0.1859802889711900942, -0.8217981779190254299, -32.27126551972443735 ) ) ;
#29913 = CARTESIAN_POINT ( 'NONE',  ( -6.500000000000000000, 0.000000000000000000, 3.930000000000000160 ) ) ;
#29914 =( REPRESENTATION_RELATIONSHIP ('NONE','NONE', #23037, #28231 ) REPRESENTATION_RELATIONSHIP_WITH_TRANSFORMATION ( #33158 )SHAPE_REPRESENTATION_RELATIONSHIP( ) );
#29915 = LINE ( 'NONE', #2845, #11441 ) ;
#29916 = CARTESIAN_POINT ( 'NONE',  ( -20.00000000000007461, -145.0000000000000000, -187.0000000000000000 ) ) ;
#29917 = CARTESIAN_POINT ( 'NONE',  ( 2.033800780627561533, 5.833185478271119884, 33.40977515897103700 ) ) ;
#29918 = VECTOR ( 'NONE', #7040, 1000.000000000000000 ) ;
#29919 = ORIENTED_EDGE ( 'NONE', *, *, #15022, .T. ) ;
#29920 = CARTESIAN_POINT ( 'NONE',  ( 0.7752961785294064656, 31.37228877271656913, 12.97290618475348012 ) ) ;
#29921 =( LENGTH_UNIT ( ) NAMED_UNIT ( * ) SI_UNIT ( .MILLI., .METRE. ) );
#29922 = VERTEX_POINT ( 'NONE', #33085 ) ;
#29923 = ORIENTED_EDGE ( 'NONE', *, *, #508, .F. ) ;
#29924 = CIRCLE ( 'NONE', #8323, 30.47050528711511674 ) ;
#29925 = DIRECTION ( 'NONE',  ( 0.000000000000000000, 0.000000000000000000, -1.000000000000000000 ) ) ;
#29926 = APPLICATION_PROTOCOL_DEFINITION ( 'draft international standard', 'automotive_design', 1998, #23061 ) ;
#29927 = EDGE_CURVE ( 'NONE', #3503, #16280, #19428, .T. ) ;
#29928 = ORIENTED_EDGE ( 'NONE', *, *, #10411, .T. ) ;
#29929 = CARTESIAN_POINT ( 'NONE',  ( -262.5000000000000000, 0.000000000000000000, 7.500000000000000000 ) ) ;
#29930 = LINE ( 'NONE', #8385, #3938 ) ;
#29931 = EDGE_CURVE ( 'NONE', #29748, #8703, #7453, .T. ) ;
#29932 = EDGE_CURVE ( 'NONE', #2181, #17362, #8702, .T. ) ;
#29933 = CARTESIAN_POINT ( 'NONE',  ( 2.789999999999999147, -3.728217946243117087, 30.24156218513554606 ) ) ;
#29934 = VERTEX_POINT ( 'NONE', #17091 ) ;
#29935 = ORIENTED_EDGE ( 'NONE', *, *, #11395, .T. ) ;
#29936 = CARTESIAN_POINT ( 'NONE',  ( 2.789999999999999147, 11.80989368511502846, -28.76039115933972923 ) ) ;
#29937 = CARTESIAN_POINT ( 'NONE',  ( -365.0000000000000000, 118.9999999999999716, 113.9999999999999858 ) ) ;
#29938 = EDGE_CURVE ( 'NONE', #7170, #6836, #10854, .T. ) ;
#29939 = AXIS2_PLACEMENT_3D ( 'NONE', #20381, #33718, #6829 ) ;
#29940 = CARTESIAN_POINT ( 'NONE',  ( 9.630725478591894984, 36.62364762272929397, 68.31122994652405112 ) ) ;
#29941 = LINE ( 'NONE', #2867, #12017 ) ;
#29942 = DIRECTION ( 'NONE',  ( 1.000000000000000000, 0.000000000000000000, 0.000000000000000000 ) ) ;
#29943 = VERTEX_POINT ( 'NONE', #24534 ) ;
#29944 = CARTESIAN_POINT ( 'NONE',  ( -0.9727285265192152641, -1.747512292859696670, -0.7500000000000000000 ) ) ;
#29945 = DIRECTION ( 'NONE',  ( 0.000000000000000000, -6.123233995736766036E-17, -1.000000000000000000 ) ) ;
#29946 = FACE_OUTER_BOUND ( 'NONE', #33633, .T. ) ;
#29947 = PRODUCT_DEFINITION_SHAPE ( 'NONE', 'NONE',  #32294 ) ;
#29948 = DIRECTION ( 'NONE',  ( 1.000000000000000000, 0.000000000000000000, 0.000000000000000000 ) ) ;
#29949 = EDGE_CURVE ( 'NONE', #7621, #11365, #25663, .T. ) ;
#29950 = DIRECTION ( 'NONE',  ( -0.000000000000000000, -0.000000000000000000, -1.000000000000000000 ) ) ;
#29952 = DIRECTION ( 'NONE',  ( -1.000000000000000000, -0.000000000000000000, -0.000000000000000000 ) ) ;
#29951 = LINE ( 'NONE', #5543, #11061 ) ;
#29953 = CIRCLE ( 'NONE', #32230, 2.524999999999999467 ) ;
#29954 = CARTESIAN_POINT ( 'NONE',  ( 2.765921099433442443, 7.350529080603967813, -30.20932655202929595 ) ) ;
#29955 = ORIENTED_EDGE ( 'NONE', *, *, #14478, .T. ) ;
#29956 = CARTESIAN_POINT ( 'NONE',  ( -449.9999999999999432, 105.0000000000000142, -175.0000000000000000 ) ) ;
#29958 = FACE_BOUND ( 'NONE', #1709, .T. ) ;
#29957 = CARTESIAN_POINT ( 'NONE',  ( 2.789999999999999147, 18.59128259035506758, -24.91982945642901726 ) ) ;
#29959 = ORIENTED_EDGE ( 'NONE', *, *, #7333, .F. ) ;
#29960 =( NAMED_UNIT ( * ) PLANE_ANGLE_UNIT ( ) SI_UNIT ( $, .RADIAN. ) );
#29961 = ORIENTED_EDGE ( 'NONE', *, *, #18428, .F. ) ;
#29962 = ORIENTED_EDGE ( 'NONE', *, *, #4112, .T. ) ;
#29963 = CARTESIAN_POINT ( 'NONE',  ( 0.000000000000000000, 3.214697847761802057E-14, -87.50000000000000000 ) ) ;
#29964 = ORIENTED_EDGE ( 'NONE', *, *, #24646, .T. ) ;
#29965 = EDGE_LOOP ( 'NONE', ( #21953, #10288, #1512, #5729 ) ) ;
#29966 = DIRECTION ( 'NONE',  ( -1.000000000000000000, -0.000000000000000000, -0.000000000000000000 ) ) ;
#29967 = CONTEXT_DEPENDENT_SHAPE_REPRESENTATION ( #26938, #23397 ) ;
#29968 = VECTOR ( 'NONE', #306, 1000.000000000000000 ) ;
#29969 = AXIS2_PLACEMENT_3D ( 'NONE', #23549, #26391, #5019 ) ;
#29970 = DIRECTION ( 'NONE',  ( 0.000000000000000000, -1.000000000000000000, -2.465190328815662439E-32 ) ) ;
#29971 = CYLINDRICAL_SURFACE ( 'NONE', #18282, 7.999999999999979572 ) ;
#29972 = ORIENTED_EDGE ( 'NONE', *, *, #4668, .T. ) ;
#29973 = VERTEX_POINT ( 'NONE', #21707 ) ;
#29974 = DIRECTION ( 'NONE',  ( 1.000000000000000000, 0.000000000000000000, 0.000000000000000000 ) ) ;
#29975 =( NAMED_UNIT ( * ) PLANE_ANGLE_UNIT ( ) SI_UNIT ( $, .RADIAN. ) );
#29976 = EDGE_CURVE ( 'NONE', #16944, #20519, #14242, .T. ) ;
#29977 = ADVANCED_FACE ( 'NONE', ( #3187 ), #531, .T. ) ;
#29978 = CARTESIAN_POINT ( 'NONE',  ( 99.86204640771551055, -2.561659524636490826, -12.23586498300002035 ) ) ;
#29979 = LINE ( 'NONE', #77, #34725 ) ;
#29980 = EDGE_LOOP ( 'NONE', ( #60, #711, #6101, #6621 ) ) ;
#29981 = AXIS2_PLACEMENT_3D ( 'NONE', #19183, #10635, #13132 ) ;
#29982 = DIRECTION ( 'NONE',  ( 0.000000000000000000, -1.000000000000000000, 0.000000000000000000 ) ) ;
#29983 = ADVANCED_FACE ( 'NONE', ( #19579 ), #16393, .T. ) ;
#29984 = EDGE_CURVE ( 'NONE', #4470, #19925, #2937, .T. ) ;
#29985 = DIRECTION ( 'NONE',  ( 0.000000000000000000, 0.000000000000000000, -1.000000000000000000 ) ) ;
#29986 = ORIENTED_EDGE ( 'NONE', *, *, #9076, .T. ) ;
#29987 = LINE ( 'NONE', #30333, #1445 ) ;
#29988 = FACE_OUTER_BOUND ( 'NONE', #27475, .T. ) ;
#29989 = DIRECTION ( 'NONE',  ( -1.000000000000000000, -0.000000000000000000, -0.000000000000000000 ) ) ;
#29990 = CARTESIAN_POINT ( 'NONE',  ( -20.00000000000007461, 112.9999999999999574, -162.9999999999999716 ) ) ;
#29991 = VERTEX_POINT ( 'NONE', #23296 ) ;
#29992 = VECTOR ( 'NONE', #6194, 1000.000000000000000 ) ;
#29993 = DIRECTION ( 'NONE',  ( 0.000000000000000000, 0.000000000000000000, -1.000000000000000000 ) ) ;
#29994 = ORIENTED_EDGE ( 'NONE', *, *, #5718, .T. ) ;
#29996 = CARTESIAN_POINT ( 'NONE',  ( 1.749999999999999778, -30.02688531850381182, -16.81585001935615153 ) ) ;
#29995 = FACE_OUTER_BOUND ( 'NONE', #17451, .T. ) ;
#29997 = CARTESIAN_POINT ( 'NONE',  ( 35.44043929807611448, -12.65143121711728291, 10.00000000000000000 ) ) ;
#29998 = EDGE_CURVE ( 'NONE', #22841, #21039, #17275, .T. ) ;
#29999 = AXIS2_PLACEMENT_3D ( 'NONE', #33127, #32946, #30470 ) ;
#30000 = AXIS2_PLACEMENT_3D ( 'NONE', #33806, #22607, #25254 ) ;
#30001 = ORIENTED_EDGE ( 'NONE', *, *, #5368, .F. ) ;
#30002 = CARTESIAN_POINT ( 'NONE',  ( 0.000000000000000000, -33.69708579775584667, -49.43553178847298568 ) ) ;
#30003 = CARTESIAN_POINT ( 'NONE',  ( 2.033589659274374295, -32.97789401874100434, -7.919772684713185740 ) ) ;
#30004 = VERTEX_POINT ( 'NONE', #31470 ) ;
#30005 = EDGE_CURVE ( 'NONE', #33194, #26426, #23948, .T. ) ;
#30006 = EDGE_CURVE ( 'NONE', #18684, #33194, #7075, .T. ) ;
#30007 = ORIENTED_EDGE ( 'NONE', *, *, #21571, .T. ) ;
#30008 = DIRECTION ( 'NONE',  ( 0.000000000000000000, 1.836970198721029688E-16, -1.000000000000000000 ) ) ;
#30009 = DIRECTION ( 'NONE',  ( 1.000000000000000000, 0.000000000000000000, -0.000000000000000000 ) ) ;
#30010 = ORIENTED_EDGE ( 'NONE', *, *, #12806, .F. ) ;
#30011 = ORIENTED_EDGE ( 'NONE', *, *, #9720, .F. ) ;
#30012 = LINE ( 'NONE', #33379, #27502 ) ;
#30013 = LINE ( 'NONE', #5605, #15894 ) ;
#30014 = AXIS2_PLACEMENT_3D ( 'NONE', #8429, #24431, #16285 ) ;
#30015 = CARTESIAN_POINT ( 'NONE',  ( -12.00000000000001066, 108.9999999999999858, -175.0000000000000284 ) ) ;
#30016 = CARTESIAN_POINT ( 'NONE',  ( 3.235562306570555532E-30, 1.325223266901699007E-14, -67.50000000000000000 ) ) ;
#30017 = ORIENTED_EDGE ( 'NONE', *, *, #761, .F. ) ;
#30018 = ORIENTED_EDGE ( 'NONE', *, *, #28938, .T. ) ;
#30019 = LINE ( 'NONE', #7767, #31571 ) ;
#30020 = CARTESIAN_POINT ( 'NONE',  ( 145.0000000000000568, -167.8552739801376390, -46.75049602362128809 ) ) ;
#30021 = DIRECTION ( 'NONE',  ( 0.9289767198167909745, -0.3701381553399156199, 0.000000000000000000 ) ) ;
#30022 = DIRECTION ( 'NONE',  ( -1.000000000000000000, -0.000000000000000000, -0.000000000000000000 ) ) ;
#30023 = AXIS2_PLACEMENT_3D ( 'NONE', #10839, #30057, #2286 ) ;
#30024 = DIRECTION ( 'NONE',  ( 0.000000000000000000, 1.836970198721029441E-16, -1.000000000000000000 ) ) ;
#30025 = EDGE_CURVE ( 'NONE', #5728, #11221, #33614, .T. ) ;
#30026 = ADVANCED_FACE ( 'NONE', ( #33798 ), #15469, .T. ) ;
#30027 = CARTESIAN_POINT ( 'NONE',  ( 5.713835024271038954, 32.03991982186465748, 49.43553178847298568 ) ) ;
#30029 = CIRCLE ( 'NONE', #7782, 32.54542015209057126 ) ;
#30028 = DIRECTION ( 'NONE',  ( 1.000000000000000000, 0.000000000000000000, 0.000000000000000000 ) ) ;
#30030 = VERTEX_POINT ( 'NONE', #12451 ) ;
#30031 = CARTESIAN_POINT ( 'NONE',  ( -500.0000000000000000, -113.0000000000000000, 159.0000000000000000 ) ) ;
#30032 = LINE ( 'NONE', #19015, #26804 ) ;
#30033 = EDGE_CURVE ( 'NONE', #2604, #5830, #23660, .T. ) ;
#30034 = AXIS2_PLACEMENT_3D ( 'NONE', #29047, #10551, #7324 ) ;
#30035 = CARTESIAN_POINT ( 'NONE',  ( 0.000000000000000000, -33.69708579775584667, 49.43553178847298568 ) ) ;
#30036 = ORIENTED_EDGE ( 'NONE', *, *, #28970, .T. ) ;
#30037 = DIRECTION ( 'NONE',  ( 0.000000000000000000, 0.3681245526846860794, -0.9297764858882481276 ) ) ;
#30038 = ORIENTED_EDGE ( 'NONE', *, *, #33628, .F. ) ;
#30039 = FACE_OUTER_BOUND ( 'NONE', #5251, .T. ) ;
#30040 = CARTESIAN_POINT ( 'NONE',  ( -108.8478167861455148, 3.386225727737903757, -12.03506400121763775 ) ) ;
#30041 = VECTOR ( 'NONE', #11244, 1000.000000000000114 ) ;
#30042 = VERTEX_POINT ( 'NONE', #34136 ) ;
#30043 = DIRECTION ( 'NONE',  ( 0.000000000000000000, -1.310824597558155437E-49, -1.000000000000000000 ) ) ;
#30044 = LINE ( 'NONE', #7634, #31005 ) ;
#30045 = DIRECTION ( 'NONE',  ( -1.000000000000000000, -0.000000000000000000, -0.000000000000000000 ) ) ;
#30046 = VERTEX_POINT ( 'NONE', #30774 ) ;
#30047 = EDGE_CURVE ( 'NONE', #9756, #30505, #12643, .T. ) ;
#30048 = PRESENTATION_LAYER_ASSIGNMENT (  '', '', ( #21543 ) ) ;
#30049 = EDGE_CURVE ( 'NONE', #14706, #23769, #29143, .T. ) ;
#30050 = EDGE_LOOP ( 'NONE', ( #849, #3423, #11912, #28535, #32357, #34287, #33405, #31924 ) ) ;
#30051 = DIRECTION ( 'NONE',  ( 0.1063910735369155841, -0.9943243633099125844, -3.335902418025060287E-15 ) ) ;
#30052 = LINE ( 'NONE', #32529, #14447 ) ;
#30053 = ORIENTED_EDGE ( 'NONE', *, *, #14123, .T. ) ;
#30054 = CARTESIAN_POINT ( 'NONE',  ( 0.000000000000000000, 0.000000000000000000, 3.000000000000000000 ) ) ;
#30055 = ADVANCED_FACE ( 'NONE', ( #29513 ), #28979, .F. ) ;
#30056 = VECTOR ( 'NONE', #27175, 1000.000000000000000 ) ;
#30057 = DIRECTION ( 'NONE',  ( 1.000000000000000000, 0.000000000000000000, 0.000000000000000000 ) ) ;
#30058 = ADVANCED_FACE ( 'NONE', ( #18153 ), #20970, .F. ) ;
#30059 = DIRECTION ( 'NONE',  ( 1.000000000000000000, 0.000000000000000000, 0.000000000000000000 ) ) ;
#30060 = CARTESIAN_POINT ( 'NONE',  ( -107.2949071119419813, -4.583230167788450160, 5.938965658480642951 ) ) ;
#30061 = CONTEXT_DEPENDENT_SHAPE_REPRESENTATION ( #2613, #25959 ) ;
#30062 = VERTEX_POINT ( 'NONE', #34495 ) ;
#30063 = ORIENTED_EDGE ( 'NONE', *, *, #27407, .F. ) ;
#30065 = ADVANCED_FACE ( 'NONE', ( #29336 ), #35034, .T. ) ;
#30064 = EDGE_LOOP ( 'NONE', ( #8071, #7859, #16302, #13332 ) ) ;
#30066 = CARTESIAN_POINT ( 'NONE',  ( -365.0000000000000000, -135.0000000000000000, 126.0000000000000000 ) ) ;
#30067 = CYLINDRICAL_SURFACE ( 'NONE', #1789, 12.50000000000000000 ) ;
#30068 = CYLINDRICAL_SURFACE ( 'NONE', #17356, 4.000000000000003553 ) ;
#30069 = VECTOR ( 'NONE', #9373, 1000.000000000000000 ) ;
#30070 = ORIENTED_EDGE ( 'NONE', *, *, #18730, .F. ) ;
#30071 = ORIENTED_EDGE ( 'NONE', *, *, #34271, .T. ) ;
#30072 = CYLINDRICAL_SURFACE ( 'NONE', #30515, 7.999999999999979572 ) ;
#30073 = EDGE_LOOP ( 'NONE', ( #12558, #3541, #19717, #10088 ) ) ;
#30074 = DIRECTION ( 'NONE',  ( -1.000000000000000000, 0.000000000000000000, 0.000000000000000000 ) ) ;
#30075 = CARTESIAN_POINT ( 'NONE',  ( 11.99999999999999645, -115.0000000000000000, 162.9999999999999716 ) ) ;
#30076 = VERTEX_POINT ( 'NONE', #26304 ) ;
#30077=STYLED_ITEM('',(#35254),#10767);
#30078 = ORIENTED_EDGE ( 'NONE', *, *, #26687, .F. ) ;
#30079 = LINE ( 'NONE', #21885, #25960 ) ;
#30080 = DIRECTION ( 'NONE',  ( 0.000000000000000000, 0.000000000000000000, -1.000000000000000000 ) ) ;
#30081 = VERTEX_POINT ( 'NONE', #18668 ) ;
#30082 = CARTESIAN_POINT ( 'NONE',  ( 0.000000000000000000, -49.99999999999999289, 0.000000000000000000 ) ) ;
#30083 = DIRECTION ( 'NONE',  ( 0.000000000000000000, 0.000000000000000000, -1.000000000000000000 ) ) ;
#30084 = DIRECTION ( 'NONE',  ( 1.000000000000000000, 0.000000000000000000, -0.000000000000000000 ) ) ;
#30085 = CIRCLE ( 'NONE', #27810, 2.524999999999999467 ) ;
#30086 = LINE ( 'NONE', #29560, #4864 ) ;
#30087 = DIRECTION ( 'NONE',  ( 0.000000000000000000, 1.836970198721029934E-16, -1.000000000000000000 ) ) ;
#30088 = CARTESIAN_POINT ( 'NONE',  ( 0.000000000000000000, 3.524919873834583163E-15, 68.31122994652405112 ) ) ;
#30089 = EDGE_CURVE ( 'NONE', #108, #2320, #26830, .T. ) ;
#30090 = EDGE_CURVE ( 'NONE', #19038, #14635, #1915, .T. ) ;
#30091 = ORIENTED_EDGE ( 'NONE', *, *, #28074, .F. ) ;
#30092 = CARTESIAN_POINT ( 'NONE',  ( 1.039999999999999591, 31.89769921722987434, 12.91988538846969803 ) ) ;
#30093 = DIRECTION ( 'NONE',  ( 2.631201909438060269E-14, -5.396010391056495992E-16, 0.9999999999999998890 ) ) ;
#30094 = ORIENTED_EDGE ( 'NONE', *, *, #26049, .F. ) ;
#30095 = EDGE_LOOP ( 'NONE', ( #18189, #12685, #13625, #17295 ) ) ;
#30096 =( GEOMETRIC_REPRESENTATION_CONTEXT ( 3 ) GLOBAL_UNCERTAINTY_ASSIGNED_CONTEXT ( ( #2049 ) ) GLOBAL_UNIT_ASSIGNED_CONTEXT ( ( #3564, #11599, #9091 ) ) REPRESENTATION_CONTEXT ( 'NONE', 'WORKASPACE' ) );
#30097 = FACE_OUTER_BOUND ( 'NONE', #20148, .T. ) ;
#30098 = PRODUCT_CONTEXT ( 'NONE', #10309, 'mechanical' ) ;
#30099 = ORIENTED_EDGE ( 'NONE', *, *, #24145, .F. ) ;
#30100 = DIRECTION ( 'NONE',  ( 0.000000000000000000, 1.836970198721029441E-16, -1.000000000000000000 ) ) ;
#30101 = CARTESIAN_POINT ( 'NONE',  ( -8.499999999999998224, 0.000000000000000000, 3.180000000000000160 ) ) ;
#30103 = PLANE ( 'NONE',  #11870 ) ;
#30102 = CARTESIAN_POINT ( 'NONE',  ( -12.00000000000001066, 144.9999999999999716, -154.9999999999999716 ) ) ;
#30104 = VERTEX_POINT ( 'NONE', #26479 ) ;
#30105 = VERTEX_POINT ( 'NONE', #5104 ) ;
#30106 = DIRECTION ( 'NONE',  ( 0.000000000000000000, 1.000000000000000000, 0.000000000000000000 ) ) ;
#30107 = CARTESIAN_POINT ( 'NONE',  ( 5.021133111224473033, 8.235406450278427215, -67.50000000000000000 ) ) ;
#30108 = FACE_OUTER_BOUND ( 'NONE', #25145, .T. ) ;
#30109 = DIRECTION ( 'NONE',  ( 1.000000000000000000, -0.000000000000000000, -0.000000000000000000 ) ) ;
#30110 = DIRECTION ( 'NONE',  ( 0.000000000000000000, -3.435095992033281961E-15, -1.000000000000000000 ) ) ;
#30111 = ORIENTED_EDGE ( 'NONE', *, *, #4940, .F. ) ;
#30112 = CARTESIAN_POINT ( 'NONE',  ( 0.000000000000000000, 20.79173593595294633, -22.27454621808743340 ) ) ;
#30113 = CARTESIAN_POINT ( 'NONE',  ( -499.9999999999999432, 108.9999999999999858, -187.0000000000000000 ) ) ;
#30114 = DIRECTION ( 'NONE',  ( -0.000000000000000000, 0.000000000000000000, 1.000000000000000000 ) ) ;
#30115 = AXIS2_PLACEMENT_3D ( 'NONE', #7284, #1611, #26338 ) ;
#30116 =( REPRESENTATION_RELATIONSHIP ('NONE','NONE', #23037, #15767 ) REPRESENTATION_RELATIONSHIP_WITH_TRANSFORMATION ( #13516 )SHAPE_REPRESENTATION_RELATIONSHIP( ) );
#30117 = CARTESIAN_POINT ( 'NONE',  ( -445.9999999999999432, 105.0000000000000142, 162.9999999999999716 ) ) ;
#30118 = DIRECTION ( 'NONE',  ( 1.000000000000000000, 0.000000000000000000, 0.000000000000000000 ) ) ;
#30120 = DIRECTION ( 'NONE',  ( 0.5611870653623822758, 0.8276889981568905652, -0.000000000000000000 ) ) ;
#30119 = PLANE ( 'NONE',  #31527 ) ;
#30121 = DIRECTION ( 'NONE',  ( 0.000000000000000000, 0.000000000000000000, 1.000000000000000000 ) ) ;
#30122 = ORIENTED_EDGE ( 'NONE', *, *, #3155, .T. ) ;
#30123 = LINE ( 'NONE', #24419, #30396 ) ;
#30125 = CARTESIAN_POINT ( 'NONE',  ( -19.99999999999998934, -56.99999999999997868, -175.0000000000000000 ) ) ;
#30124 = DIRECTION ( 'NONE',  ( -0.000000000000000000, -0.000000000000000000, -1.000000000000000000 ) ) ;
#30126 = EDGE_CURVE ( 'NONE', #18315, #8996, #34673, .T. ) ;
#30127 = AXIS2_PLACEMENT_3D ( 'NONE', #18204, #5167, #21565 ) ;
#30128 = EDGE_CURVE ( 'NONE', #7115, #34482, #22264, .T. ) ;
#30129 = VERTEX_POINT ( 'NONE', #21499 ) ;
#30130 = EDGE_CURVE ( 'NONE', #32547, #14097, #23459, .T. ) ;
#30131 = ORIENTED_EDGE ( 'NONE', *, *, #32251, .F. ) ;
#30132 = ORIENTED_EDGE ( 'NONE', *, *, #3324, .F. ) ;
#30133 = FACE_OUTER_BOUND ( 'NONE', #21372, .T. ) ;
#30134 = EDGE_LOOP ( 'NONE', ( #26586, #26770, #16837, #25860 ) ) ;
#30135 = VERTEX_POINT ( 'NONE', #15993 ) ;
#30136 = DIRECTION ( 'NONE',  ( 0.000000000000000000, 1.836970198721029441E-16, -1.000000000000000000 ) ) ;
#30137 = B_SPLINE_CURVE_WITH_KNOTS ( 'NONE', 3,
 ( #26089, #1705, #15075, #31601, #12573, #6513 ),
 .UNSPECIFIED., .F., .F.,
 ( 4, 2, 4 ),
 ( 4.404817006176418240E-07, 0.001874269609036405965, 0.003748098736372194612 ),
 .UNSPECIFIED. ) ;
#30138 = CYLINDRICAL_SURFACE ( 'NONE', #7259, 3.999999999999982681 ) ;
#30139 = CYLINDRICAL_SURFACE ( 'NONE', #18836, 10.00000000000000000 ) ;
#30140 = ORIENTED_EDGE ( 'NONE', *, *, #6200, .F. ) ;
#30141 = EDGE_LOOP ( 'NONE', ( #5668, #15183, #1474, #31872 ) ) ;
#30142 = CARTESIAN_POINT ( 'NONE',  ( 19.99999999999996092, -134.9999999999999716, 162.9999999999999716 ) ) ;
#30143 = CARTESIAN_POINT ( 'NONE',  ( -365.0000000000000000, 134.9999999999999716, 113.9999999999999858 ) ) ;
#30144 = CARTESIAN_POINT ( 'NONE',  ( 106.8679498092085538, -5.438347208236144148, -11.25609171608219938 ) ) ;
#30145 = LINE ( 'NONE', #5407, #5156 ) ;
#30146 = EDGE_LOOP ( 'NONE', ( #15982, #24970, #18506, #16218, #33186 ) ) ;
#30147 = VECTOR ( 'NONE', #14505, 1000.000000000000000 ) ;
#30148 = CARTESIAN_POINT ( 'NONE',  ( -12.00000000000001066, 124.9999999999999716, 155.0000000000000000 ) ) ;
#30149 = CARTESIAN_POINT ( 'NONE',  ( -500.0000000000000000, -109.0000000000000142, 187.0000000000000000 ) ) ;
#30150 = EDGE_LOOP ( 'NONE', ( #12345, #2638, #31557, #34458 ) ) ;
#30151 = CARTESIAN_POINT ( 'NONE',  ( 0.000000000000000000, 0.000000000000000000, -0.7500000000000000000 ) ) ;
#30152 = CARTESIAN_POINT ( 'NONE',  ( -15.64512930492132448, -28.53829535743847856, 68.31122994652405112 ) ) ;
#30153 = CARTESIAN_POINT ( 'NONE',  ( 19.99999999999998934, -137.0000000000000000, 174.9999999999999432 ) ) ;
#30154 = LINE ( 'NONE', #21625, #25716 ) ;
#30155 = ORIENTED_EDGE ( 'NONE', *, *, #16293, .F. ) ;
#30156 = AXIS2_PLACEMENT_3D ( 'NONE', #15729, #26558, #26382 ) ;
#30157 = AXIS2_PLACEMENT_3D ( 'NONE', #11810, #12154, #31185 ) ;
#30158 = DIRECTION ( 'NONE',  ( 0.000000000000000000, 0.000000000000000000, 1.000000000000000000 ) ) ;
#30159 = VERTEX_POINT ( 'NONE', #32340 ) ;
#30161 = CARTESIAN_POINT ( 'NONE',  ( 14.70109753509668948, 34.88954974633765005, 68.31122994652405112 ) ) ;
#30160 = DIRECTION ( 'NONE',  ( 1.000000000000000000, 0.000000000000000000, 0.000000000000000000 ) ) ;
#30162 = DIRECTION ( 'NONE',  ( 0.000000000000000000, 0.000000000000000000, 1.000000000000000000 ) ) ;
#30163 = EDGE_CURVE ( 'NONE', #26980, #13600, #5801, .T. ) ;
#30164 = ORIENTED_EDGE ( 'NONE', *, *, #19369, .F. ) ;
#30165 = CARTESIAN_POINT ( 'NONE',  ( -6.500000000000000000, 0.000000000000000000, 3.931000000000000494 ) ) ;
#30166 = DIRECTION ( 'NONE',  ( 0.000000000000000000, 0.000000000000000000, 1.000000000000000000 ) ) ;
#30167 = AXIS2_PLACEMENT_3D ( 'NONE', #8606, #26953, #24803 ) ;
#30168 = ADVANCED_FACE ( 'NONE', ( #24152 ), #13142, .T. ) ;
#30169 = EDGE_CURVE ( 'NONE', #10663, #22622, #25295, .T. ) ;
#30170 = VERTEX_POINT ( 'NONE', #1745 ) ;
#30171 = VECTOR ( 'NONE', #31416, 1000.000000000000000 ) ;
#30172 = EDGE_CURVE ( 'NONE', #22441, #34152, #30032, .T. ) ;
#30173 = ADVANCED_FACE ( 'NONE', ( #29860 ), #13487, .T. ) ;
#30174 = ORIENTED_EDGE ( 'NONE', *, *, #26634, .T. ) ;
#30175 = CARTESIAN_POINT ( 'NONE',  ( 5.021133111224265200, -15.68591377522703745, -67.50000000000000000 ) ) ;
#30176 = DIRECTION ( 'NONE',  ( -0.000000000000000000, -0.000000000000000000, -1.000000000000000000 ) ) ;
#30177 = ORIENTED_EDGE ( 'NONE', *, *, #29739, .T. ) ;
#30178 = VERTEX_POINT ( 'NONE', #32509 ) ;
#30179 = CARTESIAN_POINT ( 'NONE',  ( -20.02113311122488781, 8.235406450278427215, -67.50000000000000000 ) ) ;
#30180 = EDGE_CURVE ( 'NONE', #6409, #30837, #16026, .T. ) ;
#30181 = DIRECTION ( 'NONE',  ( -1.000000000000000000, 0.000000000000000000, -0.000000000000000000 ) ) ;
#30182 = DIRECTION ( 'NONE',  ( 1.000000000000000000, 0.000000000000000000, 0.000000000000000000 ) ) ;
#30183 = VECTOR ( 'NONE', #22850, 1000.000000000000000 ) ;
#30184 = DIRECTION ( 'NONE',  ( 0.000000000000000000, 1.000000000000000000, 5.053935297177146739E-49 ) ) ;
#30185 = ORIENTED_EDGE ( 'NONE', *, *, #34922, .T. ) ;
#30186 = EDGE_LOOP ( 'NONE', ( #18900, #18333, #7522, #30672, #16557, #7000, #16990, #34891 ) ) ;
#30187 = CIRCLE ( 'NONE', #3479, 32.54542015209056416 ) ;
#30188 = FACE_OUTER_BOUND ( 'NONE', #17565, .T. ) ;
#30189 = DIRECTION ( 'NONE',  ( 1.000000000000000000, 0.000000000000000000, 5.546364386991661285E-52 ) ) ;
#30190 = AXIS2_PLACEMENT_3D ( 'NONE', #2755, #24635, #18632 ) ;
#30191 = FACE_OUTER_BOUND ( 'NONE', #32298, .T. ) ;
#30192 = FACE_OUTER_BOUND ( 'NONE', #32156, .T. ) ;
#30193 = CARTESIAN_POINT ( 'NONE',  ( -25.07182831876307105, -28.36910952062234870, 68.31122994652405112 ) ) ;
#30194 = FACE_OUTER_BOUND ( 'NONE', #4418, .T. ) ;
#30195 = CYLINDRICAL_SURFACE ( 'NONE', #5036, 7.999999999999979572 ) ;
#30196 = ORIENTED_EDGE ( 'NONE', *, *, #13033, .F. ) ;
#30197 = VECTOR ( 'NONE', #29760, 1000.000000000000000 ) ;
#30198 = CARTESIAN_POINT ( 'NONE',  ( -500.0000000000000000, -137.0000000000000000, 159.0000000000000000 ) ) ;
#30199 = DIRECTION ( 'NONE',  ( 0.000000000000000000, 0.000000000000000000, 1.000000000000000000 ) ) ;
#30200 = CIRCLE ( 'NONE', #16581, 1.999999999999999112 ) ;
#30201 = CARTESIAN_POINT ( 'NONE',  ( 0.000000000000000000, -5.984944020945660803, -28.84917528048448787 ) ) ;
#30202 = ORIENTED_EDGE ( 'NONE', *, *, #6531, .F. ) ;
#30203 = DIRECTION ( 'NONE',  ( -0.05413890858541543089, -0.9985334138511240409, 0.000000000000000000 ) ) ;
#30204 = ORIENTED_EDGE ( 'NONE', *, *, #19340, .F. ) ;
#30205 = LINE ( 'NONE', #32038, #7661 ) ;
#30206 = CARTESIAN_POINT ( 'NONE',  ( -105.6777138778371068, 5.081071289440263428, 11.42094332255972589 ) ) ;
#30208 = ORIENTED_EDGE ( 'NONE', *, *, #23153, .F. ) ;
#30207 = CIRCLE ( 'NONE', #4596, 2.000000000000001776 ) ;
#30209 = VECTOR ( 'NONE', #2932, 1000.000000000000000 ) ;
#30210 = CARTESIAN_POINT ( 'NONE',  ( -442.0000000000000000, -105.0000000000000142, 155.0000000000000000 ) ) ;
#30211 = CARTESIAN_POINT ( 'NONE',  ( 2.789999999999999147, -15.78270255339092287, 26.02842157509082455 ) ) ;
#30212 = DIRECTION ( 'NONE',  ( -0.000000000000000000, 1.000000000000000000, -0.000000000000000000 ) ) ;
#30213 = AXIS2_PLACEMENT_3D ( 'NONE', #30478, #25474, #33488 ) ;
#30214 = ORIENTED_EDGE ( 'NONE', *, *, #11503, .T. ) ;
#30215 = EDGE_CURVE ( 'NONE', #27224, #27344, #5796, .T. ) ;
#30216 = EDGE_CURVE ( 'NONE', #12565, #10302, #21834, .T. ) ;
#30217 = CARTESIAN_POINT ( 'NONE',  ( 821.7838007394873330, 1304.220615509354502, 1753.598338701303419 ) ) ;
#30218 = CARTESIAN_POINT ( 'NONE',  ( 0.07098932344682959417, -31.66360817300142827, 1.400248398912060210 ) ) ;
#30219 = EDGE_LOOP ( 'NONE', ( #10090, #7936, #19805, #4664 ) ) ;
#30220 = DIRECTION ( 'NONE',  ( -1.000000000000000000, 0.000000000000000000, 0.000000000000000000 ) ) ;
#30221 = AXIS2_PLACEMENT_3D ( 'NONE', #4920, #32163, #26468 ) ;
#30222 = CARTESIAN_POINT ( 'NONE',  ( -37.12776225901827587, -7.411627343331148587, 17.41927665145494686 ) ) ;
#30223 = FACE_OUTER_BOUND ( 'NONE', #12128, .T. ) ;
#30224 = CARTESIAN_POINT ( 'NONE',  ( -101.1692820431775033, -3.393468573754153006, 6.689828017866632948 ) ) ;
#30225 = ORIENTED_EDGE ( 'NONE', *, *, #21523, .F. ) ;
#30226 = ORIENTED_EDGE ( 'NONE', *, *, #29850, .T. ) ;
#30227 = EDGE_LOOP ( 'NONE', ( #30277, #34861, #7380, #5141 ) ) ;
#30228 = CARTESIAN_POINT ( 'NONE',  ( -442.0000000000000000, 105.0000000000000142, -109.9999999999999574 ) ) ;
#30229 = EDGE_CURVE ( 'NONE', #30758, #10803, #5279, .T. ) ;
#30230 = DIRECTION ( 'NONE',  ( -1.000000000000000000, -0.000000000000000000, 0.000000000000000000 ) ) ;
#30231 = AXIS2_PLACEMENT_3D ( 'NONE', #19942, #16408, #27237 ) ;
#30232 = CARTESIAN_POINT ( 'NONE',  ( 2.765921099433441999, -21.56796757982826307, 22.39322359481599278 ) ) ;
#30234 = VERTEX_POINT ( 'NONE', #32692 ) ;
#30233 = VECTOR ( 'NONE', #2102, 1000.000000000000114 ) ;
#30235 = ORIENTED_EDGE ( 'NONE', *, *, #25004, .F. ) ;
#30236 = CARTESIAN_POINT ( 'NONE',  ( -449.9999999999999432, -137.0000000000000000, 155.0000000000000000 ) ) ;
#30237 = VECTOR ( 'NONE', #5767, 1000.000000000000000 ) ;
#30238 = ORIENTED_EDGE ( 'NONE', *, *, #18264, .T. ) ;
#30239 = PRESENTATION_LAYER_ASSIGNMENT (  '', '', ( #4077 ) ) ;
#30240 = ADVANCED_FACE ( 'NONE', ( #27705 ), #27347, .T. ) ;
#30241 = DIRECTION ( 'NONE',  ( -1.000000000000000000, 0.000000000000000000, 0.000000000000000000 ) ) ;
#30242 = DIRECTION ( 'NONE',  ( 0.000000000000000000, 1.000000000000000000, 1.224646799147353207E-16 ) ) ;
#30243 = VERTEX_POINT ( 'NONE', #16169 ) ;
#30244 = EDGE_CURVE ( 'NONE', #7395, #18440, #27389, .T. ) ;
#30246 = EDGE_CURVE ( 'NONE', #25980, #9992, #4073, .T. ) ;
#30245 = EDGE_LOOP ( 'NONE', ( #20989, #34248, #15433, #14096, #13595 ) ) ;
#30247 = LINE ( 'NONE', #11037, #29703 ) ;
#30248 = EDGE_LOOP ( 'NONE', ( #10387, #28376, #13272, #3382 ) ) ;
#30249 = DIRECTION ( 'NONE',  ( 0.000000000000000000, 0.000000000000000000, 1.000000000000000000 ) ) ;
#30250 = CARTESIAN_POINT ( 'NONE',  ( -45.00000000000000000, -4.831299144296466785, 15.81122994652406355 ) ) ;
#30251 = ADVANCED_FACE ( 'NONE', ( #8315 ), #16521, .T. ) ;
#30252 = DIRECTION ( 'NONE',  ( 0.000000000000000000, -1.000000000000000000, -2.465190328815662439E-32 ) ) ;
#30253 = FACE_OUTER_BOUND ( 'NONE', #496, .T. ) ;
#30254 = CARTESIAN_POINT ( 'NONE',  ( 3.235562306570555532E-30, 14.09580098603202458, -67.50000000000000000 ) ) ;
#30255 = DIRECTION ( 'NONE',  ( 0.000000000000000000, 0.000000000000000000, 1.000000000000000000 ) ) ;
#30256 = PLANE ( 'NONE',  #34280 ) ;
#30257 = AXIS2_PLACEMENT_3D ( 'NONE', #24597, #2546, #238 ) ;
#30258 = VERTEX_POINT ( 'NONE', #24489 ) ;
#30259 = CIRCLE ( 'NONE', #8664, 3.999999999999976019 ) ;
#30260 =( GEOMETRIC_REPRESENTATION_CONTEXT ( 3 ) GLOBAL_UNCERTAINTY_ASSIGNED_CONTEXT ( ( #27799 ) ) GLOBAL_UNIT_ASSIGNED_CONTEXT ( ( #1843, #7345, #29257 ) ) REPRESENTATION_CONTEXT ( 'NONE', 'WORKASPACE' ) );
#30261 = EDGE_CURVE ( 'NONE', #26414, #19893, #33814, .T. ) ;
#30262 = CYLINDRICAL_SURFACE ( 'NONE', #6321, 2.036051781435508801 ) ;
#30263 = CARTESIAN_POINT ( 'NONE',  ( 852.6505942970502474, 1015.741480641997555, 1753.598338701303419 ) ) ;
#30264 = AXIS2_PLACEMENT_3D ( 'NONE', #132, #32868, #5625 ) ;
#30265 = ORIENTED_EDGE ( 'NONE', *, *, #32473, .T. ) ;
#30266 = ORIENTED_EDGE ( 'NONE', *, *, #27521, .T. ) ;
#30267 = DIRECTION ( 'NONE',  ( 1.000000000000000000, -0.000000000000000000, -0.000000000000000000 ) ) ;
#30268 = LINE ( 'NONE', #5867, #19341 ) ;
#30269 = APPLICATION_PROTOCOL_DEFINITION ( 'draft international standard', 'automotive_design', 1998, #7809 ) ;
#30270 = ORIENTED_EDGE ( 'NONE', *, *, #6204, .F. ) ;
#30271 = CARTESIAN_POINT ( 'NONE',  ( 10.17231796313407344, -5.651112684911596240, -87.50000000000000000 ) ) ;
#30272 =( NAMED_UNIT ( * ) SI_UNIT ( $, .STERADIAN. ) SOLID_ANGLE_UNIT ( ) );
#30273 = CONTEXT_DEPENDENT_SHAPE_REPRESENTATION ( #20812, #23803 ) ;
#30275 = FACE_OUTER_BOUND ( 'NONE', #7743, .T. ) ;
#30274 = CARTESIAN_POINT ( 'NONE',  ( 1.749999999999999778, -18.66807150955433769, 28.91175816027496381 ) ) ;
#30276 = ORIENTED_EDGE ( 'NONE', *, *, #17469, .T. ) ;
#30277 = ORIENTED_EDGE ( 'NONE', *, *, #11587, .T. ) ;
#30278 = CARTESIAN_POINT ( 'NONE',  ( -15.64512930492131382, -28.53829535743846435, 68.31122994652405112 ) ) ;
#30279 = LINE ( 'NONE', #29940, #31782 ) ;
#30280 = CARTESIAN_POINT ( 'NONE',  ( -418.0000000000000000, 124.9999999999999574, -190.9999999999999716 ) ) ;
#30281 = PLANE ( 'NONE',  #26921 ) ;
#30282 = ORIENTED_EDGE ( 'NONE', *, *, #19412, .F. ) ;
#30283 = EDGE_CURVE ( 'NONE', #32497, #19094, #13839, .T. ) ;
#30284 =( GEOMETRIC_REPRESENTATION_CONTEXT ( 3 ) GLOBAL_UNCERTAINTY_ASSIGNED_CONTEXT ( ( #23139 ) ) GLOBAL_UNIT_ASSIGNED_CONTEXT ( ( #25664, #4458, #15348 ) ) REPRESENTATION_CONTEXT ( 'NONE', 'WORKASPACE' ) );
#30285 = DIRECTION ( 'NONE',  ( 0.000000000000000000, 0.000000000000000000, -1.000000000000000000 ) ) ;
#30286 = CARTESIAN_POINT ( 'NONE',  ( 11.99999999999999645, 134.9999999999999432, -194.9999999999999432 ) ) ;
#30287 = EDGE_CURVE ( 'NONE', #33511, #26400, #6179, .T. ) ;
#30288 = CARTESIAN_POINT ( 'NONE',  ( -11.99999999999998224, -134.9999999999999716, 194.9999999999999716 ) ) ;
#30289 = AXIS2_PLACEMENT_3D ( 'NONE', #5107, #24328, #7255 ) ;
#30290 = CIRCLE ( 'NONE', #10392, 7.999999999999979572 ) ;
#30291 = ORIENTED_EDGE ( 'NONE', *, *, #21122, .T. ) ;
#30292 = DIRECTION ( 'NONE',  ( -1.000000000000000000, -0.000000000000000000, 0.000000000000000000 ) ) ;
#30293 =( NAMED_UNIT ( * ) PLANE_ANGLE_UNIT ( ) SI_UNIT ( $, .RADIAN. ) );
#30294 = CYLINDRICAL_SURFACE ( 'NONE', #10423, 2.033421858999710619 ) ;
#30296 = LINE ( 'NONE', #1107, #25901 ) ;
#30295 = DIRECTION ( 'NONE',  ( 0.000000000000000000, 0.000000000000000000, -1.000000000000000000 ) ) ;
#30297 = CARTESIAN_POINT ( 'NONE',  ( 11.99999999999999645, 144.9999999999999147, 194.9999999999999716 ) ) ;
#30298 = ORIENTED_EDGE ( 'NONE', *, *, #20040, .T. ) ;
#30299 = DIRECTION ( 'NONE',  ( 0.000000000000000000, 1.310824597558155437E-49, 1.000000000000000000 ) ) ;
#30300 = CARTESIAN_POINT ( 'NONE',  ( 0.000000000000000000, 6.992329373473909019E-15, 49.43553178847298568 ) ) ;
#30301 = AXIS2_PLACEMENT_3D ( 'NONE', #1149, #17189, #20025 ) ;
#30302 = VERTEX_POINT ( 'NONE', #490 ) ;
#30303 = ORIENTED_EDGE ( 'NONE', *, *, #9405, .T. ) ;
#30304 = AXIS2_PLACEMENT_3D ( 'NONE', #23831, #32007, #21680 ) ;
#30305 = CIRCLE ( 'NONE', #9282, 4.000000000000003553 ) ;
#30306 = AXIS2_PLACEMENT_3D ( 'NONE', #34059, #2187, #12715 ) ;
#30307 = ORIENTED_EDGE ( 'NONE', *, *, #16496, .T. ) ;
#30308 = DIRECTION ( 'NONE',  ( 1.000000000000000000, 0.000000000000000000, 0.000000000000000000 ) ) ;
#30309 = ORIENTED_EDGE ( 'NONE', *, *, #9565, .T. ) ;
#30310 = VERTEX_POINT ( 'NONE', #2619 ) ;
#30311 = ADVANCED_FACE ( 'NONE', ( #11349 ), #19537, .F. ) ;
#30312 = CARTESIAN_POINT ( 'NONE',  ( 22.89764159710613001, 4.274639749586562232, -87.50000000000000000 ) ) ;
#30313 = ITEM_DEFINED_TRANSFORMATION ( 'NONE', 'NONE', #18968,  #28566 ) ;
#30314 = ORIENTED_EDGE ( 'NONE', *, *, #19989, .T. ) ;
#30315 = CARTESIAN_POINT ( 'NONE',  ( -410.0000000000000568, -105.0000000000000142, -101.9999999999999858 ) ) ;
#30316 = DIRECTION ( 'NONE',  ( 0.000000000000000000, 0.000000000000000000, -1.000000000000000000 ) ) ;
#30317 = ORIENTED_EDGE ( 'NONE', *, *, #32400, .F. ) ;
#30318 = VERTEX_POINT ( 'NONE', #11521 ) ;
#30319 = CARTESIAN_POINT ( 'NONE',  ( -414.0000000000000568, -105.0000000000000142, 187.0000000000000000 ) ) ;
#30320 = CARTESIAN_POINT ( 'NONE',  ( 0.000000000000000000, 31.93991905851385837, 0.000000000000000000 ) ) ;
#30321 = B_SPLINE_CURVE_WITH_KNOTS ( 'NONE', 3,
 ( #27621, #5371, #13581, #2531, #8573, #5712 ),
 .UNSPECIFIED., .F., .F.,
 ( 4, 2, 4 ),
 ( 1.978909662040517630E-07, 0.001873396183027085504, 0.003746594475087967023 ),
 .UNSPECIFIED. ) ;
#30322 = EDGE_CURVE ( 'NONE', #18216, #8179, #33221, .T. ) ;
#30323 = DIRECTION ( 'NONE',  ( -0.1617819965527614312, 0.9868265225415265851, 0.000000000000000000 ) ) ;
#30324 = LINE ( 'NONE', #16833, #7440 ) ;
#30325 = ORIENTED_EDGE ( 'NONE', *, *, #23258, .T. ) ;
#30326 = EDGE_CURVE ( 'NONE', #24869, #14949, #1538, .T. ) ;
#30327 = CARTESIAN_POINT ( 'NONE',  ( 2.789999999999999147, -25.83993731729808729, 18.77381338200959604 ) ) ;
#30328 = EDGE_CURVE ( 'NONE', #7557, #904, #12060, .T. ) ;
#30329 = AXIS2_PLACEMENT_3D ( 'NONE', #4211, #20602, #28784 ) ;
#30330 = LINE ( 'NONE', #30149, #7921 ) ;
#30331 = EDGE_LOOP ( 'NONE', ( #28036, #22454, #4710, #5909 ) ) ;
#30332 = PRODUCT_DEFINITION ( 'UNKNOWN', '', #9884, #34916 ) ;
#30333 = CARTESIAN_POINT ( 'NONE',  ( 11.62236370382047745, -30.39942490923498752, -36.68877005347593467 ) ) ;
#30334 = LINE ( 'NONE', #13795, #14939 ) ;
#30335 = LINE ( 'NONE', #30153, #4927 ) ;
#30336 = DIRECTION ( 'NONE',  ( -1.000000000000000000, -0.000000000000000000, -0.000000000000000000 ) ) ;
#30337 = ORIENTED_EDGE ( 'NONE', *, *, #28977, .F. ) ;
#30338 = VECTOR ( 'NONE', #34951, 1000.000000000000000 ) ;
#30339 = CIRCLE ( 'NONE', #6439, 4.750000000000004441 ) ;
#30340 = FACE_OUTER_BOUND ( 'NONE', #17196, .T. ) ;
#30341 = VERTEX_POINT ( 'NONE', #6333 ) ;
#30343 = FILL_AREA_STYLE ('',( #13802 ) ) ;
#30342 = CARTESIAN_POINT ( 'NONE',  ( 2.033800793007967123, 27.74641878906490788, -19.50321439924927702 ) ) ;
#30344 = ORIENTED_EDGE ( 'NONE', *, *, #6070, .T. ) ;
#30345 = LINE ( 'NONE', #8461, #10935 ) ;
#30346 = CARTESIAN_POINT ( 'NONE',  ( 2.789999999999999147, -30.41598411195407081, -1.821977758773984490 ) ) ;
#30347 = ORIENTED_EDGE ( 'NONE', *, *, #14333, .F. ) ;
#30348 = ORIENTED_EDGE ( 'NONE', *, *, #28013, .T. ) ;
#30349 = B_SPLINE_CURVE_WITH_KNOTS ( 'NONE', 3,
 ( #33607, #1222, #33260, #28280 ),
 .UNSPECIFIED., .F., .F.,
 ( 4, 4 ),
 ( 0.005298346188946770341, 0.005985214897255175526 ),
 .UNSPECIFIED. ) ;
#30350 = AXIS2_PLACEMENT_3D ( 'NONE', #14716, #28742, #20394 ) ;
#30351 = ORIENTED_EDGE ( 'NONE', *, *, #20015, .T. ) ;
#30352 = DIRECTION ( 'NONE',  ( 0.000000000000000000, 0.9980267284282708928, 0.06279051952932451774 ) ) ;
#30353 = LINE ( 'NONE', #11325, #5087 ) ;
#30354 = ORIENTED_EDGE ( 'NONE', *, *, #16342, .F. ) ;
#30355 = ORIENTED_EDGE ( 'NONE', *, *, #23070, .T. ) ;
#30356 = CARTESIAN_POINT ( 'NONE',  ( 129.3530333899765594, 6.000000000000000000, -62.49999999999999289 ) ) ;
#30357 = CIRCLE ( 'NONE', #4778, 3.999999999999976019 ) ;
#30358 = CARTESIAN_POINT ( 'NONE',  ( 1.749999999999999778, -18.21166265554811403, 29.20140402659732359 ) ) ;
#30359 = LINE ( 'NONE', #27686, #23273 ) ;
#30360 = AXIS2_PLACEMENT_3D ( 'NONE', #26355, #25830, #1973 ) ;
#30361 = LINE ( 'NONE', #472, #11219 ) ;
#30362 = DIRECTION ( 'NONE',  ( 0.9052067871510963704, 0.3606673485459945261, -0.2247659586956879396 ) ) ;
#30363 = ORIENTED_EDGE ( 'NONE', *, *, #18944, .T. ) ;
#30364 = ORIENTED_EDGE ( 'NONE', *, *, #22058, .T. ) ;
#30365 = AXIS2_PLACEMENT_3D ( 'NONE', #6827, #3455, #34066 ) ;
#30366 = ADVANCED_FACE ( 'NONE', ( #20413, #33399 ), #17415, .T. ) ;
#30367 = CARTESIAN_POINT ( 'NONE',  ( 143.0000000000000568, -175.8248315648716016, -46.05325008164006562 ) ) ;
#30368 = CARTESIAN_POINT ( 'NONE',  ( 0.000000000000000000, 3.524919873834583163E-15, 68.31122994652405112 ) ) ;
#30369 = CARTESIAN_POINT ( 'NONE',  ( 1.395000000000002238, -1.891117961019738836, -34.36292081097834483 ) ) ;
#30370 = VECTOR ( 'NONE', #5303, 1000.000000000000000 ) ;
#30371 = EDGE_CURVE ( 'NONE', #23862, #12566, #11703, .T. ) ;
#30372 = DIRECTION ( 'NONE',  ( -0.000000000000000000, -1.836970198721029688E-16, 1.000000000000000000 ) ) ;
#30373 = CARTESIAN_POINT ( 'NONE',  ( 2.261199740935803781, 7.012902549146583731, 32.64503617578046857 ) ) ;
#30374 = DIRECTION ( 'NONE',  ( 0.000000000000000000, 0.000000000000000000, 1.000000000000000000 ) ) ;
#30376 = CARTESIAN_POINT ( 'NONE',  ( -20.82057426567703473, -31.63141042832694083, 68.31122994652405112 ) ) ;
#30375 =( REPRESENTATION_RELATIONSHIP ('NONE','NONE', #23037, #28231 ) REPRESENTATION_RELATIONSHIP_WITH_TRANSFORMATION ( #28179 )SHAPE_REPRESENTATION_RELATIONSHIP( ) );
#30377 = CARTESIAN_POINT ( 'NONE',  ( 4.815661544189686616, -32.18716788982706589, 68.31122994652405112 ) ) ;
#30378 = ORIENTED_EDGE ( 'NONE', *, *, #2083, .T. ) ;
#30379 = EDGE_CURVE ( 'NONE', #7570, #23345, #14287, .T. ) ;
#30380 = LINE ( 'NONE', #30031, #32186 ) ;
#30381 = CARTESIAN_POINT ( 'NONE',  ( -8.300095185491707450E-14, -14.96425809614971669, -26.76330950827351174 ) ) ;
#30382 = CARTESIAN_POINT ( 'NONE',  ( 0.000000000000000000, 0.000000000000000000, 3.180000000000000160 ) ) ;
#30383 = ORIENTED_EDGE ( 'NONE', *, *, #10617, .F. ) ;
#30384 = AXIS2_PLACEMENT_3D ( 'NONE', #8426, #19300, #16994 ) ;
#30385 = EDGE_CURVE ( 'NONE', #23416, #726, #22734, .T. ) ;
#30386 = DIRECTION ( 'NONE',  ( -0.000000000000000000, -0.000000000000000000, -1.000000000000000000 ) ) ;
#30387 = ORIENTED_EDGE ( 'NONE', *, *, #6778, .T. ) ;
#30388 = CARTESIAN_POINT ( 'NONE',  ( 0.000000000000000000, 0.000000000000000000, 0.000000000000000000 ) ) ;
#30389 = AXIS2_PLACEMENT_3D ( 'NONE', #10229, #3392, #22799 ) ;
#30390 = DIRECTION ( 'NONE',  ( -0.000000000000000000, -0.000000000000000000, -1.000000000000000000 ) ) ;
#30391 = EDGE_CURVE ( 'NONE', #17657, #23884, #33932, .T. ) ;
#30392 = ADVANCED_FACE ( 'NONE', ( #22903 ), #8843, .F. ) ;
#30393 = CARTESIAN_POINT ( 'NONE',  ( 2.033589655458472034, -32.71412841873095090, 8.947071897914785410 ) ) ;
#30394 = VECTOR ( 'NONE', #17145, 999.9999999999998863 ) ;
#30395 = ORIENTED_EDGE ( 'NONE', *, *, #5280, .T. ) ;
#30396 = VECTOR ( 'NONE', #2715, 1000.000000000000000 ) ;
#30397 = CARTESIAN_POINT ( 'NONE',  ( 1.040000000000000924, 0.000000000000000000, 0.000000000000000000 ) ) ;
#30398 = DIRECTION ( 'NONE',  ( 0.000000000000000000, 1.000000000000000000, 0.000000000000000000 ) ) ;
#30399 = FACE_OUTER_BOUND ( 'NONE', #16904, .T. ) ;
#30400 = VERTEX_POINT ( 'NONE', #30910 ) ;
#30401 = DIRECTION ( 'NONE',  ( 2.631201909438060585E-14, -5.396010391056496978E-16, 1.000000000000000000 ) ) ;
#30402 = LINE ( 'NONE', #5998, #24397 ) ;
#30403 = VERTEX_POINT ( 'NONE', #17233 ) ;
#30404 = DIRECTION ( 'NONE',  ( 1.000000000000000000, 0.000000000000000000, -0.000000000000000000 ) ) ;
#30405 = CARTESIAN_POINT ( 'NONE',  ( 2.033589656346549202, -33.91140021655721881, 0.5303102773909653678 ) ) ;
#30406 = AXIS2_PLACEMENT_3D ( 'NONE', #6760, #25981, #14631 ) ;
#30407 = PLANE ( 'NONE',  #20169 ) ;
#30408 = CARTESIAN_POINT ( 'NONE',  ( 110.1903123430731881, -2.454113965193227997, 7.089506392665936296 ) ) ;
#30409 = ITEM_DEFINED_TRANSFORMATION ( 'NONE', 'NONE', #25760,  #28566 ) ;
#30410 = ORIENTED_EDGE ( 'NONE', *, *, #4044, .T. ) ;
#30411 = EDGE_LOOP ( 'NONE', ( #29444, #15473, #24501, #5007 ) ) ;
#30412 = VERTEX_POINT ( 'NONE', #3492 ) ;
#30413 = VECTOR ( 'NONE', #18310, 1000.000000000000000 ) ;
#30414 = CARTESIAN_POINT ( 'NONE',  ( 2.567399184519788768, -37.78162119159486565, 68.31122994652405112 ) ) ;
#30415 = AXIS2_PLACEMENT_3D ( 'NONE', #13537, #13707, #18884 ) ;
#30416 = PLANE ( 'NONE',  #25863 ) ;
#30417 = VECTOR ( 'NONE', #33406, 1000.000000000000000 ) ;
#30418 = ORIENTED_EDGE ( 'NONE', *, *, #1495, .F. ) ;
#30419 = ORIENTED_EDGE ( 'NONE', *, *, #32329, .T. ) ;
#30420 = CIRCLE ( 'NONE', #15090, 7.999999999999979572 ) ;
#30421 = DIRECTION ( 'NONE',  ( 0.000000000000000000, 0.000000000000000000, 1.000000000000000000 ) ) ;
#30422 = ORIENTED_EDGE ( 'NONE', *, *, #12367, .T. ) ;
#30423 = CLOSED_SHELL ( 'NONE', ( #1949, #32732, #28855, #8, #11522, #10353, #31982, #8443, #29564, #34081, #27303, #12789, #6867, #9728, #34812, #13385, #27671, #24533, #10530, #21419, #26981, #16377, #20813, #20426, #13070, #21248, #4241, #12887 ) ) ;
#30424 = DIRECTION ( 'NONE',  ( 8.433758354584418579E-81, -1.000000000000000000, -3.421138828918010427E-49 ) ) ;
#30425 = EDGE_CURVE ( 'NONE', #19968, #13940, #6156, .T. ) ;
#30426 = DIRECTION ( 'NONE',  ( -1.000000000000000000, 0.000000000000000000, -5.546364386991661285E-52 ) ) ;
#30427 = EDGE_LOOP ( 'NONE', ( #22592, #21406, #32056, #12212 ) ) ;
#30428 = EDGE_LOOP ( 'NONE', ( #29401, #17681, #25429, #24696 ) ) ;
#30429 = CARTESIAN_POINT ( 'NONE',  ( -414.0000000000000568, 124.9999999999999574, -187.0000000000000000 ) ) ;
#30430 = EDGE_CURVE ( 'NONE', #11323, #29274, #15076, .T. ) ;
#30431 = EDGE_CURVE ( 'NONE', #11988, #7322, #28062, .T. ) ;
#30432 = FACE_OUTER_BOUND ( 'NONE', #5092, .T. ) ;
#30433 = EDGE_LOOP ( 'NONE', ( #236, #2087, #26252, #6842 ) ) ;
#30434 = CARTESIAN_POINT ( 'NONE',  ( 28.23027531293552528, -17.65143121711728469, 20.00000000000000000 ) ) ;
#30435 = DIRECTION ( 'NONE',  ( 1.000000000000000000, 0.000000000000000000, 0.000000000000000000 ) ) ;
#30436 = CARTESIAN_POINT ( 'NONE',  ( -442.0000000000000000, -125.0000000000000000, 159.0000000000000000 ) ) ;
#30437 = DIRECTION ( 'NONE',  ( 0.000000000000000000, 0.000000000000000000, 1.000000000000000000 ) ) ;
#30438 = AXIS2_PLACEMENT_3D ( 'NONE', #19349, #14368, #8649 ) ;
#30439 = VECTOR ( 'NONE', #23212, 1000.000000000000000 ) ;
#30440 = LINE ( 'NONE', #14252, #8586 ) ;
#30441 = CARTESIAN_POINT ( 'NONE',  ( -5.491809612354312975, 32.07872192057775607, -36.68877005347593467 ) ) ;
#30442 = LINE ( 'NONE', #3377, #9204 ) ;
#30443 = AXIS2_PLACEMENT_3D ( 'NONE', #23083, #25917, #6851 ) ;
#30444 = EDGE_CURVE ( 'NONE', #17160, #23318, #25092, .T. ) ;
#30445 = ORIENTED_EDGE ( 'NONE', *, *, #25717, .T. ) ;
#30446 = CARTESIAN_POINT ( 'NONE',  ( 845.7351782833471816, 1080.372529058497548, 1753.598338701303419 ) ) ;
#30447 = VERTEX_POINT ( 'NONE', #14736 ) ;
#30448 = CIRCLE ( 'NONE', #16831, 9.999999999999998224 ) ;
#30450 = ORIENTED_EDGE ( 'NONE', *, *, #5438, .F. ) ;
#30449 = EDGE_CURVE ( 'NONE', #29651, #25284, #27811, .T. ) ;
#30451 = DIRECTION ( 'NONE',  ( 1.000000000000000000, 0.000000000000000000, 0.000000000000000000 ) ) ;
#30452 = EDGE_CURVE ( 'NONE', #9496, #28106, #12240, .T. ) ;
#30453 = EDGE_CURVE ( 'NONE', #22841, #28422, #23088, .T. ) ;
#30454 = CARTESIAN_POINT ( 'NONE',  ( -410.0000000000000568, -124.9999999999999858, -77.99999999999997158 ) ) ;
#30455 = APPLICATION_PROTOCOL_DEFINITION ( 'draft international standard', 'automotive_design', 1998, #11461 ) ;
#30456 = VERTEX_POINT ( 'NONE', #30564 ) ;
#30457 = CARTESIAN_POINT ( 'NONE',  ( 1.040000000000002034, 6.714005886384948774, 33.75364837705175347 ) ) ;
#30458 = CARTESIAN_POINT ( 'NONE',  ( -99.88497961182919482, -0.1683156175999579174, -12.50000000000000000 ) ) ;
#30459 = ITEM_DEFINED_TRANSFORMATION ( 'NONE', 'NONE', #9303,  #28566 ) ;
#30460 = AXIS2_PLACEMENT_3D ( 'NONE', #10228, #13607, #8081 ) ;
#30462 = LINE ( 'NONE', #3566, #10715 ) ;
#30461 = CARTESIAN_POINT ( 'NONE',  ( 1.394999999999999574, -18.21166265554809627, 29.20140402659733780 ) ) ;
#30463 = ORIENTED_EDGE ( 'NONE', *, *, #32484, .F. ) ;
#30464 = ORIENTED_EDGE ( 'NONE', *, *, #8484, .F. ) ;
#30465 = DIRECTION ( 'NONE',  ( 0.1617819965527614312, -0.9868265225415265851, 0.000000000000000000 ) ) ;
#30466 = DIRECTION ( 'NONE',  ( 0.000000000000000000, 0.000000000000000000, 1.000000000000000000 ) ) ;
#30467 = LINE ( 'NONE', #6060, #16568 ) ;
#30468 = CARTESIAN_POINT ( 'NONE',  ( -12.00000000000001066, -145.0000000000000000, -158.9999999999999716 ) ) ;
#30469 = VERTEX_POINT ( 'NONE', #25204 ) ;
#30470 = DIRECTION ( 'NONE',  ( -1.232595164407830946E-32, 0.000000000000000000, -1.000000000000000000 ) ) ;
#30471 = CYLINDRICAL_SURFACE ( 'NONE', #29351, 5.738084889453667792 ) ;
#30472 = CARTESIAN_POINT ( 'NONE',  ( -365.0000000000000000, 114.9999999999999716, 126.0000000000000000 ) ) ;
#30473 = ADVANCED_FACE ( 'NONE', ( #4190 ), #23932, .T. ) ;
#30474 = ADVANCED_FACE ( 'NONE', ( #4363 ), #4700, .T. ) ;
#30475 = ORIENTED_EDGE ( 'NONE', *, *, #9274, .T. ) ;
#30476 = CIRCLE ( 'NONE', #4897, 2.525000000000001243 ) ;
#30477 = CARTESIAN_POINT ( 'NONE',  ( 0.02407890056655738464, -11.07880054387200985, -29.04985141099774637 ) ) ;
#30478 = CARTESIAN_POINT ( 'NONE',  ( 0.000000000000000000, 3.524919873834583163E-15, 68.31122994652405112 ) ) ;
#30479 = EDGE_CURVE ( 'NONE', #13866, #7179, #5774, .T. ) ;
#30480 = CARTESIAN_POINT ( 'NONE',  ( -20.02113311122509032, -15.68591377522703390, -87.50000000000000000 ) ) ;
#30482 = CARTESIAN_POINT ( 'NONE',  ( 143.0000000000000568, -85.49999999999998579, 51.88904920397798293 ) ) ;
#30481 = CARTESIAN_POINT ( 'NONE',  ( -355.0000000000000000, 132.9999999999999716, 113.9999999999999858 ) ) ;
#30483 = VECTOR ( 'NONE', #23579, 1000.000000000000000 ) ;
#30484 = DIRECTION ( 'NONE',  ( 0.000000000000000000, 1.000000000000000000, 0.000000000000000000 ) ) ;
#30485 = ORIENTED_EDGE ( 'NONE', *, *, #17901, .T. ) ;
#30486 = CARTESIAN_POINT ( 'NONE',  ( -361.0000000000000000, -135.0000000000000000, 126.0000000000000000 ) ) ;
#30487 = DIRECTION ( 'NONE',  ( 0.000000000000000000, -6.123233995736766036E-17, -1.000000000000000000 ) ) ;
#30488 = AXIS2_PLACEMENT_3D ( 'NONE', #15724, #29583, #29045 ) ;
#30489 = EDGE_LOOP ( 'NONE', ( #18598, #14173, #9001, #32801, #19652, #24079, #24799, #7143 ) ) ;
#30490 =( NAMED_UNIT ( * ) PLANE_ANGLE_UNIT ( ) SI_UNIT ( $, .RADIAN. ) );
#30491 = VECTOR ( 'NONE', #14378, 1000.000000000000000 ) ;
#30492 = EDGE_LOOP ( 'NONE', ( #352, #11383, #17272, #9924 ) ) ;
#30493 = EDGE_CURVE ( 'NONE', #34152, #707, #30259, .T. ) ;
#30494 = ADVANCED_FACE ( 'NONE', ( #12574 ), #15423, .T. ) ;
#30495 = ORIENTED_EDGE ( 'NONE', *, *, #12208, .T. ) ;
#30496 = FACE_OUTER_BOUND ( 'NONE', #4876, .T. ) ;
#30497 = ORIENTED_EDGE ( 'NONE', *, *, #25953, .T. ) ;
#30498 = EDGE_LOOP ( 'NONE', ( #35071, #6591, #26060, #2482, #26866, #14524, #1265, #32720 ) ) ;
#30499 = DIRECTION ( 'NONE',  ( -1.000000000000000000, 0.000000000000000000, 0.000000000000000000 ) ) ;
#30500 = AXIS2_PLACEMENT_3D ( 'NONE', #24456, #16312, #21802 ) ;
#30501 = EDGE_CURVE ( 'NONE', #28175, #30403, #3231, .T. ) ;
#30502 = VERTEX_POINT ( 'NONE', #23418 ) ;
#30503 = FACE_OUTER_BOUND ( 'NONE', #24629, .T. ) ;
#30504 = DIRECTION ( 'NONE',  ( 0.9985334138511239299, -0.05413890858541763051, 0.000000000000000000 ) ) ;
#30505 = VERTEX_POINT ( 'NONE', #1872 ) ;
#30506 = ORIENTED_EDGE ( 'NONE', *, *, #26178, .T. ) ;
#30507 = CYLINDRICAL_SURFACE ( 'NONE', #34447, 7.500000000000000000 ) ;
#30508 = EDGE_CURVE ( 'NONE', #14034, #13474, #3528, .T. ) ;
#30509 = CARTESIAN_POINT ( 'NONE',  ( 0.000000000000000000, 10.87635688602997597, 87.50000000000000000 ) ) ;
#30510 = VECTOR ( 'NONE', #8927, 1000.000000000000000 ) ;
#30511 = CARTESIAN_POINT ( 'NONE',  ( 109.8644316410288013, -3.049149995829645299, -12.12344935835687920 ) ) ;
#30512 = CYLINDRICAL_SURFACE ( 'NONE', #25038, 7.999999999999979572 ) ;
#30513 = CARTESIAN_POINT ( 'NONE',  ( -418.0000000000000000, -105.0000000000000142, 104.0000000000000142 ) ) ;
#30514 = ORIENTED_EDGE ( 'NONE', *, *, #5891, .T. ) ;
#30515 = AXIS2_PLACEMENT_3D ( 'NONE', #5662, #13696, #16558 ) ;
#30516 = CARTESIAN_POINT ( 'NONE',  ( 1.749999999999999778, -33.26546734453812348, -8.820166447042147695 ) ) ;
#30517 = CARTESIAN_POINT ( 'NONE',  ( 0.000000000000000000, 0.000000000000000000, 0.000000000000000000 ) ) ;
#30518 = SHAPE_REPRESENTATION ( 'motor', ( #28566 ), #18940 ) ;
#30519 = ORIENTED_EDGE ( 'NONE', *, *, #26787, .F. ) ;
#30520 = DIRECTION ( 'NONE',  ( -0.000000000000000000, -0.000000000000000000, 1.000000000000000000 ) ) ;
#30521 = PLANE ( 'NONE',  #28568 ) ;
#30522 = CARTESIAN_POINT ( 'NONE',  ( -5.469264258321805627, 1.713938105891546382, 5.429999999999999716 ) ) ;
#30523 = CARTESIAN_POINT ( 'NONE',  ( 0.000000000000000000, 9.539392014169456147, -3.000000000000000000 ) ) ;
#30524 = SURFACE_SIDE_STYLE ('',( #19677 ) ) ;
#30525 = DIRECTION ( 'NONE',  ( 0.000000000000000000, 0.000000000000000000, -1.000000000000000000 ) ) ;
#30526 = VERTEX_POINT ( 'NONE', #18270 ) ;
#30527 = EDGE_CURVE ( 'NONE', #1722, #19525, #34098, .T. ) ;
#30528 = DIRECTION ( 'NONE',  ( 0.000000000000000000, 0.000000000000000000, -1.000000000000000000 ) ) ;
#30530 = DIRECTION ( 'NONE',  ( 0.000000000000000000, 0.000000000000000000, 1.000000000000000000 ) ) ;
#30529 = FACE_OUTER_BOUND ( 'NONE', #4942, .T. ) ;
#30531 = VERTEX_POINT ( 'NONE', #23771 ) ;
#30532 = PRODUCT_DEFINITION_SHAPE ( 'NONE', 'NONE',  #35098 ) ;
#30533 = CARTESIAN_POINT ( 'NONE',  ( -20.00000000000007461, 140.9999999999999716, -187.0000000000000000 ) ) ;
#30534 = CIRCLE ( 'NONE', #2676, 4.682234377621698584 ) ;
#30535 = EDGE_CURVE ( 'NONE', #18033, #34278, #22294, .T. ) ;
#30536 = ORIENTED_EDGE ( 'NONE', *, *, #5207, .F. ) ;
#30537 = ADVANCED_FACE ( 'NONE', ( #9892 ), #10243, .T. ) ;
#30538 = AXIS2_PLACEMENT_3D ( 'NONE', #30954, #13227, #10735 ) ;
#30539 = VECTOR ( 'NONE', #29948, 1000.000000000000000 ) ;
#30540 = EDGE_CURVE ( 'NONE', #19565, #26015, #26434, .T. ) ;
#30541 = VERTEX_POINT ( 'NONE', #31941 ) ;
#30542 = CARTESIAN_POINT ( 'NONE',  ( 101.2273074351206503, -4.338569679229816067, -6.125236864567445316 ) ) ;
#30543 = VERTEX_POINT ( 'NONE', #7736 ) ;
#30544 = ORIENTED_EDGE ( 'NONE', *, *, #24749, .T. ) ;
#30545 = DIRECTION ( 'NONE',  ( -1.000000000000000000, -0.000000000000000000, -0.000000000000000000 ) ) ;
#30547 = CARTESIAN_POINT ( 'NONE',  ( 11.99999999999999645, -145.0000000000000000, 190.9999999999999716 ) ) ;
#30546 = AXIS2_PLACEMENT_3D ( 'NONE', #28792, #15633, #2090 ) ;
#30548 = DIRECTION ( 'NONE',  ( 0.000000000000000000, 1.000000000000000000, 0.000000000000000000 ) ) ;
#30549 = DIRECTION ( 'NONE',  ( -0.000000000000000000, -0.000000000000000000, -1.000000000000000000 ) ) ;
#30550 = ORIENTED_EDGE ( 'NONE', *, *, #32480, .F. ) ;
#30551 = ORIENTED_EDGE ( 'NONE', *, *, #12907, .T. ) ;
#30552 = CARTESIAN_POINT ( 'NONE',  ( 145.0000000000000568, -87.50000000000000000, 65.00000000000000000 ) ) ;
#30554 = AXIS2_PLACEMENT_3D ( 'NONE', #33206, #17040, #8297 ) ;
#30553 = CARTESIAN_POINT ( 'NONE',  ( 2.765921099433441555, 11.80989368511502846, -28.76039115933972923 ) ) ;
#30555 = DIRECTION ( 'NONE',  ( 1.000000000000000000, 0.000000000000000000, 1.300283923313630633E-47 ) ) ;
#30556 = DIRECTION ( 'NONE',  ( 0.000000000000000000, 1.000000000000000000, 1.224646799147353207E-16 ) ) ;
#30557 = FACE_OUTER_BOUND ( 'NONE', #34102, .T. ) ;
#30558 = DIRECTION ( 'NONE',  ( 0.000000000000000000, 0.000000000000000000, -1.000000000000000000 ) ) ;
#30559 = VECTOR ( 'NONE', #25908, 1000.000000000000000 ) ;
#30560 = FACE_OUTER_BOUND ( 'NONE', #14081, .T. ) ;
#30561 = ORIENTED_EDGE ( 'NONE', *, *, #28660, .F. ) ;
#30562 = VECTOR ( 'NONE', #13083, 1000.000000000000000 ) ;
#30563 = CYLINDRICAL_SURFACE ( 'NONE', #16871, 4.000000000000003553 ) ;
#30564 = CARTESIAN_POINT ( 'NONE',  ( -18.38714294329533416, -33.09555747561019245, -36.68877005347593467 ) ) ;
#30565 = LINE ( 'NONE', #17056, #24000 ) ;
#30566 = EDGE_LOOP ( 'NONE', ( #9011, #18529, #19206, #13072, #22795, #12439, #3717, #5163 ) ) ;
#30567 = VECTOR ( 'NONE', #29591, 1000.000000000000000 ) ;
#30568 = CIRCLE ( 'NONE', #3843, 2.033421858999711507 ) ;
#30569 = LINE ( 'NONE', #8495, #7561 ) ;
#30570 = ORIENTED_EDGE ( 'NONE', *, *, #20487, .T. ) ;
#30571 = DIRECTION ( 'NONE',  ( -0.000000000000000000, -0.000000000000000000, -1.000000000000000000 ) ) ;
#30572 = FACE_OUTER_BOUND ( 'NONE', #34703, .T. ) ;
#30573 = ORIENTED_EDGE ( 'NONE', *, *, #10132, .T. ) ;
#30574 = FACE_OUTER_BOUND ( 'NONE', #12509, .T. ) ;
#30575 = CARTESIAN_POINT ( 'NONE',  ( 145.0000000000000568, 87.50000000000000000, 65.00000000000000000 ) ) ;
#30576 = FACE_OUTER_BOUND ( 'NONE', #24915, .T. ) ;
#30577 = EDGE_CURVE ( 'NONE', #3029, #18315, #7555, .T. ) ;
#30578 = ORIENTED_EDGE ( 'NONE', *, *, #15762, .T. ) ;
#30579 = EDGE_CURVE ( 'NONE', #26431, #18208, #9231, .T. ) ;
#30580 = VECTOR ( 'NONE', #31201, 1000.000000000000000 ) ;
#30581 = DIRECTION ( 'NONE',  ( 0.1063910735369155841, -0.9943243633099125844, -3.335902418025060287E-15 ) ) ;
#30582 = DIRECTION ( 'NONE',  ( 1.000000000000000000, 0.000000000000000000, 0.000000000000000000 ) ) ;
#30583 = EDGE_CURVE ( 'NONE', #6917, #12135, #4654, .T. ) ;
#30584 = EDGE_LOOP ( 'NONE', ( #8289, #34204, #16053, #18425 ) ) ;
#30585 = CYLINDRICAL_SURFACE ( 'NONE', #10437, 15.00000000000000000 ) ;
#30586 = CIRCLE ( 'NONE', #34543, 2.033421858999711951 ) ;
#30587 = CIRCLE ( 'NONE', #13513, 32.54542015209055705 ) ;
#30588 = DIRECTION ( 'NONE',  ( 0.000000000000000000, 1.131431318426415506E-52, 1.000000000000000000 ) ) ;
#30589 = CONTEXT_DEPENDENT_SHAPE_REPRESENTATION ( #1021, #18029 ) ;
#30590 = ORIENTED_EDGE ( 'NONE', *, *, #6534, .T. ) ;
#30592 = ORIENTED_EDGE ( 'NONE', *, *, #7941, .T. ) ;
#30591 =( REPRESENTATION_RELATIONSHIP ('NONE','NONE', #23037, #15767 ) REPRESENTATION_RELATIONSHIP_WITH_TRANSFORMATION ( #24352 )SHAPE_REPRESENTATION_RELATIONSHIP( ) );
#30593 = ORIENTED_EDGE ( 'NONE', *, *, #15719, .F. ) ;
#30594 = EDGE_CURVE ( 'NONE', #22581, #29789, #28934, .T. ) ;
#30595 = CARTESIAN_POINT ( 'NONE',  ( -365.0000000000000000, -135.0000000000000000, 113.9999999999999858 ) ) ;
#30596 = AXIS2_PLACEMENT_3D ( 'NONE', #26729, #24402, #2342 ) ;
#30597 = CARTESIAN_POINT ( 'NONE',  ( 2.789999999999999147, 17.98401995359667893, -24.59729088254936613 ) ) ;
#30598 = CARTESIAN_POINT ( 'NONE',  ( 0.000000000000000000, 14.59907093257252164, -26.74544485249453274 ) ) ;
#30599 = ORIENTED_EDGE ( 'NONE', *, *, #6264, .F. ) ;
#30600 = VERTEX_POINT ( 'NONE', #21278 ) ;
#30601 = CARTESIAN_POINT ( 'NONE',  ( 0.000000000000000000, 2.005524111408653720, -31.87689292423236154 ) ) ;
#30602 = VERTEX_POINT ( 'NONE', #18624 ) ;
#30603 = CARTESIAN_POINT ( 'NONE',  ( -20.00000000000007461, -113.0000000000000000, -159.0000000000000000 ) ) ;
#30604 = DIRECTION ( 'NONE',  ( -1.000000000000000000, -0.000000000000000000, -0.000000000000000000 ) ) ;
#30605 = VERTEX_POINT ( 'NONE', #29466 ) ;
#30606 = ORIENTED_EDGE ( 'NONE', *, *, #20256, .F. ) ;
#30607 = DIRECTION ( 'NONE',  ( 1.000000000000000000, 0.000000000000000000, -1.848892746611746966E-32 ) ) ;
#30608 = AXIS2_PLACEMENT_3D ( 'NONE', #28662, #32020, #6934 ) ;
#30609 = CARTESIAN_POINT ( 'NONE',  ( -499.9999999999999432, 108.9999999999999858, 162.9999999999999716 ) ) ;
#30610 = ORIENTED_EDGE ( 'NONE', *, *, #28085, .F. ) ;
#30611 = CARTESIAN_POINT ( 'NONE',  ( -500.0000000000000000, -141.0000000000000000, 162.9999999999999716 ) ) ;
#30612 = PLANE ( 'NONE',  #24631 ) ;
#30613 = DIRECTION ( 'NONE',  ( -6.189473249308364160E-17, 0.000000000000000000, 1.000000000000000000 ) ) ;
#30614 = AXIS2_PLACEMENT_3D ( 'NONE', #33639, #25450, #19606 ) ;
#30615 = VECTOR ( 'NONE', #1432, 1000.000000000000000 ) ;
#30616 = PLANE ( 'NONE',  #6875 ) ;
#30617 = CARTESIAN_POINT ( 'NONE',  ( 2.033800789375341367, 31.72496621377067427, -11.99023130257920045 ) ) ;
#30618 = PRESENTATION_STYLE_ASSIGNMENT (( #717 ) ) ;
#30619 = EDGE_CURVE ( 'NONE', #8440, #32621, #33367, .T. ) ;
#30620 = ORIENTED_EDGE ( 'NONE', *, *, #20683, .T. ) ;
#30621 = CIRCLE ( 'NONE', #29478, 3.999999999999976019 ) ;
#30622 = VERTEX_POINT ( 'NONE', #26784 ) ;
#30623 = DIRECTION ( 'NONE',  ( 2.631201909438060269E-14, -5.396010391056495992E-16, 0.9999999999999998890 ) ) ;
#30624 = EDGE_CURVE ( 'NONE', #27262, #18752, #30829, .T. ) ;
#30625 = ORIENTED_EDGE ( 'NONE', *, *, #30391, .F. ) ;
#30626 = ORIENTED_EDGE ( 'NONE', *, *, #29780, .F. ) ;
#30627 = ADVANCED_FACE ( 'NONE', ( #24279 ), #5938, .F. ) ;
#30628 = CARTESIAN_POINT ( 'NONE',  ( -441.9999999999999432, -105.0000000000000142, 139.9999999999999716 ) ) ;
#30629 = VECTOR ( 'NONE', #6683, 1000.000000000000000 ) ;
#30630 = EDGE_CURVE ( 'NONE', #29298, #24529, #29813, .T. ) ;
#30631 = DIRECTION ( 'NONE',  ( -0.000000000000000000, 0.000000000000000000, -1.000000000000000000 ) ) ;
#30632 = EDGE_CURVE ( 'NONE', #19421, #31298, #15100, .T. ) ;
#30633 = VERTEX_POINT ( 'NONE', #22156 ) ;
#30634 = DIRECTION ( 'NONE',  ( 0.000000000000000000, 0.000000000000000000, -1.000000000000000000 ) ) ;
#30635 = DIRECTION ( 'NONE',  ( -0.000000000000000000, -0.000000000000000000, 1.000000000000000000 ) ) ;
#30636 = EDGE_CURVE ( 'NONE', #18981, #24353, #27302, .T. ) ;
#30637 = MECHANICAL_DESIGN_GEOMETRIC_PRESENTATION_REPRESENTATION (  '', ( #15869 ), #2752 ) ;
#30639 = DIRECTION ( 'NONE',  ( -0.000000000000000000, 0.8486862100397269959, 0.5288966977476833309 ) ) ;
#30638 = CARTESIAN_POINT ( 'NONE',  ( -418.0000000000000568, 105.0000000000000142, 159.0000000000000000 ) ) ;
#30640 = ORIENTED_EDGE ( 'NONE', *, *, #565, .T. ) ;
#30641 = VERTEX_POINT ( 'NONE', #24811 ) ;
#30642 = CARTESIAN_POINT ( 'NONE',  ( -37.12776225901827587, -7.411627343331159246, -15.81122994652406355 ) ) ;
#30643 = DIRECTION ( 'NONE',  ( 0.9985334138511240409, -0.05413890858541543089, -9.945156166269024927E-18 ) ) ;
#30645 = EDGE_CURVE ( 'NONE', #4681, #14225, #11130, .T. ) ;
#30644 = LINE ( 'NONE', #22279, #9733 ) ;
#30646 = LINE ( 'NONE', #11253, #9300 ) ;
#30647 = VERTEX_POINT ( 'NONE', #18792 ) ;
#30648 = AXIS2_PLACEMENT_3D ( 'NONE', #26301, #28798, #1741 ) ;
#30649 = CARTESIAN_POINT ( 'NONE',  ( -32.54223829851967764, 0.4550817492056254410, -15.81122994652406355 ) ) ;
#30650 = DIRECTION ( 'NONE',  ( 0.000000000000000000, 0.08715574274765885976, 0.9961946980917454342 ) ) ;
#30651 = CARTESIAN_POINT ( 'NONE',  ( 1.205771365940041528, 7.794228634059941818, 13.49999999999999645 ) ) ;
#30652 = ORIENTED_EDGE ( 'NONE', *, *, #10574, .F. ) ;
#30653 = DIRECTION ( 'NONE',  ( 0.000000000000000000, 0.000000000000000000, 1.000000000000000000 ) ) ;
#30654 = DIRECTION ( 'NONE',  ( -1.000000000000000000, -0.000000000000000000, 0.000000000000000000 ) ) ;
#30655 = CARTESIAN_POINT ( 'NONE',  ( 1.040000000000002034, 34.17636915695680244, 4.045051921974835096 ) ) ;
#30657 = CARTESIAN_POINT ( 'NONE',  ( 60.00000000000000000, -33.69708579775584667, 49.43553178847298568 ) ) ;
#30656 = DIRECTION ( 'NONE',  ( 0.000000000000000000, 6.123233995736766036E-17, 1.000000000000000000 ) ) ;
#30658 = AXIS2_PLACEMENT_3D ( 'NONE', #18437, #16116, #18100 ) ;
#30659 = UNCERTAINTY_MEASURE_WITH_UNIT (LENGTH_MEASURE( 1.000000000000000082E-05 ), #18957, 'distance_accuracy_value', 'NONE');
#30660 = CARTESIAN_POINT ( 'NONE',  ( -15.99999999999998579, 144.9999999999999716, 187.0000000000000000 ) ) ;
#30661 = ORIENTED_EDGE ( 'NONE', *, *, #32618, .F. ) ;
#30662 = CARTESIAN_POINT ( 'NONE',  ( -430.0000000000000000, -119.0000000000000000, 109.9999999999999858 ) ) ;
#30663 = FACE_OUTER_BOUND ( 'NONE', #15939, .T. ) ;
#30664 = VECTOR ( 'NONE', #34836, 1000.000000000000000 ) ;
#30665 = ORIENTED_EDGE ( 'NONE', *, *, #16552, .T. ) ;
#30666 = ORIENTED_EDGE ( 'NONE', *, *, #10922, .F. ) ;
#30667 = AXIS2_PLACEMENT_3D ( 'NONE', #8266, #21620, #7915 ) ;
#30668 = EDGE_CURVE ( 'NONE', #8703, #28747, #20639, .T. ) ;
#30669 = EDGE_CURVE ( 'NONE', #10216, #34042, #24448, .T. ) ;
#30670 = ORIENTED_EDGE ( 'NONE', *, *, #15478, .T. ) ;
#30671 = DIRECTION ( 'NONE',  ( 1.000000000000000000, 0.000000000000000000, -1.232595164407831220E-32 ) ) ;
#30672 = ORIENTED_EDGE ( 'NONE', *, *, #16978, .F. ) ;
#30673 = ORIENTED_EDGE ( 'NONE', *, *, #7697, .T. ) ;
#30674 = CARTESIAN_POINT ( 'NONE',  ( 0.000000000000000000, 0.000000000000000000, 8.000000000000000000 ) ) ;
#30675 = CIRCLE ( 'NONE', #27266, 2.524999999999999467 ) ;
#30676 = EDGE_LOOP ( 'NONE', ( #17108, #7409, #14060, #8511 ) ) ;
#30677 = CARTESIAN_POINT ( 'NONE',  ( -37.85301660235036536, 0.7430237821112573027, 68.31122994652405112 ) ) ;
#30678 = CARTESIAN_POINT ( 'NONE',  ( -20.00000000000007461, 136.9999999999999432, 194.9999999999999716 ) ) ;
#30679 = ORIENTED_EDGE ( 'NONE', *, *, #24004, .T. ) ;
#30680 = ORIENTED_EDGE ( 'NONE', *, *, #9237, .T. ) ;
#30681 = DIRECTION ( 'NONE',  ( 0.000000000000000000, 1.000000000000000000, -1.131431318426415506E-52 ) ) ;
#30682 = CARTESIAN_POINT ( 'NONE',  ( -441.9999999999999432, -105.0000000000000142, -69.99999999999998579 ) ) ;
#30683 = CARTESIAN_POINT ( 'NONE',  ( -145.0000000000000568, -90.42893218813456713, 44.81798139211241505 ) ) ;
#30685 = ADVANCED_FACE ( 'NONE', ( #29988, #11303 ), #10945, .F. ) ;
#30684 = DIRECTION ( 'NONE',  ( -0.000000000000000000, -0.000000000000000000, -1.000000000000000000 ) ) ;
#30686 = LINE ( 'NONE', #6276, #8594 ) ;
#30687 = ORIENTED_EDGE ( 'NONE', *, *, #28029, .F. ) ;
#30688 = LINE ( 'NONE', #6461, #17413 ) ;
#30689 = CARTESIAN_POINT ( 'NONE',  ( 143.0000000000000568, -87.50000000000000000, 65.00000000000000000 ) ) ;
#30690 = ORIENTED_EDGE ( 'NONE', *, *, #2134, .F. ) ;
#30691 = PRODUCT_DEFINITION_SHAPE ( 'NONE', 'NONE',  #35227 ) ;
#30692 = DIRECTION ( 'NONE',  ( -1.000000000000000000, -0.000000000000000000, -0.000000000000000000 ) ) ;
#30694 = EDGE_CURVE ( 'NONE', #34864, #17236, #16126, .T. ) ;
#30693 = CARTESIAN_POINT ( 'NONE',  ( 0.000000000000000000, 0.000000000000000000, 0.000000000000000000 ) ) ;
#30695 = LINE ( 'NONE', #34058, #9851 ) ;
#30696 = VECTOR ( 'NONE', #12191, 1000.000000000000114 ) ;
#30697 = EDGE_CURVE ( 'NONE', #750, #14972, #24625, .T. ) ;
#30698 = CARTESIAN_POINT ( 'NONE',  ( 99.30309277135016544, 0.7888478034546075879, -7.468363897292212172 ) ) ;
#30699 = DIRECTION ( 'NONE',  ( -1.000000000000000000, 0.000000000000000000, 0.000000000000000000 ) ) ;
#30700 = EDGE_CURVE ( 'NONE', #28220, #14210, #30334, .T. ) ;
#30701 = FACE_OUTER_BOUND ( 'NONE', #19915, .T. ) ;
#30702 = ORIENTED_EDGE ( 'NONE', *, *, #20074, .F. ) ;
#30703 = LINE ( 'NONE', #1503, #19585 ) ;
#30705 = CARTESIAN_POINT ( 'NONE',  ( 2.783128833706969729, 11.66139262930099640, -28.58215465626852136 ) ) ;
#30704 = CARTESIAN_POINT ( 'NONE',  ( -20.02113311122509032, -11.61907005722761177, -87.50000000000000000 ) ) ;
#30706 = ADVANCED_FACE ( 'NONE', ( #21451 ), #8448, .F. ) ;
#30707 = ORIENTED_EDGE ( 'NONE', *, *, #7167, .F. ) ;
#30708 = CARTESIAN_POINT ( 'NONE',  ( -10.00000000000000000, 0.000000000000000000, 0.000000000000000000 ) ) ;
#30709 = DIRECTION ( 'NONE',  ( -1.000000000000000000, 0.000000000000000000, 0.000000000000000000 ) ) ;
#30710 = ORIENTED_EDGE ( 'NONE', *, *, #6575, .T. ) ;
#30711 = ORIENTED_EDGE ( 'NONE', *, *, #29365, .T. ) ;
#30712 = VERTEX_POINT ( 'NONE', #16477 ) ;
#30713 = CARTESIAN_POINT ( 'NONE',  ( 100.7124613249971503, -3.830588487554197119, -6.455099174110775273 ) ) ;
#30714 = VERTEX_POINT ( 'NONE', #10604 ) ;
#30715 = VERTEX_POINT ( 'NONE', #13447 ) ;
#30716 = PLANE ( 'NONE',  #12189 ) ;
#30717 = VECTOR ( 'NONE', #33993, 1000.000000000000000 ) ;
#30718 = CARTESIAN_POINT ( 'NONE',  ( 10.00000000000000000, -7.794228634059966687, -13.49999999999999822 ) ) ;
#30719 = CARTESIAN_POINT ( 'NONE',  ( 145.0000000000000568, -78.33668825982579165, -75.00000000000001421 ) ) ;
#30720 = CARTESIAN_POINT ( 'NONE',  ( 1.991296462759137853, -32.48444414290483451, 68.31122994652405112 ) ) ;
#30721 = ORIENTED_EDGE ( 'NONE', *, *, #31833, .T. ) ;
#30722 = VERTEX_POINT ( 'NONE', #30152 ) ;
#30723 = CARTESIAN_POINT ( 'NONE',  ( 0.006892394228582813739, 29.25821015115251811, 9.843862221888281638 ) ) ;
#30724 = DIRECTION ( 'NONE',  ( 3.040835319149746090E-31, 1.000000000000000000, -3.748118910144520367E-63 ) ) ;
#30725 = DIRECTION ( 'NONE',  ( -1.000000000000000000, 6.792721752314501023E-48, -3.697785493223492838E-32 ) ) ;
#30726 = DIRECTION ( 'NONE',  ( 1.000000000000000000, -0.000000000000000000, -0.000000000000000000 ) ) ;
#30727 = LINE ( 'NONE', #14729, #11398 ) ;
#30728 = DIRECTION ( 'NONE',  ( 0.000000000000000000, -1.000000000000000000, -5.053935297177146739E-49 ) ) ;
#30729 = FACE_OUTER_BOUND ( 'NONE', #30073, .T. ) ;
#30730 = VERTEX_POINT ( 'NONE', #16655 ) ;
#30731 = CARTESIAN_POINT ( 'NONE',  ( 19.99999999999998934, 4.559999999999909015, 177.7400000000000091 ) ) ;
#30732 = CARTESIAN_POINT ( 'NONE',  ( 0.5248942696725308332, 30.74170660486493389, -13.00608379084241939 ) ) ;
#30733 = ADVANCED_FACE ( 'NONE', ( #3277 ), #24106, .F. ) ;
#30734 = CYLINDRICAL_SURFACE ( 'NONE', #5831, 2.524999999999999467 ) ;
#30735 = ORIENTED_EDGE ( 'NONE', *, *, #9731, .T. ) ;
#30736 = ADVANCED_FACE ( 'NONE', ( #790 ), #17014, .F. ) ;
#30737 = CARTESIAN_POINT ( 'NONE',  ( -442.0000000000000000, -125.0000000000000000, 162.9999999999999716 ) ) ;
#30738 = ORIENTED_EDGE ( 'NONE', *, *, #33182, .T. ) ;
#30739 = CONICAL_SURFACE ( 'NONE', #7421, 6.898500000000000298, 0.7853981633974428389 ) ;
#30740 = SURFACE_STYLE_USAGE ( .BOTH. , #9028 ) ;
#30741 = CARTESIAN_POINT ( 'NONE',  ( -99.88497961182919482, 6.264093345946821604E-16, 12.50000000000000000 ) ) ;
#30742 = AXIS2_PLACEMENT_3D ( 'NONE', #19344, #30184, #5259 ) ;
#30743 = ORIENTED_EDGE ( 'NONE', *, *, #7938, .T. ) ;
#30744 = DIRECTION ( 'NONE',  ( 0.000000000000000000, 0.000000000000000000, -1.000000000000000000 ) ) ;
#30745 = DIRECTION ( 'NONE',  ( -0.3193015301359797276, 0.9476531711828024562, -0.000000000000000000 ) ) ;
#30746 = CARTESIAN_POINT ( 'NONE',  ( -365.0000000000000000, -135.0000000000000000, 113.9999999999999858 ) ) ;
#30747 = ORIENTED_EDGE ( 'NONE', *, *, #2567, .F. ) ;
#30748 = AXIS2_PLACEMENT_3D ( 'NONE', #26908, #27086, #21044 ) ;
#30749 = DIRECTION ( 'NONE',  ( 2.631201909438060585E-14, -5.396010391056496978E-16, 1.000000000000000000 ) ) ;
#30750 = CIRCLE ( 'NONE', #13128, 7.999999999999979572 ) ;
#30751 = CARTESIAN_POINT ( 'NONE',  ( -29.72561944762171393, -13.25111019240557475, -36.68877005347593467 ) ) ;
#30752 = ORIENTED_EDGE ( 'NONE', *, *, #3088, .F. ) ;
#30753 = DIRECTION ( 'NONE',  ( 0.000000000000000000, 1.000000000000000000, 0.000000000000000000 ) ) ;
#30754 = CARTESIAN_POINT ( 'NONE',  ( 2.789819856565905809, -25.83993731729781373, -16.24881338200996694 ) ) ;
#30755 = DIRECTION ( 'NONE',  ( 0.000000000000000000, -1.000000000000000000, -1.224646799147353207E-16 ) ) ;
#30756 = CARTESIAN_POINT ( 'NONE',  ( -365.0000000000000000, -125.0000000000000284, 168.9999999999999716 ) ) ;
#30757 = ORIENTED_EDGE ( 'NONE', *, *, #29893, .F. ) ;
#30758 = VERTEX_POINT ( 'NONE', #11479 ) ;
#30759 = ORIENTED_EDGE ( 'NONE', *, *, #30697, .T. ) ;
#30760 = AXIS2_PLACEMENT_3D ( 'NONE', #17007, #14853, #22323 ) ;
#30761 =( NAMED_UNIT ( * ) SI_UNIT ( $, .STERADIAN. ) SOLID_ANGLE_UNIT ( ) );
#30763 = CIRCLE ( 'NONE', #31859, 1.999999999999999556 ) ;
#30762 = PLANE ( 'NONE',  #32476 ) ;
#30764 = CYLINDRICAL_SURFACE ( 'NONE', #23573, 2.000000000000001776 ) ;
#30765 = CARTESIAN_POINT ( 'NONE',  ( -8.501468252432740527E-14, 14.57875922523702705, -26.97523840778871573 ) ) ;
#30766 = ORIENTED_EDGE ( 'NONE', *, *, #2391, .T. ) ;
#30767 = VERTEX_POINT ( 'NONE', #14862 ) ;
#30768 = CARTESIAN_POINT ( 'NONE',  ( 2.765921099433442887, -30.46391896562411716, 6.211548095912460710 ) ) ;
#30769 = DIRECTION ( 'NONE',  ( 0.000000000000000000, 0.000000000000000000, 1.000000000000000000 ) ) ;
#30770 = VERTEX_POINT ( 'NONE', #33176 ) ;
#30771 = PRODUCT_DEFINITION_SHAPE ( 'NONE', 'NONE',  #35179 ) ;
#30772 = ADVANCED_FACE ( 'NONE', ( #27838 ), #28019, .F. ) ;
#30773 = CARTESIAN_POINT ( 'NONE',  ( 2.765921099433442443, 30.61125888652969707, -5.439165181698684570 ) ) ;
#30774 = CARTESIAN_POINT ( 'NONE',  ( 2.789999999999999147, -14.75935258146392570, -26.65732927035534772 ) ) ;
#30775 = ORIENTED_EDGE ( 'NONE', *, *, #31504, .T. ) ;
#30776 = VERTEX_POINT ( 'NONE', #25517 ) ;
#30777 = EDGE_CURVE ( 'NONE', #34034, #32903, #33667, .T. ) ;
#30778 = VECTOR ( 'NONE', #12315, 1000.000000000000000 ) ;
#30779 = AXIS2_PLACEMENT_3D ( 'NONE', #12289, #18161, #33980 ) ;
#30781 = AXIS2_PLACEMENT_3D ( 'NONE', #14353, #25176, #5769 ) ;
#30780 = DIRECTION ( 'NONE',  ( -1.000000000000000000, -3.040835319149746528E-31, -1.232595164407830946E-32 ) ) ;
#30782 = EDGE_LOOP ( 'NONE', ( #31966, #19180, #29183, #24842 ) ) ;
#30783 = EDGE_CURVE ( 'NONE', #24367, #16094, #12194, .T. ) ;
#30784 = VECTOR ( 'NONE', #16973, 1000.000000000000000 ) ;
#30785 = CARTESIAN_POINT ( 'NONE',  ( 2.783128948542799908, -11.06504178053264198, -28.81826507853140740 ) ) ;
#30786 = CARTESIAN_POINT ( 'NONE',  ( -9.410814080250917257, 36.67205378194066867, -36.68877005347593467 ) ) ;
#30787 = DIRECTION ( 'NONE',  ( 0.000000000000000000, 1.000000000000000000, 5.053935297177146739E-49 ) ) ;
#30788 = CARTESIAN_POINT ( 'NONE',  ( -99.91951324175876437, -0.6815953102691991727, 12.48576125250277968 ) ) ;
#30789 = CARTESIAN_POINT ( 'NONE',  ( 2.790000000000000924, 0.000000000000000000, 10.00000000000000000 ) ) ;
#30790 = DIRECTION ( 'NONE',  ( 0.000000000000000000, 1.000000000000000000, 1.224646799147353207E-16 ) ) ;
#30791 = ORIENTED_EDGE ( 'NONE', *, *, #1926, .F. ) ;
#30792 = AXIS2_PLACEMENT_3D ( 'NONE', #9588, #25417, #22761 ) ;
#30793 = VERTEX_POINT ( 'NONE', #28378 ) ;
#30794 = CARTESIAN_POINT ( 'NONE',  ( 833.2874294586813448, 1196.708416208197832, 1753.598338701303419 ) ) ;
#30795 =( REPRESENTATION_RELATIONSHIP ('NONE','NONE', #23037, #15767 ) REPRESENTATION_RELATIONSHIP_WITH_TRANSFORMATION ( #15629 )SHAPE_REPRESENTATION_RELATIONSHIP( ) );
#30796 = ORIENTED_EDGE ( 'NONE', *, *, #33045, .T. ) ;
#30797 = ORIENTED_EDGE ( 'NONE', *, *, #29449, .T. ) ;
#30798 = AXIS2_PLACEMENT_3D ( 'NONE', #32880, #142, #27366 ) ;
#30799 = DIRECTION ( 'NONE',  ( 1.000000000000000000, 0.000000000000000000, 5.546364386991661285E-52 ) ) ;
#30800 = VECTOR ( 'NONE', #14379, 1000.000000000000000 ) ;
#30801 = FACE_OUTER_BOUND ( 'NONE', #21765, .T. ) ;
#30802 = ITEM_DEFINED_TRANSFORMATION ( 'NONE', 'NONE', #15509,  #28566 ) ;
#30803 = CIRCLE ( 'NONE', #15470, 34.41491905851385269 ) ;
#30804 = ORIENTED_EDGE ( 'NONE', *, *, #19861, .T. ) ;
#30805 = VECTOR ( 'NONE', #7416, 1000.000000000000227 ) ;
#30806 = TOROIDAL_SURFACE ( 'NONE', #17186, 30.47050528711511674, 8.000000000000000000 ) ;
#30807 = CARTESIAN_POINT ( 'NONE',  ( 0.000000000000000000, 3.524919873834583163E-15, 68.31122994652405112 ) ) ;
#30808 = CARTESIAN_POINT ( 'NONE',  ( -107.2761209656274417, -4.592825538643426242, -11.62648616087116160 ) ) ;
#30810 = FACE_OUTER_BOUND ( 'NONE', #10144, .T. ) ;
#30809 = DIRECTION ( 'NONE',  ( -1.000000000000000000, 0.000000000000000000, 0.000000000000000000 ) ) ;
#30811 = ORIENTED_EDGE ( 'NONE', *, *, #13779, .F. ) ;
#30812 = VERTEX_POINT ( 'NONE', #3622 ) ;
#30813 = LINE ( 'NONE', #31168, #31618 ) ;
#30814 = EDGE_CURVE ( 'NONE', #7154, #21502, #31382, .T. ) ;
#30815 = CYLINDRICAL_SURFACE ( 'NONE', #15341, 16.19999999999999574 ) ;
#30816 = CARTESIAN_POINT ( 'NONE',  ( -500.0000000000000000, -105.0000000000000142, 162.9999999999999716 ) ) ;
#30817 = DIRECTION ( 'NONE',  ( 0.000000000000000000, 0.000000000000000000, 1.000000000000000000 ) ) ;
#30818 = ORIENTED_EDGE ( 'NONE', *, *, #18724, .F. ) ;
#30819 = CARTESIAN_POINT ( 'NONE',  ( 1.039999999999999813, -24.90160365674851661, -23.75493189058366994 ) ) ;
#30820 = CARTESIAN_POINT ( 'NONE',  ( -6.500000000000000000, 0.000000000000000000, -0.7520000000000001128 ) ) ;
#30821 = PRODUCT_DEFINITION_SHAPE ( 'NONE', 'NONE',  #35102 ) ;
#30822 = VERTEX_POINT ( 'NONE', #22694 ) ;
#30823 = EDGE_CURVE ( 'NONE', #6516, #10776, #3969, .T. ) ;
#30824 = CARTESIAN_POINT ( 'NONE',  ( -8.000000000000000000, 0.000000000000000000, 0.000000000000000000 ) ) ;
#30825 = FACE_BOUND ( 'NONE', #4893, .T. ) ;
#30826 = DIRECTION ( 'NONE',  ( -0.9289767198167914186, 0.3701381553399144542, 0.000000000000000000 ) ) ;
#30828 = CARTESIAN_POINT ( 'NONE',  ( 105.0000000000000000, 0.000000000000000000, 60.00000000000000000 ) ) ;
#30827 = CARTESIAN_POINT ( 'NONE',  ( 0.7564103436534542757, -33.91140021655721881, -0.5303102773914404322 ) ) ;
#30829 = CIRCLE ( 'NONE', #6925, 15.00000000000000000 ) ;
#30830 = EDGE_CURVE ( 'NONE', #28173, #10186, #31048, .T. ) ;
#30831 = VECTOR ( 'NONE', #31813, 1000.000000000000000 ) ;
#30832 = DIRECTION ( 'NONE',  ( 1.000000000000000000, -3.540705920434608777E-32, 2.891205793294675368E-16 ) ) ;
#30833 = CARTESIAN_POINT ( 'NONE',  ( 1.039999999999999147, -24.90160365674884346, 23.75493189058332177 ) ) ;
#30834 = ORIENTED_EDGE ( 'NONE', *, *, #13303, .T. ) ;
#30835 = CARTESIAN_POINT ( 'NONE',  ( 0.000000000000000000, 11.30192140231230091, 28.29696565125076191 ) ) ;
#30836 = EDGE_CURVE ( 'NONE', #26849, #5629, #2336, .T. ) ;
#30837 = VERTEX_POINT ( 'NONE', #17371 ) ;
#30838 = SHAPE_REPRESENTATION_RELATIONSHIP ( 'NONE' , 'NONE' ,  #11185, #32214 ) ;
#30839 = EDGE_LOOP ( 'NONE', ( #1734, #15661, #6963, #26895 ) ) ;
#30840 = EDGE_LOOP ( 'NONE', ( #27593, #29964, #7567, #13395, #9312, #17345 ) ) ;
#30841 = CARTESIAN_POINT ( 'NONE',  ( 11.99999999999999645, -145.0000000000000000, -158.9999999999999716 ) ) ;
#30842 = VERTEX_POINT ( 'NONE', #8798 ) ;
#30843 = VERTEX_POINT ( 'NONE', #615 ) ;
#30844 = FACE_OUTER_BOUND ( 'NONE', #23234, .T. ) ;
#30845 = CONTEXT_DEPENDENT_SHAPE_REPRESENTATION ( #13341, #2098 ) ;
#30846 = ORIENTED_EDGE ( 'NONE', *, *, #17876, .F. ) ;
#30847 = DIRECTION ( 'NONE',  ( 0.4198891015602640997, 0.9075754196709572286, 0.000000000000000000 ) ) ;
#30848 = VECTOR ( 'NONE', #22423, 1000.000000000000000 ) ;
#30849 = CARTESIAN_POINT ( 'NONE',  ( 0.006871193125022706863, 29.25797949657101782, -9.843693408253376020 ) ) ;
#30850 = VERTEX_POINT ( 'NONE', #25339 ) ;
#30851 = EDGE_LOOP ( 'NONE', ( #16724, #27285, #29109, #23527 ) ) ;
#30852 = VECTOR ( 'NONE', #31095, 1000.000000000000000 ) ;
#30853 = DIRECTION ( 'NONE',  ( 0.000000000000000000, 1.000000000000000000, 1.224646799147353207E-16 ) ) ;
#30854 = LINE ( 'NONE', #16830, #23756 ) ;
#30855 = DIRECTION ( 'NONE',  ( 1.000000000000000000, 0.000000000000000000, 0.000000000000000000 ) ) ;
#30856 = CARTESIAN_POINT ( 'NONE',  ( 0.000000000000000000, -32.54542015209057126, 76.74945698428001606 ) ) ;
#30857 = CARTESIAN_POINT ( 'NONE',  ( 21.17270648470164218, -7.613573412837960852, 0.000000000000000000 ) ) ;
#30858 = ORIENTED_EDGE ( 'NONE', *, *, #20017, .T. ) ;
#30859 = DIRECTION ( 'NONE',  ( -1.848892746611746419E-32, -6.842277657836020854E-49, 1.000000000000000000 ) ) ;
#30860 = DIRECTION ( 'NONE',  ( 1.300283923313630633E-47, 0.000000000000000000, -1.000000000000000000 ) ) ;
#30861 = ORIENTED_EDGE ( 'NONE', *, *, #30932, .F. ) ;
#30862 = CARTESIAN_POINT ( 'NONE',  ( 0.000000000000000000, 11.69134295108991495, 6.750000000000012434 ) ) ;
#30863 = DIRECTION ( 'NONE',  ( 0.000000000000000000, 1.836970198721029441E-16, -1.000000000000000000 ) ) ;
#30864 = DIRECTION ( 'NONE',  ( 0.8276889981568904542, 0.5611870653623824978, -0.000000000000000000 ) ) ;
#30865 = EDGE_CURVE ( 'NONE', #984, #25727, #975, .T. ) ;
#30866 = CARTESIAN_POINT ( 'NONE',  ( -441.9999999999999432, 105.0000000000000142, 190.9999999999999716 ) ) ;
#30867 = PLANE ( 'NONE',  #5960 ) ;
#30868 = EDGE_CURVE ( 'NONE', #20453, #21836, #10931, .T. ) ;
#30869 = EDGE_CURVE ( 'NONE', #21081, #18600, #34183, .T. ) ;
#30870 = DIRECTION ( 'NONE',  ( 0.000000000000000000, -1.000000000000000000, 0.000000000000000000 ) ) ;
#30871 = ORIENTED_EDGE ( 'NONE', *, *, #21961, .T. ) ;
#30872 = DIRECTION ( 'NONE',  ( 0.000000000000000000, 0.7705132427757948044, -0.6374239897486828621 ) ) ;
#30874 = CARTESIAN_POINT ( 'NONE',  ( 2.790000000000083080, 11.49192876466753965, -28.42779197341999264 ) ) ;
#30873 = CARTESIAN_POINT ( 'NONE',  ( -442.0000000000000000, 104.9999999999999858, -159.0000000000000000 ) ) ;
#30875 = AXIS2_PLACEMENT_3D ( 'NONE', #32926, #8723, #22438 ) ;
#30877 = ORIENTED_EDGE ( 'NONE', *, *, #12870, .F. ) ;
#30876 = VECTOR ( 'NONE', #31643, 1000.000000000000000 ) ;
#30878 = VECTOR ( 'NONE', #14660, 1000.000000000000114 ) ;
#30879 = VECTOR ( 'NONE', #27136, 1000.000000000000000 ) ;
#30880 = CARTESIAN_POINT ( 'NONE',  ( -45.00000000000000000, 3.353962854566122864, -15.81122994652406355 ) ) ;
#30881 = ORIENTED_EDGE ( 'NONE', *, *, #20259, .T. ) ;
#30883 = EDGE_CURVE ( 'NONE', #28025, #30456, #11662, .T. ) ;
#30882 = VERTEX_POINT ( 'NONE', #3800 ) ;
#30884 = EDGE_LOOP ( 'NONE', ( #1994, #19759, #12888, #14630 ) ) ;
#30885 = CARTESIAN_POINT ( 'NONE',  ( 102.4141533279665026, -5.135784989587515170, -5.469495349232144754 ) ) ;
#30886 = ORIENTED_EDGE ( 'NONE', *, *, #1080, .F. ) ;
#30887 = ORIENTED_EDGE ( 'NONE', *, *, #18175, .T. ) ;
#30888 = LINE ( 'NONE', #17730, #8756 ) ;
#30889 = ADVANCED_FACE ( 'NONE', ( #6645 ), #30521, .T. ) ;
#30890 = FACE_OUTER_BOUND ( 'NONE', #29416, .T. ) ;
#30891 = EDGE_CURVE ( 'NONE', #22434, #17624, #6820, .T. ) ;
#30892 = COLOUR_RGB ( '',0.7921568627450980005, 0.8196078431372548767, 0.9333333333333333481 ) ;
#30894 = ADVANCED_FACE ( 'NONE', ( #14693 ), #16638, .T. ) ;
#30893 = DIRECTION ( 'NONE',  ( -0.000000000000000000, -0.000000000000000000, -1.000000000000000000 ) ) ;
#30895 = FACE_OUTER_BOUND ( 'NONE', #6450, .T. ) ;
#30896 = ORIENTED_EDGE ( 'NONE', *, *, #3548, .T. ) ;
#30897 = ORIENTED_EDGE ( 'NONE', *, *, #19899, .F. ) ;
#30898 = DIRECTION ( 'NONE',  ( 0.000000000000000000, -5.145227585319922065E-49, -1.000000000000000000 ) ) ;
#30899 = DIRECTION ( 'NONE',  ( 0.000000000000000000, 0.000000000000000000, -1.000000000000000000 ) ) ;
#30900 = CARTESIAN_POINT ( 'NONE',  ( -355.0000000000000000, 114.9999999999999716, 126.0000000000000000 ) ) ;
#30901 = EDGE_CURVE ( 'NONE', #14883, #6108, #29723, .T. ) ;
#30902 = CARTESIAN_POINT ( 'NONE',  ( 12.00000000000001066, -32.99999999999997158, 154.9999999999999716 ) ) ;
#30903 = CARTESIAN_POINT ( 'NONE',  ( -418.0000000000000000, 113.0000000000000000, -155.0000000000000000 ) ) ;
#30904 = AXIS2_PLACEMENT_3D ( 'NONE', #22785, #20468, #4249 ) ;
#30905 = CARTESIAN_POINT ( 'NONE',  ( 2.790000000000082636, 30.16006060148120582, -5.529416874851581731 ) ) ;
#30906 = AXIS2_PLACEMENT_3D ( 'NONE', #13624, #19323, #10949 ) ;
#30907 = VECTOR ( 'NONE', #28298, 1000.000000000000000 ) ;
#30908 = ORIENTED_EDGE ( 'NONE', *, *, #30452, .T. ) ;
#30909 = CARTESIAN_POINT ( 'NONE',  ( 145.0000000000000568, -78.33668825982579165, -75.00000000000001421 ) ) ;
#30910 = CARTESIAN_POINT ( 'NONE',  ( 0.000000000000000000, 9.869977788041397915, -27.85166815053926115 ) ) ;
#30911 = DIRECTION ( 'NONE',  ( 0.000000000000000000, 7.888609052210118054E-31, 1.000000000000000000 ) ) ;
#30912 = EDGE_LOOP ( 'NONE', ( #1680, #3551, #1644, #29445 ) ) ;
#30913 = EDGE_CURVE ( 'NONE', #9416, #32148, #15872, .T. ) ;
#30914 = EDGE_CURVE ( 'NONE', #13611, #9466, #27415, .T. ) ;
#30915 = DIRECTION ( 'NONE',  ( 0.000000000000000000, 0.000000000000000000, -1.000000000000000000 ) ) ;
#30916 = ORIENTED_EDGE ( 'NONE', *, *, #19004, .F. ) ;
#30917 = DIRECTION ( 'NONE',  ( 0.000000000000000000, 5.145227585319922065E-49, 1.000000000000000000 ) ) ;
#30918 = CARTESIAN_POINT ( 'NONE',  ( 2.765921099433442443, -30.46391896562403190, -6.211548095912885259 ) ) ;
#30919 = VECTOR ( 'NONE', #10366, 1000.000000000000000 ) ;
#30920 = ORIENTED_EDGE ( 'NONE', *, *, #18806, .T. ) ;
#30921 = DIRECTION ( 'NONE',  ( 0.9635499925192230197, -0.2675283385292204774, -0.000000000000000000 ) ) ;
#30922 = PLANE ( 'NONE',  #23060 ) ;
#30923 = CARTESIAN_POINT ( 'NONE',  ( 2.790000000000081304, -26.00660110917952750, 16.24378060718745687 ) ) ;
#30924 = VERTEX_POINT ( 'NONE', #12365 ) ;
#30925 = PRODUCT_DEFINITION_FORMATION_WITH_SPECIFIED_SOURCE ( 'ANY', '', #14046, .NOT_KNOWN. ) ;
#30926 = CARTESIAN_POINT ( 'NONE',  ( 814.8007456722230017, 960.5761160671663674, 1753.598338701303646 ) ) ;
#30927 = AXIS2_PLACEMENT_3D ( 'NONE', #13496, #8322, #138 ) ;
#30928 = DIRECTION ( 'NONE',  ( 0.000000000000000000, 1.000000000000000000, 5.053935297177146739E-49 ) ) ;
#30929 = EDGE_LOOP ( 'NONE', ( #28805, #10631, #7176, #29006, #1346 ) ) ;
#30930 = CARTESIAN_POINT ( 'NONE',  ( 0.7564103397028663078, -25.08336923281162001, 22.82737131378414119 ) ) ;
#30931 = CIRCLE ( 'NONE', #32059, 34.41491905851385269 ) ;
#30932 = EDGE_CURVE ( 'NONE', #33546, #12281, #31953, .T. ) ;
#30933 = DIRECTION ( 'NONE',  ( 0.000000000000000000, 1.000000000000000000, -0.000000000000000000 ) ) ;
#30934 = ADVANCED_FACE ( 'NONE', ( #2305 ), #21711, .T. ) ;
#30935 = CARTESIAN_POINT ( 'NONE',  ( -145.0000000000000568, -87.50000000000000000, 51.88904920397797582 ) ) ;
#30936 = CYLINDRICAL_SURFACE ( 'NONE', #5688, 15.00000000000000000 ) ;
#30937 = CONTEXT_DEPENDENT_SHAPE_REPRESENTATION ( #10106, #1517 ) ;
#30938 = ORIENTED_EDGE ( 'NONE', *, *, #35041, .F. ) ;
#30939 = ORIENTED_EDGE ( 'NONE', *, *, #21608, .F. ) ;
#30940 = ORIENTED_EDGE ( 'NONE', *, *, #30431, .T. ) ;
#30941 = FILL_AREA_STYLE ('',( #3523 ) ) ;
#30942 = DIRECTION ( 'NONE',  ( 1.000000000000000000, 0.000000000000000000, -0.000000000000000000 ) ) ;
#30943 = VECTOR ( 'NONE', #10798, 1000.000000000000000 ) ;
#30944 = CARTESIAN_POINT ( 'NONE',  ( 2.033589657508612536, 33.71046419695407081, 3.724096820061226332 ) ) ;
#30945 = CARTESIAN_POINT ( 'NONE',  ( 0.02407890056655781832, 4.286445725888479608, -30.79383171238939809 ) ) ;
#30946 = ORIENTED_EDGE ( 'NONE', *, *, #1447, .F. ) ;
#30947 = DIRECTION ( 'NONE',  ( -0.6051742151937650194, 0.7960930657056437543, 0.000000000000000000 ) ) ;
#30948 = LINE ( 'NONE', #9421, #24911 ) ;
#30949 = ORIENTED_EDGE ( 'NONE', *, *, #3726, .T. ) ;
#30950 = EDGE_CURVE ( 'NONE', #11706, #24474, #10329, .T. ) ;
#30951 = AXIS2_PLACEMENT_3D ( 'NONE', #30986, #33649, #17488 ) ;
#30952 = CYLINDRICAL_SURFACE ( 'NONE', #6088, 7.999999999999992895 ) ;
#30953 = CARTESIAN_POINT ( 'NONE',  ( 110.7380848894536882, 0.3849557905273008340, 12.50000000000000533 ) ) ;
#30954 = CARTESIAN_POINT ( 'NONE',  ( 2.789999999999999147, 0.000000000000000000, 0.000000000000000000 ) ) ;
#30955 = ORIENTED_EDGE ( 'NONE', *, *, #28480, .F. ) ;
#30956 = CARTESIAN_POINT ( 'NONE',  ( 0.000000000000000000, 0.000000000000000000, 0.000000000000000000 ) ) ;
#30957 = CIRCLE ( 'NONE', #23555, 7.999999999999979572 ) ;
#30958 = VECTOR ( 'NONE', #11046, 1000.000000000000000 ) ;
#30959 = CARTESIAN_POINT ( 'NONE',  ( 2.765921099433442887, -23.70329957282599764, 20.11932597908820242 ) ) ;
#30960 = ORIENTED_EDGE ( 'NONE', *, *, #7938, .F. ) ;
#30961 = LINE ( 'NONE', #6740, #12412 ) ;
#30963 = CIRCLE ( 'NONE', #10509, 7.999999999999979572 ) ;
#30962 = DIRECTION ( 'NONE',  ( -1.000000000000000000, 0.000000000000000000, 0.000000000000000000 ) ) ;
#30964 = DIRECTION ( 'NONE',  ( -0.7071067811865435759, 8.659560562354980929E-17, -0.7071067811865514585 ) ) ;
#30965 = CARTESIAN_POINT ( 'NONE',  ( -100.9438390900021432, -3.120668149329707486, 12.10491939767606873 ) ) ;
#30966 = CARTESIAN_POINT ( 'NONE',  ( 2.606461982302225699, 30.42925477731488826, -10.74656554331663827 ) ) ;
#30967 = ADVANCED_FACE ( 'NONE', ( #25878 ), #23213, .F. ) ;
#30968 = DIRECTION ( 'NONE',  ( 0.000000000000000000, 0.000000000000000000, 1.000000000000000000 ) ) ;
#30969 = ORIENTED_EDGE ( 'NONE', *, *, #18667, .F. ) ;
#30970 = VECTOR ( 'NONE', #30136, 1000.000000000000000 ) ;
#30971 = ORIENTED_EDGE ( 'NONE', *, *, #19615, .F. ) ;
#30972 = CARTESIAN_POINT ( 'NONE',  ( 782.2797628629703013, 1100.620984972938004, 1753.598338701303646 ) ) ;
#30973 = ORIENTED_EDGE ( 'NONE', *, *, #22091, .F. ) ;
#30974 = VECTOR ( 'NONE', #14764, 1000.000000000000000 ) ;
#30975 = ADVANCED_FACE ( 'NONE', ( #24198 ), #7648, .T. ) ;
#30976 = VECTOR ( 'NONE', #22113, 1000.000000000000000 ) ;
#30977 = EDGE_CURVE ( 'NONE', #594, #9940, #26836, .T. ) ;
#30978 = LINE ( 'NONE', #3209, #24317 ) ;
#30979 = ADVANCED_FACE ( 'NONE', ( #8178 ), #35077, .F. ) ;
#30980 = VECTOR ( 'NONE', #19720, 1000.000000000000000 ) ;
#30981 = DIRECTION ( 'NONE',  ( -1.000000000000000000, 6.792721752314501023E-48, -3.697785493223492838E-32 ) ) ;
#30982 = VECTOR ( 'NONE', #33282, 1000.000000000000000 ) ;
#30983 = ORIENTED_EDGE ( 'NONE', *, *, #29097, .F. ) ;
#30984 = FACE_OUTER_BOUND ( 'NONE', #32808, .T. ) ;
#30985 = CLOSED_SHELL ( 'NONE', ( #34850, #24059, #1992, #28098, #20623, #16811, #15007, #21706, #14880, #170, #20808, #31739, #18866, #5330, #34230, #1838, #31578, #26432 ) ) ;
#30987 = LINE ( 'NONE', #19789, #12427 ) ;
#30986 = CARTESIAN_POINT ( 'NONE',  ( -349.0000000000000000, -125.0000000000000284, 181.0000000000000000 ) ) ;
#30988 = ORIENTED_EDGE ( 'NONE', *, *, #23464, .T. ) ;
#30989 = ORIENTED_EDGE ( 'NONE', *, *, #29998, .F. ) ;
#30990 = CARTESIAN_POINT ( 'NONE',  ( -19.99999999999998934, 4.559999999999909015, 177.7400000000000091 ) ) ;
#30991 = CARTESIAN_POINT ( 'NONE',  ( 143.0000000000000568, -85.49999999999998579, 65.00000000000000000 ) ) ;
#30992 = LINE ( 'NONE', #34005, #30778 ) ;
#30993 = ORIENTED_EDGE ( 'NONE', *, *, #21511, .T. ) ;
#30994 = CARTESIAN_POINT ( 'NONE',  ( 2.789999999999999147, 17.11426446101236820, -26.96776559937708129 ) ) ;
#30995 = AXIS2_PLACEMENT_3D ( 'NONE', #1126, #11992, #23017 ) ;
#30996 = DIRECTION ( 'NONE',  ( 1.000000000000000000, 0.000000000000000000, 0.000000000000000000 ) ) ;
#30997 = AXIS2_PLACEMENT_3D ( 'NONE', #2395, #13446, #32295 ) ;
#30998 = VERTEX_POINT ( 'NONE', #13188 ) ;
#30999 = AXIS2_PLACEMENT_3D ( 'NONE', #6328, #25019, #30374 ) ;
#31000 = FACE_OUTER_BOUND ( 'NONE', #31034, .T. ) ;
#31001 = PLANE ( 'NONE',  #30213 ) ;
#31002 = DIRECTION ( 'NONE',  ( -0.000000000000000000, 1.836970198721029934E-16, -1.000000000000000000 ) ) ;
#31004 = DIRECTION ( 'NONE',  ( 0.000000000000000000, 0.000000000000000000, -1.000000000000000000 ) ) ;
#31003 = DIRECTION ( 'NONE',  ( -0.000000000000000000, -1.836970198721029688E-16, 1.000000000000000000 ) ) ;
#31005 = VECTOR ( 'NONE', #19031, 1000.000000000000000 ) ;
#31006 =( REPRESENTATION_RELATIONSHIP ('NONE','NONE', #23037, #15767 ) REPRESENTATION_RELATIONSHIP_WITH_TRANSFORMATION ( #3743 )SHAPE_REPRESENTATION_RELATIONSHIP( ) );
#31007 = CARTESIAN_POINT ( 'NONE',  ( 0.5248940958085364095, 13.50646231473678327, -30.52517305359770816 ) ) ;
#31009 = VECTOR ( 'NONE', #20220, 1000.000000000000000 ) ;
#31008 = CARTESIAN_POINT ( 'NONE',  ( 0.02407890056655695096, -21.56796757982826307, 22.39322359481599278 ) ) ;
#31010 = VERTEX_POINT ( 'NONE', #6993 ) ;
#31011 = CARTESIAN_POINT ( 'NONE',  ( 2.719010707633259916, -8.452877438714052616, -30.54658108095620861 ) ) ;
#31012 = CARTESIAN_POINT ( 'NONE',  ( 0.7564103437026272747, -29.46130761496082329, -16.80165608683667955 ) ) ;
#31013 = VECTOR ( 'NONE', #12016, 1000.000000000000000 ) ;
#31014 = ORIENTED_EDGE ( 'NONE', *, *, #1007, .F. ) ;
#31015 =( NAMED_UNIT ( * ) SI_UNIT ( $, .STERADIAN. ) SOLID_ANGLE_UNIT ( ) );
#31016 = EDGE_CURVE ( 'NONE', #29402, #22892, #20617, .T. ) ;
#31017 = ORIENTED_EDGE ( 'NONE', *, *, #34159, .F. ) ;
#31018 = EDGE_CURVE ( 'NONE', #33119, #15570, #202, .T. ) ;
#31019 = AXIS2_PLACEMENT_3D ( 'NONE', #20055, #5968, #30898 ) ;
#31020 = ADVANCED_FACE ( 'NONE', ( #5328 ), #27052, .T. ) ;
#31021 = CARTESIAN_POINT ( 'NONE',  ( -361.0000000000000000, 134.9999999999999716, 128.0000000000000000 ) ) ;
#31022 = ORIENTED_EDGE ( 'NONE', *, *, #20187, .F. ) ;
#31023 = B_SPLINE_CURVE_WITH_KNOTS ( 'NONE', 3,
 ( #25705, #30705, #30874, #9343 ),
 .UNSPECIFIED., .F., .F.,
 ( 4, 4 ),
 ( 3.087659402382905059E-07, 0.0006880453895801965291 ),
 .UNSPECIFIED. ) ;
#31024 = ORIENTED_EDGE ( 'NONE', *, *, #13147, .F. ) ;
#31025 = ORIENTED_EDGE ( 'NONE', *, *, #29727, .T. ) ;
#31026 = EDGE_CURVE ( 'NONE', #31513, #28476, #28718, .T. ) ;
#31027 = CARTESIAN_POINT ( 'NONE',  ( -143.0000000000000568, -85.49999999999998579, 63.00000000000000000 ) ) ;
#31028 = VECTOR ( 'NONE', #4313, 1000.000000000000000 ) ;
#31029 = CONTEXT_DEPENDENT_SHAPE_REPRESENTATION ( #19009, #23502 ) ;
#31030 = ORIENTED_EDGE ( 'NONE', *, *, #28498, .T. ) ;
#31031 = CYLINDRICAL_SURFACE ( 'NONE', #3284, 7.999999999999979572 ) ;
#31032 = FACE_OUTER_BOUND ( 'NONE', #22988, .T. ) ;
#31033 = VERTEX_POINT ( 'NONE', #19065 ) ;
#31034 = EDGE_LOOP ( 'NONE', ( #10914, #8691, #15579, #34255 ) ) ;
#31035 = DIRECTION ( 'NONE',  ( 0.000000000000000000, 0.000000000000000000, 1.000000000000000000 ) ) ;
#31036 = CARTESIAN_POINT ( 'NONE',  ( 0.07094831638746298963, -28.42120447776880354, 14.02663268823279630 ) ) ;
#31037 = VECTOR ( 'NONE', #7699, 1000.000000000000114 ) ;
#31038 = ADVANCED_FACE ( 'NONE', ( #3540 ), #27401, .F. ) ;
#31039 = CARTESIAN_POINT ( 'NONE',  ( -12.25939112814508825, 30.14816249862102637, 68.31122994652405112 ) ) ;
#31040 = CARTESIAN_POINT ( 'NONE',  ( -442.0000000000000000, 145.0000000000000000, -175.0000000000000000 ) ) ;
#31041 = CARTESIAN_POINT ( 'NONE',  ( -23.93921925319781963, 29.33115633223347274, -36.68877005347593467 ) ) ;
#31042 = ORIENTED_EDGE ( 'NONE', *, *, #10214, .T. ) ;
#31043 = FACE_OUTER_BOUND ( 'NONE', #31358, .T. ) ;
#31044 = LINE ( 'NONE', #14506, #24761 ) ;
#31045 = CARTESIAN_POINT ( 'NONE',  ( 145.0000000000000568, -177.8172209610550851, -45.87893859614474223 ) ) ;
#31046 = ORIENTED_EDGE ( 'NONE', *, *, #6425, .F. ) ;
#31047 = CARTESIAN_POINT ( 'NONE',  ( 0.02407890056655521624, 28.29688452313399338, 12.88099432405614309 ) ) ;
#31048 = LINE ( 'NONE', #33358, #32512 ) ;
#31049 = DIRECTION ( 'NONE',  ( 0.000000000000000000, 1.000000000000000000, 1.836970198721029688E-16 ) ) ;
#31050 = DIRECTION ( 'NONE',  ( 0.000000000000000000, 0.000000000000000000, -1.000000000000000000 ) ) ;
#31052 = FACE_OUTER_BOUND ( 'NONE', #22353, .T. ) ;
#31051 = PLANE ( 'NONE',  #16766 ) ;
#31053 = AXIS2_PLACEMENT_3D ( 'NONE', #3266, #33346, #14140 ) ;
#31054 = DIRECTION ( 'NONE',  ( -0.000000000000000000, 1.836970198721029934E-16, -1.000000000000000000 ) ) ;
#31055 = ORIENTED_EDGE ( 'NONE', *, *, #9724, .T. ) ;
#31056 = LINE ( 'NONE', #3977, #14457 ) ;
#31058 = PLANE ( 'NONE',  #29939 ) ;
#31057 = DIRECTION ( 'NONE',  ( 0.6051742151937647973, 0.7960930657056438653, 0.000000000000000000 ) ) ;
#31059 = AXIS2_PLACEMENT_3D ( 'NONE', #13577, #24936, #571 ) ;
#31060 = ORIENTED_EDGE ( 'NONE', *, *, #18809, .T. ) ;
#31061 =( REPRESENTATION_RELATIONSHIP ('NONE','NONE', #23037, #28231 ) REPRESENTATION_RELATIONSHIP_WITH_TRANSFORMATION ( #11242 )SHAPE_REPRESENTATION_RELATIONSHIP( ) );
#31062 = LINE ( 'NONE', #9346, #14896 ) ;
#31063 = CIRCLE ( 'NONE', #15726, 1.649999999999999911 ) ;
#31064 = VERTEX_POINT ( 'NONE', #22245 ) ;
#31065 = EDGE_CURVE ( 'NONE', #17606, #4766, #16925, .T. ) ;
#31066 = ORIENTED_EDGE ( 'NONE', *, *, #17006, .T. ) ;
#31067 = CARTESIAN_POINT ( 'NONE',  ( 108.4931367044692934, -4.566352457759228045, -5.955250171528614800 ) ) ;
#31068 = ORIENTED_EDGE ( 'NONE', *, *, #34307, .F. ) ;
#31069 = ORIENTED_EDGE ( 'NONE', *, *, #7540, .T. ) ;
#31070 = EDGE_CURVE ( 'NONE', #15610, #17344, #26852, .T. ) ;
#31071 = DIRECTION ( 'NONE',  ( 0.000000000000000000, -0.000000000000000000, -1.000000000000000000 ) ) ;
#31072 = PRODUCT_DEFINITION_SHAPE ( 'NONE', 'NONE',  #35188 ) ;
#31073 = ADVANCED_FACE ( 'NONE', ( #30432 ), #889, .F. ) ;
#31074 = CARTESIAN_POINT ( 'NONE',  ( 2.033589658210382733, 22.02455111472429650, 25.79115045147389296 ) ) ;
#31075 = AXIS2_PLACEMENT_3D ( 'NONE', #10191, #12877, #34574 ) ;
#31076 = CARTESIAN_POINT ( 'NONE',  ( -499.9999999999999432, 136.9999999999999432, 162.9999999999999716 ) ) ;
#31077 = CARTESIAN_POINT ( 'NONE',  ( 19.99999999999998224, 134.9999999999999432, -162.9999999999999432 ) ) ;
#31078 = EDGE_CURVE ( 'NONE', #30843, #26104, #32912, .T. ) ;
#31079 = EDGE_LOOP ( 'NONE', ( #16458, #4163, #11151, #3771 ) ) ;
#31080 = EDGE_CURVE ( 'NONE', #8775, #18155, #22605, .T. ) ;
#31081 = ORIENTED_EDGE ( 'NONE', *, *, #26682, .F. ) ;
#31082 = LINE ( 'NONE', #28922, #18543 ) ;
#31083 = CARTESIAN_POINT ( 'NONE',  ( -70.00000000000000000, 75.55999999999990280, 177.7400000000000091 ) ) ;
#31084 = DIRECTION ( 'NONE',  ( 0.000000000000000000, 1.836970198721029688E-16, -1.000000000000000000 ) ) ;
#31085 = VECTOR ( 'NONE', #19492, 1000.000000000000000 ) ;
#31086 = CARTESIAN_POINT ( 'NONE',  ( -27.84632068199329780, 25.66368763279034226, 68.31122994652405112 ) ) ;
#31087 = CARTESIAN_POINT ( 'NONE',  ( -442.0000000000000000, 105.0000000000000142, 162.9999999999999716 ) ) ;
#31088 = DIRECTION ( 'NONE',  ( 0.000000000000000000, 1.836970198721029688E-16, -1.000000000000000000 ) ) ;
#31089 = CARTESIAN_POINT ( 'NONE',  ( 10.62930655775863364, -36.34639295086970634, -36.68877005347593467 ) ) ;
#31090 = EDGE_LOOP ( 'NONE', ( #2301, #24363 ) ) ;
#31091 = VECTOR ( 'NONE', #24821, 1000.000000000000000 ) ;
#31092 = CARTESIAN_POINT ( 'NONE',  ( 0.000000000000000000, -30.41598411195412055, 1.821977758773545952 ) ) ;
#31093 = CARTESIAN_POINT ( 'NONE',  ( -355.0000000000000000, 134.9999999999999716, 113.9999999999999858 ) ) ;
#31094 = EDGE_CURVE ( 'NONE', #27019, #22138, #5825, .T. ) ;
#31095 = DIRECTION ( 'NONE',  ( -1.000000000000000000, -0.000000000000000000, 0.000000000000000000 ) ) ;
#31096 = ORIENTED_EDGE ( 'NONE', *, *, #23547, .T. ) ;
#31097 = CARTESIAN_POINT ( 'NONE',  ( -445.9999999999999432, -125.0000000000000000, 107.9999999999999858 ) ) ;
#31098 = ORIENTED_EDGE ( 'NONE', *, *, #29582, .T. ) ;
#31099 = CARTESIAN_POINT ( 'NONE',  ( 2.765921099433441999, -3.506335382740735529, 30.89238256715863784 ) ) ;
#31100 = DIRECTION ( 'NONE',  ( -1.000000000000000000, 0.000000000000000000, -0.000000000000000000 ) ) ;
#31101 = ADVANCED_FACE ( 'NONE', ( #180 ), #19762, .F. ) ;
#31102 = CIRCLE ( 'NONE', #18032, 15.00000000000000000 ) ;
#31103 = EDGE_CURVE ( 'NONE', #29721, #22453, #29145, .T. ) ;
#31104 = ORIENTED_EDGE ( 'NONE', *, *, #18667, .T. ) ;
#31105 = CARTESIAN_POINT ( 'NONE',  ( 11.99999999999999645, 124.9999999999999716, 155.0000000000000000 ) ) ;
#31106 = CARTESIAN_POINT ( 'NONE',  ( 0.02407890056655608360, -31.05158812718222450, 1.559667679918499417 ) ) ;
#31107 = CARTESIAN_POINT ( 'NONE',  ( 1.749999999999999778, 14.40815186467775888, 31.25366880301323746 ) ) ;
#31108 = VERTEX_POINT ( 'NONE', #30609 ) ;
#31109 = DIRECTION ( 'NONE',  ( 2.631201909438060585E-14, -5.396010391056496978E-16, 1.000000000000000000 ) ) ;
#31110 = VECTOR ( 'NONE', #3474, 1000.000000000000000 ) ;
#31111 = CYLINDRICAL_SURFACE ( 'NONE', #15928, 34.41491905851385269 ) ;
#31112 = B_SPLINE_CURVE_WITH_KNOTS ( 'NONE', 3,
 ( #20521, #12001, #28538, #20184, #31036, #9836 ),
 .UNSPECIFIED., .F., .F.,
 ( 4, 2, 4 ),
 ( 4.404817209449920197E-07, 0.001874269760234692061, 0.003748099038748438881 ),
 .UNSPECIFIED. ) ;
#31113 = VERTEX_POINT ( 'NONE', #25252 ) ;
#31114 = CARTESIAN_POINT ( 'NONE',  ( 30.69344702212033127, -10.82204614554912681, 68.31122994652405112 ) ) ;
#31115 = DIRECTION ( 'NONE',  ( 1.000000000000000000, 0.000000000000000000, 0.000000000000000000 ) ) ;
#31116 = CARTESIAN_POINT ( 'NONE',  ( 15.99999999999998579, 4.559999999999909015, 177.7400000000000091 ) ) ;
#31117 = DIRECTION ( 'NONE',  ( 0.000000000000000000, 1.000000000000000000, 5.053935297177146739E-49 ) ) ;
#31118 = CONTEXT_DEPENDENT_SHAPE_REPRESENTATION ( #34218, #20560 ) ;
#31119 = EDGE_CURVE ( 'NONE', #16921, #21448, #5848, .T. ) ;
#31120 = ORIENTED_EDGE ( 'NONE', *, *, #18346, .T. ) ;
#31121 = ADVANCED_FACE ( 'NONE', ( #24898 ), #6028, .T. ) ;
#31122 = ORIENTED_EDGE ( 'NONE', *, *, #3805, .F. ) ;
#31123 = ORIENTED_EDGE ( 'NONE', *, *, #6772, .T. ) ;
#31124 = CARTESIAN_POINT ( 'NONE',  ( -414.0000000000000568, 105.0000000000000142, 187.0000000000000000 ) ) ;
#31125 = CARTESIAN_POINT ( 'NONE',  ( 1.205771365940061957, -15.58845726811992449, 7.826847450972439323E-16 ) ) ;
#31126 = VECTOR ( 'NONE', #19533, 1000.000000000000227 ) ;
#31127 = AXIS2_PLACEMENT_3D ( 'NONE', #405, #930, #30653 ) ;
#31128 = DIRECTION ( 'NONE',  ( -0.000000000000000000, 1.000000000000000000, -0.000000000000000000 ) ) ;
#31129 = DIRECTION ( 'NONE',  ( 1.000000000000000000, 0.000000000000000000, 0.000000000000000000 ) ) ;
#31130 = CARTESIAN_POINT ( 'NONE',  ( -20.02113311122478123, 16.12922284503173742, -67.50000000000000000 ) ) ;
#31131 = FACE_OUTER_BOUND ( 'NONE', #23989, .T. ) ;
#31132 = VERTEX_POINT ( 'NONE', #13705 ) ;
#31133 = CARTESIAN_POINT ( 'NONE',  ( 103.1340045722813130, 5.439315735761663717, 11.25565174199232743 ) ) ;
#31134 = AXIS2_PLACEMENT_3D ( 'NONE', #29139, #34664, #10271 ) ;
#31135 = ORIENTED_EDGE ( 'NONE', *, *, #29893, .T. ) ;
#31136 = CARTESIAN_POINT ( 'NONE',  ( 2.719010744112896116, -15.78394019282702132, -27.48475859319554715 ) ) ;
#31137 = LINE ( 'NONE', #25781, #6395 ) ;
#31138 = ORIENTED_EDGE ( 'NONE', *, *, #1601, .F. ) ;
#31139 = CARTESIAN_POINT ( 'NONE',  ( -355.0000000000000000, -135.0000000000000000, 113.9999999999999858 ) ) ;
#31140 = CARTESIAN_POINT ( 'NONE',  ( 15.99999999999998579, -115.0000000000000000, 174.9999999999999432 ) ) ;
#31141 = EDGE_CURVE ( 'NONE', #9326, #25124, #10955, .T. ) ;
#31142 = CARTESIAN_POINT ( 'NONE',  ( -500.0000000000000000, -137.0000000000000000, 187.0000000000000000 ) ) ;
#31143 = EDGE_CURVE ( 'NONE', #26377, #5208, #30247, .T. ) ;
#31144 = EDGE_CURVE ( 'NONE', #29254, #199, #710, .T. ) ;
#31145 = VECTOR ( 'NONE', #17405, 1000.000000000000000 ) ;
#31146 = CARTESIAN_POINT ( 'NONE',  ( -110.1150203881708336, -0.1683156175999609427, 12.50000000000000000 ) ) ;
#31147 = CARTESIAN_POINT ( 'NONE',  ( 2.789999999999999147, 30.93646776788796160, 7.943134866716423659 ) ) ;
#31148 = PLANE ( 'NONE',  #13756 ) ;
#31149 = EDGE_CURVE ( 'NONE', #21389, #31871, #21010, .T. ) ;
#31150 = VERTEX_POINT ( 'NONE', #14247 ) ;
#31151 = AXIS2_PLACEMENT_3D ( 'NONE', #2463, #13344, #32532 ) ;
#31152 = VECTOR ( 'NONE', #5331, 1000.000000000000000 ) ;
#31153 = EDGE_CURVE ( 'NONE', #319, #9821, #16571, .T. ) ;
#31154 = ORIENTED_EDGE ( 'NONE', *, *, #12068, .F. ) ;
#31155 = DIRECTION ( 'NONE',  ( -0.6450379176759554190, 0.7641505641954781103, -2.405639128100926250E-14 ) ) ;
#31156 = ORIENTED_EDGE ( 'NONE', *, *, #32694, .F. ) ;
#31157 = CIRCLE ( 'NONE', #11267, 9.999999999999994671 ) ;
#31158 = CARTESIAN_POINT ( 'NONE',  ( -31.68358972719163091, 7.440061483287550459, -36.68877005347593467 ) ) ;
#31159 = LINE ( 'NONE', #17646, #20477 ) ;
#31160 = ORIENTED_EDGE ( 'NONE', *, *, #19594, .F. ) ;
#31161 = CARTESIAN_POINT ( 'NONE',  ( -418.0000000000000000, 105.0000000000000000, -69.99999999999998579 ) ) ;
#31162 = CARTESIAN_POINT ( 'NONE',  ( -99.89326661827516318, -0.3368495349214569723, -12.49660185505138976 ) ) ;
#31164 = CYLINDRICAL_SURFACE ( 'NONE', #2744, 16.19999999999999574 ) ;
#31163 = LINE ( 'NONE', #9966, #11629 ) ;
#31165 = VECTOR ( 'NONE', #30847, 1000.000000000000227 ) ;
#31166 = ORIENTED_EDGE ( 'NONE', *, *, #32887, .T. ) ;
#31167 = ORIENTED_EDGE ( 'NONE', *, *, #21510, .F. ) ;
#31168 = CARTESIAN_POINT ( 'NONE',  ( 15.44711578872682445, -28.64595934308655600, 49.43553178847298568 ) ) ;
#31169 = DIRECTION ( 'NONE',  ( 1.000000000000000000, 0.000000000000000000, 0.000000000000000000 ) ) ;
#31170 = PLANE ( 'NONE',  #20540 ) ;
#31171 = ORIENTED_EDGE ( 'NONE', *, *, #5480, .F. ) ;
#31172=STYLED_ITEM('',(#35275),#10060);
#31173 = CYLINDRICAL_SURFACE ( 'NONE', #8904, 7.999999999999986677 ) ;
#31174 = MECHANICAL_DESIGN_GEOMETRIC_PRESENTATION_REPRESENTATION (  '', ( #18605 ), #26614 ) ;
#31175 = ORIENTED_EDGE ( 'NONE', *, *, #13740, .T. ) ;
#31176 = CARTESIAN_POINT ( 'NONE',  ( -19.99999999999998934, -145.0000000000000000, 187.0000000000000000 ) ) ;
#31177 = DIRECTION ( 'NONE',  ( -1.000000000000000000, 0.000000000000000000, 1.232595164407831220E-32 ) ) ;
#31178 = CARTESIAN_POINT ( 'NONE',  ( -7.700000000000000178, 0.000000000000000000, 0.000000000000000000 ) ) ;
#31179 = AXIS2_PLACEMENT_3D ( 'NONE', #23880, #2698, #10727 ) ;
#31180 = EDGE_CURVE ( 'NONE', #19820, #9756, #17097, .T. ) ;
#31182 = DIRECTION ( 'NONE',  ( 0.000000000000000000, 0.000000000000000000, 1.000000000000000000 ) ) ;
#31181 = DIRECTION ( 'NONE',  ( -0.000000000000000000, 1.000000000000000000, -0.000000000000000000 ) ) ;
#31183 = EDGE_CURVE ( 'NONE', #22142, #24957, #23299, .T. ) ;
#31184 = CARTESIAN_POINT ( 'NONE',  ( 0.000000000000000000, -11.13185981125856294, -28.36429779836965182 ) ) ;
#31185 = DIRECTION ( 'NONE',  ( 1.000000000000000000, 0.000000000000000000, 0.000000000000000000 ) ) ;
#31186 = ORIENTED_EDGE ( 'NONE', *, *, #26993, .F. ) ;
#31187 = DIRECTION ( 'NONE',  ( 0.000000000000000000, 0.000000000000000000, -1.000000000000000000 ) ) ;
#31188 = CARTESIAN_POINT ( 'NONE',  ( 145.0000000000000568, 87.50000000000000000, -65.00000000000000000 ) ) ;
#31189 = VECTOR ( 'NONE', #3002, 1000.000000000000114 ) ;
#31190 = CIRCLE ( 'NONE', #6736, 10.00000000000000000 ) ;
#31191 = VERTEX_POINT ( 'NONE', #9429 ) ;
#31192 = ORIENTED_EDGE ( 'NONE', *, *, #163, .F. ) ;
#31193 = COLOUR_RGB ( '',0.7921568627450980005, 0.8196078431372548767, 0.9333333333333333481 ) ;
#31194 = CARTESIAN_POINT ( 'NONE',  ( 0.02407890056655781832, 18.59128259035472297, 24.91982945642928016 ) ) ;
#31195 = ORIENTED_EDGE ( 'NONE', *, *, #18673, .F. ) ;
#31196 = ORIENTED_EDGE ( 'NONE', *, *, #26968, .T. ) ;
#31197 = EDGE_LOOP ( 'NONE', ( #2943, #19487 ) ) ;
#31198 = CARTESIAN_POINT ( 'NONE',  ( 0.000000000000000000, 0.000000000000000000, 0.000000000000000000 ) ) ;
#31199 = CONTEXT_DEPENDENT_SHAPE_REPRESENTATION ( #29232, #34304 ) ;
#31200 = ORIENTED_EDGE ( 'NONE', *, *, #21912, .T. ) ;
#31201 = DIRECTION ( 'NONE',  ( 1.000000000000000000, -0.000000000000000000, -0.000000000000000000 ) ) ;
#31202 = FACE_OUTER_BOUND ( 'NONE', #32168, .T. ) ;
#31203 = ORIENTED_EDGE ( 'NONE', *, *, #7752, .F. ) ;
#31204 = ORIENTED_EDGE ( 'NONE', *, *, #23148, .F. ) ;
#31205 = CARTESIAN_POINT ( 'NONE',  ( -6.500000000000000000, 0.000000000000000000, 5.429999999999999716 ) ) ;
#31206 = DIRECTION ( 'NONE',  ( -1.000000000000000000, 0.000000000000000000, 0.000000000000000000 ) ) ;
#31207 = CARTESIAN_POINT ( 'NONE',  ( -12.00000000000001243, 134.9999999999998863, 194.9999999999999716 ) ) ;
#31208 = DIRECTION ( 'NONE',  ( 1.000000000000000000, 3.040835319149746090E-31, 1.232595164407830946E-32 ) ) ;
#31209 = LINE ( 'NONE', #7327, #9164 ) ;
#31210 = ORIENTED_EDGE ( 'NONE', *, *, #28224, .F. ) ;
#31211 = FACE_OUTER_BOUND ( 'NONE', #2132, .T. ) ;
#31212 = DIRECTION ( 'NONE',  ( -1.000000000000000000, -0.000000000000000000, -0.000000000000000000 ) ) ;
#31213 = VECTOR ( 'NONE', #17407, 1000.000000000000000 ) ;
#31214 = CARTESIAN_POINT ( 'NONE',  ( -355.0000000000000000, 118.9999999999999716, 126.0000000000000000 ) ) ;
#31215 = VERTEX_POINT ( 'NONE', #22950 ) ;
#31216 = CARTESIAN_POINT ( 'NONE',  ( 129.3530333899765594, 6.000000000000000000, 62.49999999999999289 ) ) ;
#31217 = CARTESIAN_POINT ( 'NONE',  ( 0.006892382889170392546, 23.98878059851183764, -19.42891868047383142 ) ) ;
#31218 = EDGE_CURVE ( 'NONE', #6516, #27008, #20285, .T. ) ;
#31219 = DIRECTION ( 'NONE',  ( 1.000000000000000000, 0.000000000000000000, 0.000000000000000000 ) ) ;
#31220 = CARTESIAN_POINT ( 'NONE',  ( 0.006892381134854739730, -23.57982834652831627, -19.92325699910571046 ) ) ;
#31222 = CARTESIAN_POINT ( 'NONE',  ( -29.34345171400087793, 14.07715221144534823, 68.31122994652405112 ) ) ;
#31221 = DIRECTION ( 'NONE',  ( 0.000000000000000000, 0.000000000000000000, 1.000000000000000000 ) ) ;
#31223 = CIRCLE ( 'NONE', #11899, 4.750000000000004441 ) ;
#31224 = EDGE_CURVE ( 'NONE', #19647, #23009, #31137, .T. ) ;
#31225 = CARTESIAN_POINT ( 'NONE',  ( 2.033589656860156136, -1.600050605840442008, 33.87778227150285915 ) ) ;
#31226 = EDGE_LOOP ( 'NONE', ( #6447, #32070, #34608, #9690, #27885, #17000, #2728, #17521, #28070 ) ) ;
#31227 = EDGE_CURVE ( 'NONE', #423, #24841, #5244, .T. ) ;
#31228 = DIRECTION ( 'NONE',  ( 0.000000000000000000, 0.000000000000000000, -1.000000000000000000 ) ) ;
#31230 = CARTESIAN_POINT ( 'NONE',  ( 0.5288002579745525455, -2.866095775114346988, 33.26657006572082054 ) ) ;
#31229 = DIRECTION ( 'NONE',  ( 3.040835319149746090E-31, 1.000000000000000000, -3.748118910144520367E-63 ) ) ;
#31231 = VECTOR ( 'NONE', #19489, 1000.000000000000000 ) ;
#31232 = VERTEX_POINT ( 'NONE', #17279 ) ;
#31233 = CARTESIAN_POINT ( 'NONE',  ( 0.000000000000000000, -33.69708579775584667, 49.43553178847298568 ) ) ;
#31234 = ORIENTED_EDGE ( 'NONE', *, *, #3073, .T. ) ;
#31235 = VECTOR ( 'NONE', #29098, 1000.000000000000000 ) ;
#31236 = ORIENTED_EDGE ( 'NONE', *, *, #5235, .T. ) ;
#31237 = CARTESIAN_POINT ( 'NONE',  ( 107.5840264377090421, -5.136475861867761061, -5.468785347707075140 ) ) ;
#31238 = VERTEX_POINT ( 'NONE', #17628 ) ;
#31239 = ORIENTED_EDGE ( 'NONE', *, *, #5611, .F. ) ;
#31240 = CARTESIAN_POINT ( 'NONE',  ( 0.5288002558916620188, -18.53787122671754162, 27.77096539590122504 ) ) ;
#31241 = CYLINDRICAL_SURFACE ( 'NONE', #8788, 2.033421858999710619 ) ;
#31242 = DIRECTION ( 'NONE',  ( 0.000000000000000000, 0.000000000000000000, -1.000000000000000000 ) ) ;
#31243 = CARTESIAN_POINT ( 'NONE',  ( 2.789999999999999147, 9.869977788041397915, -27.85166815053926115 ) ) ;
#31244 = EDGE_LOOP ( 'NONE', ( #6293, #1954, #24894, #24638 ) ) ;
#31245 = ORIENTED_EDGE ( 'NONE', *, *, #24364, .F. ) ;
#31246 = CARTESIAN_POINT ( 'NONE',  ( -449.9999999999999432, -105.0000000000000142, 107.9999999999999574 ) ) ;
#31247 = DIRECTION ( 'NONE',  ( 0.000000000000000000, 0.000000000000000000, -1.000000000000000000 ) ) ;
#31248 = FACE_OUTER_BOUND ( 'NONE', #12517, .T. ) ;
#31249 = CARTESIAN_POINT ( 'NONE',  ( 2.789999999999999147, 0.000000000000000000, 0.000000000000000000 ) ) ;
#31250 = CARTESIAN_POINT ( 'NONE',  ( 35.44043929807611448, -17.65143121711728469, 14.30932821646982411 ) ) ;
#31251 = AXIS2_PLACEMENT_3D ( 'NONE', #11902, #17250, #33245 ) ;
#31252 = DIRECTION ( 'NONE',  ( -1.000000000000000000, 0.000000000000000000, -1.300283923313630633E-47 ) ) ;
#31253 = CARTESIAN_POINT ( 'NONE',  ( 1.205771365940041306, -7.794228634059936489, 13.50000000000000000 ) ) ;
#31254 = ORIENTED_EDGE ( 'NONE', *, *, #18673, .T. ) ;
#31255 = CARTESIAN_POINT ( 'NONE',  ( 0.006892384446387221988, -15.15194214258620242, 26.89541087693579868 ) ) ;
#31256 = DIRECTION ( 'NONE',  ( -3.469446951953832974E-18, -1.000000000000000000, -7.888609052210116302E-31 ) ) ;
#31257 = EDGE_CURVE ( 'NONE', #29621, #28835, #18366, .T. ) ;
#31258 = CARTESIAN_POINT ( 'NONE',  ( -70.00000000000000000, 75.55999999999990280, -172.9900000000000091 ) ) ;
#31259 = EDGE_LOOP ( 'NONE', ( #11031, #21991, #8019, #16899, #29005 ) ) ;
#31260 =( REPRESENTATION_RELATIONSHIP ('NONE','NONE', #23037, #15767 ) REPRESENTATION_RELATIONSHIP_WITH_TRANSFORMATION ( #4231 )SHAPE_REPRESENTATION_RELATIONSHIP( ) );
#31261 = CARTESIAN_POINT ( 'NONE',  ( 2.789999999999999147, 17.98401995359633077, 24.59729088254962548 ) ) ;
#31262 = ORIENTED_EDGE ( 'NONE', *, *, #3327, .F. ) ;
#31263 = EDGE_CURVE ( 'NONE', #34740, #3207, #3720, .T. ) ;
#31265 = CARTESIAN_POINT ( 'NONE',  ( 31.73435513276359643, 7.220462394039750542, 68.31122994652405112 ) ) ;
#31264 = CARTESIAN_POINT ( 'NONE',  ( -500.0000000000000000, 104.9999999999999858, 155.0000000000000000 ) ) ;
#31266 = DIRECTION ( 'NONE',  ( 0.000000000000000000, 0.000000000000000000, 1.000000000000000000 ) ) ;
#31267 = EDGE_CURVE ( 'NONE', #14449, #8838, #14948, .T. ) ;
#31268 = ORIENTED_EDGE ( 'NONE', *, *, #32090, .F. ) ;
#31269 = ADVANCED_FACE ( 'NONE', ( #22774 ), #11931, .T. ) ;
#31270 = EDGE_CURVE ( 'NONE', #28601, #17012, #14383, .T. ) ;
#31271 = CARTESIAN_POINT ( 'NONE',  ( 2.789999999999999147, -11.13185981125856827, -28.36429779836962339 ) ) ;
#31272 = CARTESIAN_POINT ( 'NONE',  ( -449.9999999999999432, -104.9999999999999858, -162.9999999999999716 ) ) ;
#31273 = EDGE_CURVE ( 'NONE', #7312, #25172, #6384, .T. ) ;
#31274 = ORIENTED_EDGE ( 'NONE', *, *, #719, .F. ) ;
#31275 = VECTOR ( 'NONE', #14969, 999.9999999999998863 ) ;
#31276 = B_SPLINE_CURVE_WITH_KNOTS ( 'NONE', 3,
 ( #3138, #483, #11344, #22189, #33028, #8653 ),
 .UNSPECIFIED., .F., .F.,
 ( 4, 2, 4 ),
 ( 4.404817011192420828E-07, 0.001874269612720305071, 0.003748098743739490622 ),
 .UNSPECIFIED. ) ;
#31277 = DIRECTION ( 'NONE',  ( -0.1063910735369225230, 0.9943243633099118073, -1.000770725407345128E-14 ) ) ;
#31278 = CARTESIAN_POINT ( 'NONE',  ( 99.26191511054632599, 1.643815732525060864E-21, 12.50000000000000000 ) ) ;
#31279 = ORIENTED_EDGE ( 'NONE', *, *, #12702, .F. ) ;
#31280 = DIRECTION ( 'NONE',  ( 1.000000000000000000, 0.000000000000000000, -1.848892746611746966E-32 ) ) ;
#31281 = CARTESIAN_POINT ( 'NONE',  ( 143.0000000000000568, -12.50000000000001066, 1.224646799147353217E-14 ) ) ;
#31282 = CARTESIAN_POINT ( 'NONE',  ( -35.00000000000000000, -4.184937238521373004, 15.81122994652407776 ) ) ;
#31283 = FACE_OUTER_BOUND ( 'NONE', #28348, .T. ) ;
#31284 = ORIENTED_EDGE ( 'NONE', *, *, #26746, .F. ) ;
#31285 = ORIENTED_EDGE ( 'NONE', *, *, #33516, .T. ) ;
#31286 = ORIENTED_EDGE ( 'NONE', *, *, #33626, .F. ) ;
#31287 = CARTESIAN_POINT ( 'NONE',  ( -18.38714294329533416, -33.09555747561021377, 68.31122994652405112 ) ) ;
#31288 = CARTESIAN_POINT ( 'NONE',  ( 145.0000000000000568, -89.01471862576147487, 43.40376782973931569 ) ) ;
#31289 = PLANE ( 'NONE',  #29269 ) ;
#31290 = LINE ( 'NONE', #4225, #10913 ) ;
#31291 = DIRECTION ( 'NONE',  ( 0.000000000000000000, 0.000000000000000000, -1.000000000000000000 ) ) ;
#31292 = ORIENTED_EDGE ( 'NONE', *, *, #19869, .T. ) ;
#31293 = VECTOR ( 'NONE', #18657, 1000.000000000000000 ) ;
#31294 = CARTESIAN_POINT ( 'NONE',  ( 100.6806599292393116, 3.795444455902926340, 11.91305592319908691 ) ) ;
#31295 = AXIS2_PLACEMENT_3D ( 'NONE', #12957, #26461, #2085 ) ;
#31296 = ORIENTED_EDGE ( 'NONE', *, *, #18312, .F. ) ;
#31297 = DIRECTION ( 'NONE',  ( 0.000000000000000000, 0.000000000000000000, -1.000000000000000000 ) ) ;
#31298 = VERTEX_POINT ( 'NONE', #20456 ) ;
#31299 = CARTESIAN_POINT ( 'NONE',  ( 2.261199752785263861, -24.86182815675638835, -22.28830832814908547 ) ) ;
#31300 = EDGE_CURVE ( 'NONE', #1893, #26714, #14960, .T. ) ;
#31301 = FACE_OUTER_BOUND ( 'NONE', #32518, .T. ) ;
#31302 = AXIS2_PLACEMENT_3D ( 'NONE', #22638, #33311, #33124 ) ;
#31303 = EDGE_CURVE ( 'NONE', #30004, #3035, #1850, .T. ) ;
#31304 = EDGE_CURVE ( 'NONE', #5389, #9440, #12106, .T. ) ;
#31305 = DIRECTION ( 'NONE',  ( -1.000000000000000000, 0.000000000000000000, 0.000000000000000000 ) ) ;
#31306 = UNCERTAINTY_MEASURE_WITH_UNIT (LENGTH_MEASURE( 1.000000000000000082E-05 ), #16628, 'distance_accuracy_value', 'NONE');
#31307 = LINE ( 'NONE', #20462, #28713 ) ;
#31308 = CARTESIAN_POINT ( 'NONE',  ( 19.99999999999998934, 4.559999999999908127, -177.7400000000000091 ) ) ;
#31309 = ORIENTED_EDGE ( 'NONE', *, *, #13147, .T. ) ;
#31310 = ORIENTED_EDGE ( 'NONE', *, *, #22745, .T. ) ;
#31311 = CARTESIAN_POINT ( 'NONE',  ( 783.6628460657107098, 1087.694775289636937, 1753.598338701303419 ) ) ;
#31312 = CIRCLE ( 'NONE', #28475, 8.000000000000007105 ) ;
#31313 = ORIENTED_EDGE ( 'NONE', *, *, #15295, .F. ) ;
#31314 = EDGE_CURVE ( 'NONE', #13351, #33784, #1748, .T. ) ;
#31315 = AXIS2_PLACEMENT_3D ( 'NONE', #16464, #24266, #71 ) ;
#31316 = LINE ( 'NONE', #19040, #7856 ) ;
#31317 = DIRECTION ( 'NONE',  ( 1.000000000000000000, 0.000000000000000000, 0.000000000000000000 ) ) ;
#31318 = ITEM_DEFINED_TRANSFORMATION ( 'NONE', 'NONE', #10389,  #28566 ) ;
#31319 = EDGE_LOOP ( 'NONE', ( #21883, #14438, #19576, #27433 ) ) ;
#31320 = LINE ( 'NONE', #20131, #29851 ) ;
#31321 = DIRECTION ( 'NONE',  ( 3.970546015203020284E-16, 0.000000000000000000, -1.000000000000000000 ) ) ;
#31322 = EDGE_CURVE ( 'NONE', #13445, #1771, #3595, .T. ) ;
#31323 = EDGE_CURVE ( 'NONE', #28665, #15358, #26132, .T. ) ;
#31324 = EDGE_CURVE ( 'NONE', #5728, #29028, #12625, .T. ) ;
#31326 = DIRECTION ( 'NONE',  ( -0.000000000000000000, -1.000000000000000000, -0.000000000000000000 ) ) ;
#31325 = LINE ( 'NONE', #6933, #34918 ) ;
#31328 = ORIENTED_EDGE ( 'NONE', *, *, #5604, .F. ) ;
#31327 = AXIS2_PLACEMENT_3D ( 'NONE', #13881, #8882, #27924 ) ;
#31329 = VERTEX_POINT ( 'NONE', #19933 ) ;
#31330 = LINE ( 'NONE', #14458, #7755 ) ;
#31331 = AXIS2_PLACEMENT_3D ( 'NONE', #17987, #9948, #34330 ) ;
#31332 = CIRCLE ( 'NONE', #16009, 1.999999999999999556 ) ;
#31333 = EDGE_CURVE ( 'NONE', #33608, #24529, #26297, .T. ) ;
#31334 = DIRECTION ( 'NONE',  ( 0.000000000000000000, 0.000000000000000000, 1.000000000000000000 ) ) ;
#31335 = LINE ( 'NONE', #25465, #18843 ) ;
#31336 = VERTEX_POINT ( 'NONE', #15830 ) ;
#31337 = FACE_OUTER_BOUND ( 'NONE', #7800, .T. ) ;
#31338 = B_SPLINE_CURVE_WITH_KNOTS ( 'NONE', 3,
 ( #698, #33432, #19919, #14236 ),
 .UNSPECIFIED., .F., .F.,
 ( 4, 4 ),
 ( 2.335573237721180036E-07, 0.0006879695513619570393 ),
 .UNSPECIFIED. ) ;
#31339 = ORIENTED_EDGE ( 'NONE', *, *, #33877, .F. ) ;
#31340 = CARTESIAN_POINT ( 'NONE',  ( -12.00000000000003908, -134.9999999999999716, -154.9999999999999716 ) ) ;
#31341 = LINE ( 'NONE', #6946, #9740 ) ;
#31342 = VECTOR ( 'NONE', #23197, 1000.000000000000000 ) ;
#31343 = DIRECTION ( 'NONE',  ( 0.000000000000000000, -1.000000000000000000, 6.123233995736766036E-17 ) ) ;
#31345 = FACE_OUTER_BOUND ( 'NONE', #22030, .T. ) ;
#31344 = CARTESIAN_POINT ( 'NONE',  ( 2.719010671502130272, 31.23843357299755041, 5.357709411917663367 ) ) ;
#31346 = EDGE_CURVE ( 'NONE', #1780, #6336, #7603, .T. ) ;
#31347 = CARTESIAN_POINT ( 'NONE',  ( -117.4999999999997442, 0.000000000000000000, 12.50000000000000000 ) ) ;
#31348 = FACE_OUTER_BOUND ( 'NONE', #11416, .T. ) ;
#31349 = FACE_OUTER_BOUND ( 'NONE', #5355, .T. ) ;
#31350 = CARTESIAN_POINT ( 'NONE',  ( 0.07094833869610567278, -27.07192087577299588, -16.48097105307910581 ) ) ;
#31351 = PRODUCT_DEFINITION_SHAPE ( 'NONE', 'NONE',  #35143 ) ;
#31352 = EDGE_LOOP ( 'NONE', ( #18390, #28912, #1379, #4166, #4290, #11458, #30091, #32817 ) ) ;
#31353 = VECTOR ( 'NONE', #20244, 1000.000000000000114 ) ;
#31354 = SHAPE_REPRESENTATION_RELATIONSHIP ( 'NONE' , 'NONE' ,  #30518, #7549 ) ;
#31355 = VECTOR ( 'NONE', #31439, 1000.000000000000000 ) ;
#31356 = AXIS2_PLACEMENT_3D ( 'NONE', #14875, #31573, #1339 ) ;
#31357 = AXIS2_PLACEMENT_3D ( 'NONE', #5851, #14250, #8712 ) ;
#31358 = EDGE_LOOP ( 'NONE', ( #15309, #20161, #13255, #15196 ) ) ;
#31359 = ORIENTED_EDGE ( 'NONE', *, *, #17553, .T. ) ;
#31360 = FACE_OUTER_BOUND ( 'NONE', #13954, .T. ) ;
#31361 = VERTEX_POINT ( 'NONE', #28982 ) ;
#31362 = EDGE_LOOP ( 'NONE', ( #28693, #34454, #4673, #17640 ) ) ;
#31363 = ORIENTED_EDGE ( 'NONE', *, *, #1972, .F. ) ;
#31364 = LINE ( 'NONE', #9310, #12816 ) ;
#31365 = AXIS2_PLACEMENT_3D ( 'NONE', #654, #12054, #23081 ) ;
#31366 = EDGE_CURVE ( 'NONE', #11554, #29991, #27014, .T. ) ;
#31367 = ADVANCED_FACE ( 'NONE', ( #13148 ), #2269, .T. ) ;
#31368 = VERTEX_POINT ( 'NONE', #23818 ) ;
#31369 = DIRECTION ( 'NONE',  ( 0.000000000000000000, 1.836970198721029441E-16, -1.000000000000000000 ) ) ;
#31370 = CARTESIAN_POINT ( 'NONE',  ( 0.07094833594414887146, 24.79283726477109084, 19.74402504231806077 ) ) ;
#31371 = ORIENTED_EDGE ( 'NONE', *, *, #23900, .T. ) ;
#31372 = ORIENTED_EDGE ( 'NONE', *, *, #2133, .T. ) ;
#31373 = CARTESIAN_POINT ( 'NONE',  ( 2.789999999999999147, -29.91351748324107263, 5.799410679710522487 ) ) ;
#31374 = DIRECTION ( 'NONE',  ( -0.000000000000000000, 0.000000000000000000, 1.000000000000000000 ) ) ;
#31375 = DIRECTION ( 'NONE',  ( -0.9075754196709567845, -0.4198891015602652099, -7.713237663339549565E-17 ) ) ;
#31376 = LINE ( 'NONE', #4136, #27894 ) ;
#31377 = CARTESIAN_POINT ( 'NONE',  ( 1.395000000000002238, -30.28730148581174220, 16.34215476954022961 ) ) ;
#31378 = EDGE_LOOP ( 'NONE', ( #13211, #24136, #12536, #23457 ) ) ;
#31379 = MECHANICAL_DESIGN_GEOMETRIC_PRESENTATION_REPRESENTATION (  '', ( #4071 ), #8073 ) ;
#31380 = CARTESIAN_POINT ( 'NONE',  ( 0.000000000000000000, -115.0000000000000000, 0.000000000000000000 ) ) ;
#31381 = CARTESIAN_POINT ( 'NONE',  ( -32.37866696771086339, 3.290334066652078171, 68.31122994652405112 ) ) ;
#31382 = CIRCLE ( 'NONE', #29119, 7.999999999999979572 ) ;
#31383 = DIRECTION ( 'NONE',  ( -1.000000000000000000, 0.000000000000000000, -5.546364386991661285E-52 ) ) ;
#31384 = ORIENTED_EDGE ( 'NONE', *, *, #15999, .F. ) ;
#31385 = CIRCLE ( 'NONE', #703, 7.999999999999952038 ) ;
#31386 = ADVANCED_FACE ( 'NONE', ( #34863, #26660 ), #10472, .F. ) ;
#31387 = B_SPLINE_CURVE_WITH_KNOTS ( 'NONE', 3,
 ( #6822, #22866, #17191, #22331, #33710, #33894 ),
 .UNSPECIFIED., .F., .F.,
 ( 4, 2, 4 ),
 ( 2.178692865977853586E-07, 0.001873416183138251236, 0.003746614496989904633 ),
 .UNSPECIFIED. ) ;
#31388 = FACE_OUTER_BOUND ( 'NONE', #10496, .T. ) ;
#31389 = CARTESIAN_POINT ( 'NONE',  ( 0.000000000000000000, -55.00000000000000711, 0.000000000000000000 ) ) ;
#31390 = CARTESIAN_POINT ( 'NONE',  ( -0.01189939958579078194, -1.353540050145433327, -8.257405511687798239 ) ) ;
#31391 = LINE ( 'NONE', #17891, #33131 ) ;
#31393 = CARTESIAN_POINT ( 'NONE',  ( -105.3514761500790655, 5.105882603317796864, -5.493682664683364081 ) ) ;
#31392 = DIRECTION ( 'NONE',  ( 0.000000000000000000, -1.000000000000000000, 0.000000000000000000 ) ) ;
#31394 = DIRECTION ( 'NONE',  ( -0.8835120444460224931, -0.4684084406997908179, -0.000000000000000000 ) ) ;
#31395 = EDGE_LOOP ( 'NONE', ( #8273, #29091, #24089, #2735 ) ) ;
#31396 = DIRECTION ( 'NONE',  ( 0.000000000000000000, 0.000000000000000000, 1.000000000000000000 ) ) ;
#31398 = DIRECTION ( 'NONE',  ( 0.000000000000000000, 0.000000000000000000, 1.000000000000000000 ) ) ;
#31397 = DIRECTION ( 'NONE',  ( -0.000000000000000000, -0.000000000000000000, 1.000000000000000000 ) ) ;
#31399 = VERTEX_POINT ( 'NONE', #26837 ) ;
#31400 = PRODUCT_DEFINITION_SHAPE ( 'NONE', 'NONE',  #35121 ) ;
#31401 = CARTESIAN_POINT ( 'NONE',  ( -10.00000000000000000, 0.000000000000000000, 0.000000000000000000 ) ) ;
#31402 = EDGE_CURVE ( 'NONE', #23546, #6373, #26930, .T. ) ;
#31403 = ORIENTED_EDGE ( 'NONE', *, *, #19412, .T. ) ;
#31404 = VECTOR ( 'NONE', #33804, 1000.000000000000000 ) ;
#31405 = AXIS2_PLACEMENT_3D ( 'NONE', #4327, #4153, #12899 ) ;
#31406 = VECTOR ( 'NONE', #9556, 1000.000000000000000 ) ;
#31407 = VERTEX_POINT ( 'NONE', #2445 ) ;
#31408 = CARTESIAN_POINT ( 'NONE',  ( 2.765921099433440666, -11.07880054387200985, -29.04985141099774637 ) ) ;
#31409 = ORIENTED_EDGE ( 'NONE', *, *, #27436, .T. ) ;
#31410 = VERTEX_POINT ( 'NONE', #29339 ) ;
#31411 = DIRECTION ( 'NONE',  ( -1.000000000000000000, 0.000000000000000000, -5.546364386991661285E-52 ) ) ;
#31412 = EDGE_CURVE ( 'NONE', #25358, #13175, #4125, .T. ) ;
#31413 = ADVANCED_FACE ( 'NONE', ( #20799 ), #24024, .T. ) ;
#31414 = EDGE_CURVE ( 'NONE', #19961, #736, #10651, .T. ) ;
#31415 = DIRECTION ( 'NONE',  ( 0.000000000000000000, 0.000000000000000000, 1.000000000000000000 ) ) ;
#31416 = DIRECTION ( 'NONE',  ( -3.469446951953832974E-18, -1.000000000000000000, -7.888609052210116302E-31 ) ) ;
#31417 = VERTEX_POINT ( 'NONE', #1919 ) ;
#31418 = ORIENTED_EDGE ( 'NONE', *, *, #9583, .T. ) ;
#31419 = CARTESIAN_POINT ( 'NONE',  ( 19.99999999999998934, -124.9999999999999432, -186.9999999999999716 ) ) ;
#31420 = DIRECTION ( 'NONE',  ( 1.000000000000000000, 3.469446951953834515E-18, 0.000000000000000000 ) ) ;
#31421 = CARTESIAN_POINT ( 'NONE',  ( -12.00000000000001066, -28.99999999999999645, -175.0000000000000000 ) ) ;
#31422 = LINE ( 'NONE', #31086, #22121 ) ;
#31423 = LINE ( 'NONE', #23921, #11428 ) ;
#31424 = ORIENTED_EDGE ( 'NONE', *, *, #21585, .F. ) ;
#31425 = CARTESIAN_POINT ( 'NONE',  ( -29.68486519896224962, 23.49918569563710946, 68.31122994652405112 ) ) ;
#31426 = CARTESIAN_POINT ( 'NONE',  ( 0.7561992231261003283, -18.61835568386921835, -28.34776818504862916 ) ) ;
#31427 = ORIENTED_EDGE ( 'NONE', *, *, #12859, .T. ) ;
#31428 = FACE_OUTER_BOUND ( 'NONE', #3421, .T. ) ;
#31429 = CARTESIAN_POINT ( 'NONE',  ( 0.000000000000000000, 2.281310696040539424E-14, -36.68877005347592757 ) ) ;
#31430 = LINE ( 'NONE', #17935, #28003 ) ;
#31431 = ORIENTED_EDGE ( 'NONE', *, *, #10371, .T. ) ;
#31432 = VECTOR ( 'NONE', #23779, 1000.000000000000114 ) ;
#31433 = AXIS2_PLACEMENT_3D ( 'NONE', #19771, #13895, #16580 ) ;
#31434 = LINE ( 'NONE', #25208, #20089 ) ;
#31435 = ORIENTED_EDGE ( 'NONE', *, *, #11212, .F. ) ;
#31436 = CARTESIAN_POINT ( 'NONE',  ( 11.99999999999999645, 144.9999999999999716, 190.9999999999999716 ) ) ;
#31437 = DIRECTION ( 'NONE',  ( -0.000000000000000000, -0.000000000000000000, -1.000000000000000000 ) ) ;
#31438 = EDGE_LOOP ( 'NONE', ( #14116, #16308, #11843, #31916 ) ) ;
#31439 = DIRECTION ( 'NONE',  ( 2.891205793294675861E-16, 0.000000000000000000, 1.000000000000000000 ) ) ;
#31440 = FACE_OUTER_BOUND ( 'NONE', #27484, .T. ) ;
#31441 = ORIENTED_EDGE ( 'NONE', *, *, #22901, .F. ) ;
#31442 = VECTOR ( 'NONE', #6821, 1000.000000000000000 ) ;
#31443 = DIRECTION ( 'NONE',  ( -6.344477933863744788E-14, -3.676471759909360080E-14, 1.000000000000000000 ) ) ;
#31444 = EDGE_CURVE ( 'NONE', #9057, #26143, #10114, .T. ) ;
#31445 = ORIENTED_EDGE ( 'NONE', *, *, #20144, .F. ) ;
#31446 = CARTESIAN_POINT ( 'NONE',  ( 2.789999999999999591, -0.2191908000477053864, -30.66081142815918170 ) ) ;
#31447 = VERTEX_POINT ( 'NONE', #4572 ) ;
#31448 = DIRECTION ( 'NONE',  ( -1.000000000000000000, -3.469446951953834515E-18, 0.000000000000000000 ) ) ;
#31449 = EDGE_CURVE ( 'NONE', #26588, #26110, #20976, .T. ) ;
#31450 = AXIS2_PLACEMENT_3D ( 'NONE', #32527, #16369, #10129 ) ;
#31451 = FILL_AREA_STYLE_COLOUR ( '', #17020 ) ;
#31452 = EDGE_CURVE ( 'NONE', #5849, #32902, #4411, .T. ) ;
#31453 = AXIS2_PLACEMENT_3D ( 'NONE', #15784, #26615, #26262 ) ;
#31454 = CARTESIAN_POINT ( 'NONE',  ( 15.04122381213380066, 28.86114964982165887, 49.43553178847298568 ) ) ;
#31455 = DIRECTION ( 'NONE',  ( 0.000000000000000000, 0.000000000000000000, -1.000000000000000000 ) ) ;
#31456 = ITEM_DEFINED_TRANSFORMATION ( 'NONE', 'NONE', #201,  #28566 ) ;
#31457 = ORIENTED_EDGE ( 'NONE', *, *, #9824, .F. ) ;
#31458 = ORIENTED_EDGE ( 'NONE', *, *, #33292, .T. ) ;
#31459 = AXIS2_PLACEMENT_3D ( 'NONE', #32745, #32388, #8367 ) ;
#31460 = ORIENTED_EDGE ( 'NONE', *, *, #18031, .T. ) ;
#31461 = ADVANCED_FACE ( 'NONE', ( #7783 ), #32345, .F. ) ;
#31462 = CARTESIAN_POINT ( 'NONE',  ( -12.00000000000001066, 124.9999999999999716, 155.0000000000000000 ) ) ;
#31463 = CARTESIAN_POINT ( 'NONE',  ( 0.000000000000000000, 0.000000000000000000, 4.679999999999999716 ) ) ;
#31464 = DIRECTION ( 'NONE',  ( -0.000000000000000000, -1.000000000000000000, -0.000000000000000000 ) ) ;
#31465 = DIRECTION ( 'NONE',  ( 1.000000000000000000, 3.469446951953834515E-18, 0.000000000000000000 ) ) ;
#31466 = LINE ( 'NONE', #5100, #14627 ) ;
#31467 = FILL_AREA_STYLE_COLOUR ( '', #10754 ) ;
#31468 = VERTEX_POINT ( 'NONE', #10287 ) ;
#31469 = EDGE_CURVE ( 'NONE', #7139, #20721, #9943, .T. ) ;
#31470 = CARTESIAN_POINT ( 'NONE',  ( -418.0000000000000568, -105.0000000000000142, -109.9999999999999574 ) ) ;
#31471 = EDGE_CURVE ( 'NONE', #19390, #20784, #21148, .T. ) ;
#31472 = ORIENTED_EDGE ( 'NONE', *, *, #11577, .T. ) ;
#31473 = VECTOR ( 'NONE', #19210, 1000.000000000000000 ) ;
#31474 = CARTESIAN_POINT ( 'NONE',  ( 19.99999999999998934, -56.99999999999997868, 154.9999999999999716 ) ) ;
#31475 = VERTEX_POINT ( 'NONE', #17060 ) ;
#31476 = PLANE ( 'NONE',  #2384 ) ;
#31477 = CARTESIAN_POINT ( 'NONE',  ( 2.783128945346505567, 14.58967697705802813, 27.20420702726705642 ) ) ;
#31478 = AXIS2_PLACEMENT_3D ( 'NONE', #15524, #29222, #29400 ) ;
#31479 = AXIS2_PLACEMENT_3D ( 'NONE', #20206, #6823, #28893 ) ;
#31480 = VECTOR ( 'NONE', #34502, 1000.000000000000000 ) ;
#31481 = CARTESIAN_POINT ( 'NONE',  ( 0.000000000000000000, 2.281310696040539424E-14, -36.68877005347592757 ) ) ;
#31482 = CARTESIAN_POINT ( 'NONE',  ( -8.245173163873238465E-14, -0.2199561701056887975, -30.66195251245371622 ) ) ;
#31483 = FILL_AREA_STYLE ('',( #15131 ) ) ;
#31484 = ORIENTED_EDGE ( 'NONE', *, *, #21902, .F. ) ;
#31485 = ORIENTED_EDGE ( 'NONE', *, *, #27234, .T. ) ;
#31486 = CARTESIAN_POINT ( 'NONE',  ( 791.9613452821549799, 1010.137517189832579, 1753.598338701303419 ) ) ;
#31487 = EDGE_LOOP ( 'NONE', ( #13773, #28546, #30445, #3599 ) ) ;
#31488 = DIRECTION ( 'NONE',  ( 0.000000000000000000, 0.000000000000000000, -1.000000000000000000 ) ) ;
#31489 = DIRECTION ( 'NONE',  ( 3.697785493223492838E-32, 1.934419779023891545E-16, -1.000000000000000000 ) ) ;
#31490 = CARTESIAN_POINT ( 'NONE',  ( 109.2875386750028639, -3.830588487554197119, 6.455099174110775273 ) ) ;
#31491 = CONTEXT_DEPENDENT_SHAPE_REPRESENTATION ( #344, #25998 ) ;
#31492 = VERTEX_POINT ( 'NONE', #16883 ) ;
#31493 = DIRECTION ( 'NONE',  ( -3.040835319149746528E-31, -1.000000000000000000, 0.000000000000000000 ) ) ;
#31494 = LINE ( 'NONE', #12649, #12358 ) ;
#31495 = VECTOR ( 'NONE', #16596, 1000.000000000000000 ) ;
#31496 = EDGE_CURVE ( 'NONE', #28354, #21081, #5855, .T. ) ;
#31497 = VERTEX_POINT ( 'NONE', #31107 ) ;
#31499 = CARTESIAN_POINT ( 'NONE',  ( 2.719010673589308258, -3.385659728284398540, 31.51320498992184227 ) ) ;
#31498 = DIRECTION ( 'NONE',  ( 0.000000000000000000, 0.000000000000000000, 1.000000000000000000 ) ) ;
#31500 = AXIS2_PLACEMENT_3D ( 'NONE', #7338, #6648, #34060 ) ;
#31501 = ORIENTED_EDGE ( 'NONE', *, *, #21535, .F. ) ;
#31502 = ORIENTED_EDGE ( 'NONE', *, *, #29605, .T. ) ;
#31503 = EDGE_CURVE ( 'NONE', #30505, #8267, #27884, .T. ) ;
#31504 = EDGE_CURVE ( 'NONE', #26019, #4201, #13833, .T. ) ;
#31505 = TOROIDAL_SURFACE ( 'NONE', #5350, 13.00000000000000000, 1.799999999999999822 ) ;
#31506 = CARTESIAN_POINT ( 'NONE',  ( 2.789999999999999147, -31.05158812718220673, -1.559667679918931738 ) ) ;
#31507 = ORIENTED_EDGE ( 'NONE', *, *, #1881, .T. ) ;
#31508 = B_SPLINE_CURVE_WITH_KNOTS ( 'NONE', 3,
 ( #27524, #21655, #30373, #2608, #21828, #32683 ),
 .UNSPECIFIED., .F., .F.,
 ( 4, 2, 4 ),
 ( 4.404817003536901581E-07, 0.001874269606490584555, 0.003748098731280815471 ),
 .UNSPECIFIED. ) ;
#31509 = CARTESIAN_POINT ( 'NONE',  ( 0.02407890056655564992, 31.00221527374952046, 2.344426712874309260 ) ) ;
#31510 = FACE_OUTER_BOUND ( 'NONE', #15731, .T. ) ;
#31511 = ORIENTED_EDGE ( 'NONE', *, *, #8679, .T. ) ;
#31512 = DIRECTION ( 'NONE',  ( -1.000000000000000000, 0.000000000000000000, 0.000000000000000000 ) ) ;
#31513 = VERTEX_POINT ( 'NONE', #16702 ) ;
#31514 = CARTESIAN_POINT ( 'NONE',  ( 0.000000000000000000, 3.524919873834583163E-15, 68.31122994652405112 ) ) ;
#31515 = LINE ( 'NONE', #23333, #7460 ) ;
#31516 = EDGE_CURVE ( 'NONE', #14788, #17615, #19718, .T. ) ;
#31517 = CARTESIAN_POINT ( 'NONE',  ( 127.4999999999999147, 0.000000000000000000, 2.499999999999825473 ) ) ;
#31519 = DIRECTION ( 'NONE',  ( -0.000000000000000000, 1.836970198721029934E-16, -1.000000000000000000 ) ) ;
#31518 = DIRECTION ( 'NONE',  ( 1.000000000000000000, 0.000000000000000000, -1.300283923313630633E-47 ) ) ;
#31520 = CIRCLE ( 'NONE', #5917, 7.999999999999979572 ) ;
#31521 = DIRECTION ( 'NONE',  ( 0.000000000000000000, 0.000000000000000000, 1.000000000000000000 ) ) ;
#31522 = CARTESIAN_POINT ( 'NONE',  ( 0.8377008405913507483, 14.95094041744785152, -1.104211576045294407 ) ) ;
#31523 = CARTESIAN_POINT ( 'NONE',  ( 0.5248941635506316761, -9.574141296992504380, 31.97728166840266439 ) ) ;
#31524 = VECTOR ( 'NONE', #18531, 1000.000000000000000 ) ;
#31525 = DIRECTION ( 'NONE',  ( 0.000000000000000000, 0.000000000000000000, -1.000000000000000000 ) ) ;
#31526 = ADVANCED_FACE ( 'NONE', ( #11529 ), #3149, .F. ) ;
#31528 = ORIENTED_EDGE ( 'NONE', *, *, #31496, .F. ) ;
#31527 = AXIS2_PLACEMENT_3D ( 'NONE', #24944, #578, #6072 ) ;
#31529 = EDGE_CURVE ( 'NONE', #27991, #26941, #3328, .T. ) ;
#31530 = ORIENTED_EDGE ( 'NONE', *, *, #17337, .F. ) ;
#31531 = ORIENTED_EDGE ( 'NONE', *, *, #34880, .F. ) ;
#31532 = PLANE ( 'NONE',  #14784 ) ;
#31533 = ORIENTED_EDGE ( 'NONE', *, *, #35018, .F. ) ;
#31534 = VERTEX_POINT ( 'NONE', #135 ) ;
#31535 = ORIENTED_EDGE ( 'NONE', *, *, #24185, .F. ) ;
#31536 = CARTESIAN_POINT ( 'NONE',  ( -130.6469666100234406, 6.000000000000000000, -62.49999999999999289 ) ) ;
#31537 = CONTEXT_DEPENDENT_SHAPE_REPRESENTATION ( #17665, #7586 ) ;
#31538 = AXIS2_PLACEMENT_3D ( 'NONE', #21033, #7671, #34928 ) ;
#31539 = ORIENTED_EDGE ( 'NONE', *, *, #17226, .T. ) ;
#31540 = FACE_OUTER_BOUND ( 'NONE', #30411, .T. ) ;
#31541 = CARTESIAN_POINT ( 'NONE',  ( -1.625000000000000000, 2.702098422956710877, 5.429999999999999716 ) ) ;
#31542 = VERTEX_POINT ( 'NONE', #22029 ) ;
#31543 = ORIENTED_EDGE ( 'NONE', *, *, #13301, .F. ) ;
#31544 = EDGE_CURVE ( 'NONE', #7548, #24819, #32871, .T. ) ;
#31545 = EDGE_CURVE ( 'NONE', #10504, #29101, #25762, .T. ) ;
#31546 = LINE ( 'NONE', #9497, #25916 ) ;
#31547 = PLANE ( 'NONE',  #10680 ) ;
#31548 = CARTESIAN_POINT ( 'NONE',  ( 1.532562817202168137, 33.69708579775584667, 49.43553178847298568 ) ) ;
#31549 = EDGE_CURVE ( 'NONE', #26511, #20630, #8667, .T. ) ;
#31550 = CARTESIAN_POINT ( 'NONE',  ( 1.395000000000002238, 22.14447232807545163, -26.34405054495533349 ) ) ;
#31551 = DIRECTION ( 'NONE',  ( 1.000000000000000000, 0.000000000000000000, 0.000000000000000000 ) ) ;
#31552 = ORIENTED_EDGE ( 'NONE', *, *, #4993, .F. ) ;
#31553 = DIRECTION ( 'NONE',  ( 1.000000000000000000, 0.000000000000000000, 0.000000000000000000 ) ) ;
#31554 = CARTESIAN_POINT ( 'NONE',  ( -418.0000000000000000, -105.0000000000000142, 194.9999999999999716 ) ) ;
#31555 = VECTOR ( 'NONE', #24165, 1000.000000000000000 ) ;
#31556 = FACE_OUTER_BOUND ( 'NONE', #27239, .T. ) ;
#31557 = ORIENTED_EDGE ( 'NONE', *, *, #5856, .F. ) ;
#31558 = CIRCLE ( 'NONE', #14539, 14.77500000000000036 ) ;
#31559 = CARTESIAN_POINT ( 'NONE',  ( 1.205771365940050410, 15.58845726811990495, 1.140844902514640588E-16 ) ) ;
#31560 = CARTESIAN_POINT ( 'NONE',  ( -35.00000000000000000, 3.353962854566122864, 15.81122994652406355 ) ) ;
#31561 = CARTESIAN_POINT ( 'NONE',  ( 104.6072996318409736, 5.728044018051756225, -4.841538128164400767 ) ) ;
#31563 = CARTESIAN_POINT ( 'NONE',  ( -107.5866028038673932, 4.424631548980197948, -6.059743929710635690 ) ) ;
#31562 = LINE ( 'NONE', #26213, #9908 ) ;
#31564 = CARTESIAN_POINT ( 'NONE',  ( 2.604019713477800035, 25.38927130757801010, -19.93727243998111476 ) ) ;
#31565 = ORIENTED_EDGE ( 'NONE', *, *, #23235, .T. ) ;
#31566 = CARTESIAN_POINT ( 'NONE',  ( 107.5624465017048550, 5.148005685260259590, -11.39183432441182653 ) ) ;
#31568 = CARTESIAN_POINT ( 'NONE',  ( -500.0000000000000000, -105.0000000000000142, 187.0000000000000000 ) ) ;
#31567 = DIRECTION ( 'NONE',  ( 0.000000000000000000, 1.836970198721029688E-16, -1.000000000000000000 ) ) ;
#31569 = EDGE_CURVE ( 'NONE', #26932, #23700, #10422, .T. ) ;
#31570 = EDGE_CURVE ( 'NONE', #21613, #7363, #30569, .T. ) ;
#31571 = VECTOR ( 'NONE', #21652, 1000.000000000000000 ) ;
#31572 = ORIENTED_EDGE ( 'NONE', *, *, #28692, .T. ) ;
#31573 = DIRECTION ( 'NONE',  ( 0.000000000000000000, 1.000000000000000000, 1.224646799147353207E-16 ) ) ;
#31574 = VECTOR ( 'NONE', #28884, 1000.000000000000000 ) ;
#31575 = ADVANCED_FACE ( 'NONE', ( #666 ), #21667, .T. ) ;
#31576 = ORIENTED_EDGE ( 'NONE', *, *, #373, .T. ) ;
#31577 = EDGE_CURVE ( 'NONE', #2811, #6643, #187, .T. ) ;
#31578 = ADVANCED_FACE ( 'NONE', ( #27710, #33226 ), #14386, .T. ) ;
#31579 = ORIENTED_EDGE ( 'NONE', *, *, #5750, .F. ) ;
#31580 = CARTESIAN_POINT ( 'NONE',  ( -361.0000000000000000, -125.0000000000000284, 112.0000000000000000 ) ) ;
#31581 = EDGE_LOOP ( 'NONE', ( #34378, #18011, #27676, #8743, #17352, #11179, #25444 ) ) ;
#31582 = ORIENTED_EDGE ( 'NONE', *, *, #23047, .T. ) ;
#31583 = CARTESIAN_POINT ( 'NONE',  ( -442.0000000000000000, 104.9999999999999858, -162.9999999999999716 ) ) ;
#31584 = VECTOR ( 'NONE', #19812, 1000.000000000000000 ) ;
#31585 = DIRECTION ( 'NONE',  ( 0.000000000000000000, -1.000000000000000000, 0.000000000000000000 ) ) ;
#31586 = CARTESIAN_POINT ( 'NONE',  ( 1.040000000000000924, 0.000000000000000000, 0.000000000000000000 ) ) ;
#31587 = ORIENTED_EDGE ( 'NONE', *, *, #14620, .F. ) ;
#31588 = ORIENTED_EDGE ( 'NONE', *, *, #21125, .F. ) ;
#31589 = CARTESIAN_POINT ( 'NONE',  ( 11.99999999999999645, -55.00000000000002132, 155.0000000000000000 ) ) ;
#31590 = DIRECTION ( 'NONE',  ( 0.000000000000000000, -0.000000000000000000, 1.000000000000000000 ) ) ;
#31591 = CARTESIAN_POINT ( 'NONE',  ( -105.0000000000000000, 0.000000000000000000, -57.49999999999999289 ) ) ;
#31592 = FACE_BOUND ( 'NONE', #24966, .T. ) ;
#31593 = CARTESIAN_POINT ( 'NONE',  ( -418.0000000000000000, -104.9999999999999716, -190.9999999999999716 ) ) ;
#31594 = ORIENTED_EDGE ( 'NONE', *, *, #10363, .T. ) ;
#31595 = ORIENTED_EDGE ( 'NONE', *, *, #29364, .F. ) ;
#31596 = CIRCLE ( 'NONE', #16273, 2.033421858999711951 ) ;
#31597 = LINE ( 'NONE', #25555, #32133 ) ;
#31598 = CARTESIAN_POINT ( 'NONE',  ( -5.018880456227426877E-16, -21.14855567236476119, 22.20072382163045077 ) ) ;
#31599 = ORIENTED_EDGE ( 'NONE', *, *, #6897, .F. ) ;
#31600 = ADVANCED_FACE ( 'NONE', ( #19197 ), #19021, .T. ) ;
#31601 = CARTESIAN_POINT ( 'NONE',  ( 0.1859802940384192305, 31.85364232850768218, 5.239790278973186055 ) ) ;
#31602 = DIRECTION ( 'NONE',  ( 0.000000000000000000, 0.000000000000000000, -1.000000000000000000 ) ) ;
#31603 = FACE_OUTER_BOUND ( 'NONE', #21301, .T. ) ;
#31604 = ORIENTED_EDGE ( 'NONE', *, *, #20665, .T. ) ;
#31605 = LINE ( 'NONE', #26441, #31432 ) ;
#31606 = ORIENTED_EDGE ( 'NONE', *, *, #34508, .T. ) ;
#31608 = LINE ( 'NONE', #1714, #25355 ) ;
#31607 = DIRECTION ( 'NONE',  ( 0.000000000000000000, 0.000000000000000000, -1.000000000000000000 ) ) ;
#31610 = AXIS2_PLACEMENT_3D ( 'NONE', #29115, #18279, #10251 ) ;
#31609 = CARTESIAN_POINT ( 'NONE',  ( -18.07349068442141515, -27.06572199953722446, 68.31122994652405112 ) ) ;
#31611 = EDGE_CURVE ( 'NONE', #13324, #29345, #34875, .T. ) ;
#31612 = EDGE_CURVE ( 'NONE', #6974, #28627, #2970, .T. ) ;
#31613 = EDGE_CURVE ( 'NONE', #18651, #7619, #12064, .T. ) ;
#31614 = ORIENTED_EDGE ( 'NONE', *, *, #25788, .T. ) ;
#31615 = CARTESIAN_POINT ( 'NONE',  ( 1.394999999999999574, -25.27164158951551087, -23.36088151536946000 ) ) ;
#31616 = DIRECTION ( 'NONE',  ( 0.000000000000000000, 1.000000000000000000, 5.145227585319922065E-49 ) ) ;
#31617 = ORIENTED_EDGE ( 'NONE', *, *, #5078, .T. ) ;
#31618 = VECTOR ( 'NONE', #11962, 999.9999999999998863 ) ;
#31619 = DIRECTION ( 'NONE',  ( -7.556845695699624510E-14, -1.801457373381261100E-14, 1.000000000000000000 ) ) ;
#31620 = VERTEX_POINT ( 'NONE', #6339 ) ;
#31621 = CARTESIAN_POINT ( 'NONE',  ( 106.5040163601712351, -5.550599894338584583, 11.20035359757823912 ) ) ;
#31622 = VERTEX_POINT ( 'NONE', #31261 ) ;
#31623 = CIRCLE ( 'NONE', #19072, 22.50000000000000355 ) ;
#31624 = CARTESIAN_POINT ( 'NONE',  ( -3.250000000000000000, 5.404196845913421754, -0.7500000000000000000 ) ) ;
#31625 = DIRECTION ( 'NONE',  ( 0.000000000000000000, 1.000000000000000000, 5.053935297177146739E-49 ) ) ;
#31626 = CARTESIAN_POINT ( 'NONE',  ( -103.3138017543800373, -4.840385614786930191, -5.731315639859864142 ) ) ;
#31627 = CARTESIAN_POINT ( 'NONE',  ( 0.5288002541271116241, 33.21438043751174973, -3.418204286533154335 ) ) ;
#31628 = ORIENTED_EDGE ( 'NONE', *, *, #13498, .F. ) ;
#31629 = ORIENTED_EDGE ( 'NONE', *, *, #5915, .T. ) ;
#31630 = VERTEX_POINT ( 'NONE', #17241 ) ;
#31631 =( GEOMETRIC_REPRESENTATION_CONTEXT ( 3 ) GLOBAL_UNCERTAINTY_ASSIGNED_CONTEXT ( ( #20916 ) ) GLOBAL_UNIT_ASSIGNED_CONTEXT ( ( #5764, #16662, #26973 ) ) REPRESENTATION_CONTEXT ( 'NONE', 'WORKASPACE' ) );
#31632 = LINE ( 'NONE', #18143, #19446 ) ;
#31633 = CARTESIAN_POINT ( 'NONE',  ( -418.0000000000000568, -109.0000000000000142, -155.0000000000000000 ) ) ;
#31634 = FACE_OUTER_BOUND ( 'NONE', #30782, .T. ) ;
#31635 = DIRECTION ( 'NONE',  ( 0.000000000000000000, 0.000000000000000000, -1.000000000000000000 ) ) ;
#31636 = FACE_OUTER_BOUND ( 'NONE', #4427, .T. ) ;
#31637 = ORIENTED_EDGE ( 'NONE', *, *, #13818, .F. ) ;
#31638 = PRODUCT_DEFINITION_SHAPE ( 'NONE', 'NONE',  #35175 ) ;
#31639 = CARTESIAN_POINT ( 'NONE',  ( 1.155000000000000027, 1.414467053015192904E-16, 3.931000000000000494 ) ) ;
#31640 = CARTESIAN_POINT ( 'NONE',  ( 0.006871126357153574046, -15.15173253686488053, -26.89521541643909330 ) ) ;
#31641 = DIRECTION ( 'NONE',  ( 0.000000000000000000, 6.123233995736766036E-17, 1.000000000000000000 ) ) ;
#31642 = ORIENTED_EDGE ( 'NONE', *, *, #20455, .F. ) ;
#31643 = DIRECTION ( 'NONE',  ( -1.000000000000000000, -0.000000000000000000, -0.000000000000000000 ) ) ;
#31644 = ORIENTED_EDGE ( 'NONE', *, *, #1015, .T. ) ;
#31645 = DIRECTION ( 'NONE',  ( 0.000000000000000000, 1.836970198721029934E-16, -1.000000000000000000 ) ) ;
#31646 = EDGE_CURVE ( 'NONE', #493, #22138, #17938, .T. ) ;
#31647 = PLANE ( 'NONE',  #11036 ) ;
#31648 = EDGE_CURVE ( 'NONE', #22205, #11568, #20075, .T. ) ;
#31649 = FACE_OUTER_BOUND ( 'NONE', #10610, .T. ) ;
#31650 = VECTOR ( 'NONE', #30182, 1000.000000000000000 ) ;
#31651 = CARTESIAN_POINT ( 'NONE',  ( -32.32899628990712415, -3.747048406849347035, -36.68877005347593467 ) ) ;
#31653 = ADVANCED_FACE ( 'NONE', ( #25926 ), #6861, .F. ) ;
#31652 = PLANE ( 'NONE',  #9781 ) ;
#31654 = ORIENTED_EDGE ( 'NONE', *, *, #21108, .T. ) ;
#31655 = EDGE_LOOP ( 'NONE', ( #13298, #20544, #14767, #20917 ) ) ;
#31656 = DIRECTION ( 'NONE',  ( -7.893605728314050488E-14, 1.618803117314786135E-15, 0.9999999999999998890 ) ) ;
#31657 = ORIENTED_EDGE ( 'NONE', *, *, #31784, .T. ) ;
#31658 = EDGE_CURVE ( 'NONE', #24529, #15307, #28423, .T. ) ;
#31659 = CARTESIAN_POINT ( 'NONE',  ( 8.927936315454026328, -31.29690601358700519, 68.31122994652405112 ) ) ;
#31660 = CIRCLE ( 'NONE', #26562, 14.20000000000000107 ) ;
#31661 = AXIS2_PLACEMENT_3D ( 'NONE', #6240, #20324, #28503 ) ;
#31662 = LINE ( 'NONE', #33334, #9916 ) ;
#31663 = CARTESIAN_POINT ( 'NONE',  ( 99.31309745116723775, -0.7897130297925551989, 7.460902677354920520 ) ) ;
#31664 = ORIENTED_EDGE ( 'NONE', *, *, #32523, .T. ) ;
#31665 = CARTESIAN_POINT ( 'NONE',  ( -361.0000000000000000, 134.9999999999999716, 112.0000000000000000 ) ) ;
#31666 = VECTOR ( 'NONE', #21488, 1000.000000000000114 ) ;
#31668 = DIRECTION ( 'NONE',  ( -0.000000000000000000, 0.000000000000000000, 1.000000000000000000 ) ) ;
#31667 = DIRECTION ( 'NONE',  ( -1.000000000000000000, 0.000000000000000000, 0.000000000000000000 ) ) ;
#31669 = ORIENTED_EDGE ( 'NONE', *, *, #18983, .T. ) ;
#31670 = VERTEX_POINT ( 'NONE', #3672 ) ;
#31671 = LINE ( 'NONE', #15685, #1547 ) ;
#31672 = ORIENTED_EDGE ( 'NONE', *, *, #26429, .T. ) ;
#31673 = PLANE ( 'NONE',  #30115 ) ;
#31674 = CARTESIAN_POINT ( 'NONE',  ( 0.000000000000000000, -20.92506858792743785, -22.14933852381697932 ) ) ;
#31675 = ORIENTED_EDGE ( 'NONE', *, *, #2514, .T. ) ;
#31676 = DIRECTION ( 'NONE',  ( -0.000000000000000000, -0.000000000000000000, 1.000000000000000000 ) ) ;
#31677 = CIRCLE ( 'NONE', #16368, 2.000000000000001776 ) ;
#31678 = PRODUCT_DEFINITION_SHAPE ( 'NONE', 'NONE',  #35126 ) ;
#31679 = ORIENTED_EDGE ( 'NONE', *, *, #22948, .T. ) ;
#31680 = DIRECTION ( 'NONE',  ( 1.000000000000000000, 3.469446951953834515E-18, 0.000000000000000000 ) ) ;
#31681 =( NAMED_UNIT ( * ) SI_UNIT ( $, .STERADIAN. ) SOLID_ANGLE_UNIT ( ) );
#31682 = EDGE_CURVE ( 'NONE', #19198, #12986, #17588, .T. ) ;
#31683 = CARTESIAN_POINT ( 'NONE',  ( 35.44043929807611448, -12.65143121711728291, 5.690671783530174999 ) ) ;
#31685 = DIRECTION ( 'NONE',  ( -1.000000000000000000, 0.000000000000000000, 0.000000000000000000 ) ) ;
#31684 = FACE_OUTER_BOUND ( 'NONE', #7200, .T. ) ;
#31686 = VECTOR ( 'NONE', #32423, 1000.000000000000000 ) ;
#31687 = VECTOR ( 'NONE', #27337, 1000.000000000000000 ) ;
#31688 = CARTESIAN_POINT ( 'NONE',  ( 0.000000000000000000, 0.000000000000000000, 4.679999999999999716 ) ) ;
#31689 = CARTESIAN_POINT ( 'NONE',  ( -5.021133111224782120, 14.09580098603202813, -87.50000000000000000 ) ) ;
#31690 = DIRECTION ( 'NONE',  ( 0.000000000000000000, 0.000000000000000000, -1.000000000000000000 ) ) ;
#31692 = ADVANCED_FACE ( 'NONE', ( #14560 ), #28766, .T. ) ;
#31691 = CARTESIAN_POINT ( 'NONE',  ( -445.9999999999999432, -125.0000000000000000, 162.9999999999999716 ) ) ;
#31693 = EDGE_CURVE ( 'NONE', #13074, #9444, #30305, .T. ) ;
#31694 = AXIS2_PLACEMENT_3D ( 'NONE', #13437, #2046, #10230 ) ;
#31695 = VERTEX_POINT ( 'NONE', #4366 ) ;
#31696 = ADVANCED_FACE ( 'NONE', ( #25744, #17420 ), #23093, .F. ) ;
#31697 = EDGE_CURVE ( 'NONE', #26094, #26996, #28246, .T. ) ;
#31698 = ORIENTED_EDGE ( 'NONE', *, *, #23740, .T. ) ;
#31699 = ORIENTED_EDGE ( 'NONE', *, *, #14084, .F. ) ;
#31700 = EDGE_CURVE ( 'NONE', #21389, #11399, #32562, .T. ) ;
#31701 = AXIS2_PLACEMENT_3D ( 'NONE', #26945, #70, #24265 ) ;
#31702 = PLANE ( 'NONE',  #3418 ) ;
#31703 = EDGE_LOOP ( 'NONE', ( #34318, #7974, #3308, #17442 ) ) ;
#31704 = VERTEX_POINT ( 'NONE', #23262 ) ;
#31705 = ORIENTED_EDGE ( 'NONE', *, *, #12622, .T. ) ;
#31706 = CARTESIAN_POINT ( 'NONE',  ( -442.0000000000000000, -125.0000000000000000, 190.9999999999999716 ) ) ;
#31707 = ITEM_DEFINED_TRANSFORMATION ( 'NONE', 'NONE', #24073,  #28566 ) ;
#31708 = AXIS2_PLACEMENT_3D ( 'NONE', #35076, #24197, #13186 ) ;
#31709 = AXIS2_PLACEMENT_3D ( 'NONE', #11013, #5302, #21164 ) ;
#31710 = ORIENTED_EDGE ( 'NONE', *, *, #872, .F. ) ;
#31711 = CARTESIAN_POINT ( 'NONE',  ( 2.783107610007986121, 14.58972988903205525, -27.20448975989763696 ) ) ;
#31712 = CARTESIAN_POINT ( 'NONE',  ( 0.000000000000000000, -49.99999999999999289, 0.000000000000000000 ) ) ;
#31713 = ORIENTED_EDGE ( 'NONE', *, *, #17853, .F. ) ;
#31714 = ORIENTED_EDGE ( 'NONE', *, *, #16566, .T. ) ;
#31715 =( REPRESENTATION_RELATIONSHIP ('NONE','NONE', #23037, #28231 ) REPRESENTATION_RELATIONSHIP_WITH_TRANSFORMATION ( #11641 )SHAPE_REPRESENTATION_RELATIONSHIP( ) );
#31716 = DIRECTION ( 'NONE',  ( 0.000000000000000000, -1.000000000000000000, 0.000000000000000000 ) ) ;
#31717 = CARTESIAN_POINT ( 'NONE',  ( -19.99999999999998934, -137.0000000000000000, 159.0000000000000000 ) ) ;
#31718 = CARTESIAN_POINT ( 'NONE',  ( 0.000000000000000000, 0.000000000000000000, 4.679999999999999716 ) ) ;
#31719 = FACE_OUTER_BOUND ( 'NONE', #22043, .T. ) ;
#31720 = CARTESIAN_POINT ( 'NONE',  ( 0.000000000000000000, 28.95078156989558948, 9.502838467758177643 ) ) ;
#31721 = ORIENTED_EDGE ( 'NONE', *, *, #20488, .F. ) ;
#31722 = VECTOR ( 'NONE', #28100, 1000.000000000000000 ) ;
#31723 = PLANE ( 'NONE',  #28277 ) ;
#31724 = CARTESIAN_POINT ( 'NONE',  ( 28.23027531293552528, -17.65143121711728469, 0.000000000000000000 ) ) ;
#31725 = ORIENTED_EDGE ( 'NONE', *, *, #13986, .F. ) ;
#31726 = CARTESIAN_POINT ( 'NONE',  ( -5.210000000000000853, 0.000000000000000000, 0.000000000000000000 ) ) ;
#31727 = CARTESIAN_POINT ( 'NONE',  ( 11.99999999999999645, 144.9999999999999716, -186.9999999999999716 ) ) ;
#31728 = TOROIDAL_SURFACE ( 'NONE', #11941, 30.47050528711512030, 8.000000000000000000 ) ;
#31729 = CARTESIAN_POINT ( 'NONE',  ( 107.0789465421990201, 5.351410369513340370, -5.255735268165820706 ) ) ;
#31731 = CARTESIAN_POINT ( 'NONE',  ( 8.000000000000000000, 0.000000000000000000, 0.000000000000000000 ) ) ;
#31730 = CARTESIAN_POINT ( 'NONE',  ( -143.0000000000000568, -87.50000000000000000, 65.00000000000000000 ) ) ;
#31732 = AXIS2_PLACEMENT_3D ( 'NONE', #3748, #915, #33473 ) ;
#31733 = FACE_OUTER_BOUND ( 'NONE', #32807, .T. ) ;
#31734 = ORIENTED_EDGE ( 'NONE', *, *, #20775, .F. ) ;
#31735 = CARTESIAN_POINT ( 'NONE',  ( 106.5032006809128546, 5.550581019792740989, -11.20035861729703797 ) ) ;
#31736 = LINE ( 'NONE', #1672, #953 ) ;
#31737 = AXIS2_PLACEMENT_3D ( 'NONE', #20267, #34478, #7060 ) ;
#31738 = VERTEX_POINT ( 'NONE', #33935 ) ;
#31739 = ADVANCED_FACE ( 'NONE', ( #25563 ), #1188, .T. ) ;
#31740 = EDGE_CURVE ( 'NONE', #31336, #30159, #17756, .T. ) ;
#31741 = LINE ( 'NONE', #33585, #1278 ) ;
#31742 = EDGE_LOOP ( 'NONE', ( #16587, #23801, #33642, #7026, #27381, #823, #5941, #15267 ) ) ;
#31743 = VECTOR ( 'NONE', #28239, 1000.000000000000000 ) ;
#31744 = EDGE_LOOP ( 'NONE', ( #20252, #11993, #7860, #8954 ) ) ;
#31745 = CARTESIAN_POINT ( 'NONE',  ( 12.46788440507149964, 30.06253867087536946, 68.31122994652405112 ) ) ;
#31746 = ORIENTED_EDGE ( 'NONE', *, *, #34140, .T. ) ;
#31747 = ORIENTED_EDGE ( 'NONE', *, *, #14919, .T. ) ;
#31748 = B_SPLINE_CURVE_WITH_KNOTS ( 'NONE', 3,
 ( #12111, #25967, #28985, #7258, #34145, #9604 ),
 .UNSPECIFIED., .F., .F.,
 ( 4, 2, 4 ),
 ( 4.404817204574324437E-07, 0.001874269756547609737, 0.003748099031374762125 ),
 .UNSPECIFIED. ) ;
#31749 = CARTESIAN_POINT ( 'NONE',  ( 1.040000000000002034, 34.17636915695680244, 4.045051921974835096 ) ) ;
#31750 = EDGE_CURVE ( 'NONE', #27819, #18126, #31434, .T. ) ;
#31751 = VECTOR ( 'NONE', #29713, 1000.000000000000114 ) ;
#31752 = CARTESIAN_POINT ( 'NONE',  ( 10.96230482721425403, -12.47301499840863848, -87.50000000000000000 ) ) ;
#31753 = LINE ( 'NONE', #7018, #33605 ) ;
#31754 = ORIENTED_EDGE ( 'NONE', *, *, #11866, .F. ) ;
#31755 = VERTEX_POINT ( 'NONE', #33404 ) ;
#31756 = DIRECTION ( 'NONE',  ( -1.000000000000000000, -0.000000000000000000, -0.000000000000000000 ) ) ;
#31757 = LINE ( 'NONE', #16423, #11819 ) ;
#31758 = CARTESIAN_POINT ( 'NONE',  ( 4.815661544189684840, -32.18716788982705168, 68.31122994652405112 ) ) ;
#31759 = ADVANCED_FACE ( 'NONE', ( #9026 ), #19895, .T. ) ;
#31760 = CARTESIAN_POINT ( 'NONE',  ( 143.0000000000000568, 85.49999999999998579, 65.00000000000000000 ) ) ;
#31761 = CARTESIAN_POINT ( 'NONE',  ( -365.0000000000000000, 134.9999999999999716, 113.9999999999999716 ) ) ;
#31762 = EDGE_LOOP ( 'NONE', ( #4962, #18514, #26306, #23445 ) ) ;
#31763 = EDGE_CURVE ( 'NONE', #19439, #29430, #12142, .T. ) ;
#31764 = EDGE_LOOP ( 'NONE', ( #19719, #23541, #24961, #8287 ) ) ;
#31765 = AXIS2_PLACEMENT_3D ( 'NONE', #22357, #33204, #27861 ) ;
#31766 = ADVANCED_FACE ( 'NONE', ( #7211 ), #34637, .F. ) ;
#31767 = DIRECTION ( 'NONE',  ( 0.000000000000000000, -1.000000000000000000, 6.123233995736766036E-17 ) ) ;
#31768 = DIRECTION ( 'NONE',  ( 0.000000000000000000, 2.309213040847544338E-50, 1.000000000000000000 ) ) ;
#31769 = ORIENTED_EDGE ( 'NONE', *, *, #8635, .F. ) ;
#31770 = DIRECTION ( 'NONE',  ( 0.000000000000000000, 0.000000000000000000, -1.000000000000000000 ) ) ;
#31771 = ADVANCED_FACE ( 'NONE', ( #7386 ), #18275, .F. ) ;
#31772 = DIRECTION ( 'NONE',  ( 0.000000000000000000, -1.000000000000000000, 1.310824597558155437E-49 ) ) ;
#31773 = DIRECTION ( 'NONE',  ( 0.000000000000000000, 1.000000000000000000, 0.000000000000000000 ) ) ;
#31774 = VERTEX_POINT ( 'NONE', #15257 ) ;
#31775 = CIRCLE ( 'NONE', #17049, 2.000000000000001776 ) ;
#31776 = DIRECTION ( 'NONE',  ( -0.000000000000000000, -1.836970198721029688E-16, 1.000000000000000000 ) ) ;
#31777 = ORIENTED_EDGE ( 'NONE', *, *, #10574, .T. ) ;
#31778 = DIRECTION ( 'NONE',  ( -1.000000000000000000, -0.000000000000000000, -0.000000000000000000 ) ) ;
#31779 = ORIENTED_EDGE ( 'NONE', *, *, #32605, .T. ) ;
#31781 = CARTESIAN_POINT ( 'NONE',  ( 0.000000000000000000, 3.524919873834583163E-15, 68.31122994652405112 ) ) ;
#31780 = DIRECTION ( 'NONE',  ( 1.000000000000000000, 0.000000000000000000, 0.000000000000000000 ) ) ;
#31782 = VECTOR ( 'NONE', #26907, 1000.000000000000000 ) ;
#31783 = EDGE_LOOP ( 'NONE', ( #3341, #17310, #11024, #2622 ) ) ;
#31784 = EDGE_CURVE ( 'NONE', #7014, #31468, #17836, .T. ) ;
#31785 = CARTESIAN_POINT ( 'NONE',  ( -365.0000000000000000, 124.9999999999999432, 168.9999999999999716 ) ) ;
#31786 = B_SPLINE_CURVE_WITH_KNOTS ( 'NONE', 3,
 ( #11692, #3657, #17044, #27692, #22544, #33388 ),
 .UNSPECIFIED., .F., .F.,
 ( 4, 2, 4 ),
 ( 4.404817080791679206E-07, 0.001874269664496251448, 0.003748098847284423666 ),
 .UNSPECIFIED. ) ;
#31787 = CARTESIAN_POINT ( 'NONE',  ( 2.765921099433441999, -15.32140196853772984, 27.05343472112986092 ) ) ;
#31788 = ORIENTED_EDGE ( 'NONE', *, *, #27270, .F. ) ;
#31789 = COLOUR_RGB ( '',0.7921568627450980005, 0.8196078431372548767, 0.9333333333333333481 ) ;
#31790 = CARTESIAN_POINT ( 'NONE',  ( 758.3567813432772482, 1352.575784968245216, 1753.598338701303419 ) ) ;
#31791 = EDGE_LOOP ( 'NONE', ( #34302, #21731 ) ) ;
#31792 = DIRECTION ( 'NONE',  ( 1.000000000000000000, 0.000000000000000000, -0.000000000000000000 ) ) ;
#31793 = VERTEX_POINT ( 'NONE', #12935 ) ;
#31794 = CARTESIAN_POINT ( 'NONE',  ( 8.000000000000003553, 1.261386203121773722E-15, 10.30000000000000071 ) ) ;
#31795 = VECTOR ( 'NONE', #9040, 1000.000000000000000 ) ;
#31796 = CYLINDRICAL_SURFACE ( 'NONE', #25490, 7.999999999999979572 ) ;
#31797 = DIRECTION ( 'NONE',  ( 0.000000000000000000, 0.000000000000000000, -1.000000000000000000 ) ) ;
#31798 = CARTESIAN_POINT ( 'NONE',  ( -349.0000000000000000, -125.0000000000000284, 185.0000000000000000 ) ) ;
#31799 = VERTEX_POINT ( 'NONE', #15426 ) ;
#31800 = ORIENTED_EDGE ( 'NONE', *, *, #18264, .F. ) ;
#31801 = ORIENTED_EDGE ( 'NONE', *, *, #11866, .T. ) ;
#31802 = CARTESIAN_POINT ( 'NONE',  ( -20.00000000000007461, 144.9999999999999716, 187.0000000000000000 ) ) ;
#31803 = CARTESIAN_POINT ( 'NONE',  ( -9.978866888775426602, 16.12922284503173742, -67.50000000000000000 ) ) ;
#31804 = EDGE_CURVE ( 'NONE', #3430, #31033, #4531, .T. ) ;
#31805 = EDGE_CURVE ( 'NONE', #1194, #19968, #34814, .T. ) ;
#31806 = PLANE ( 'NONE',  #23027 ) ;
#31807 = AXIS2_PLACEMENT_3D ( 'NONE', #3048, #13920, #24762 ) ;
#31808 = PLANE ( 'NONE',  #9764 ) ;
#31809 = CARTESIAN_POINT ( 'NONE',  ( -12.00000000000001066, -145.0000000000000000, 162.9999999999999716 ) ) ;
#31810 = ORIENTED_EDGE ( 'NONE', *, *, #20729, .F. ) ;
#31811 = DIRECTION ( 'NONE',  ( 0.000000000000000000, 1.000000000000000000, 0.000000000000000000 ) ) ;
#31812 = DIRECTION ( 'NONE',  ( -1.000000000000000000, 0.000000000000000000, 0.000000000000000000 ) ) ;
#31813 = DIRECTION ( 'NONE',  ( -1.000000000000000000, -0.000000000000000000, -0.000000000000000000 ) ) ;
#31814 = EDGE_LOOP ( 'NONE', ( #11362, #12242, #24492, #30485 ) ) ;
#31815 = DIRECTION ( 'NONE',  ( 0.000000000000000000, 1.000000000000000000, 0.000000000000000000 ) ) ;
#31816 = ORIENTED_EDGE ( 'NONE', *, *, #31611, .T. ) ;
#31817 = DIRECTION ( 'NONE',  ( 0.000000000000000000, 0.000000000000000000, 1.000000000000000000 ) ) ;
#31818 = DIRECTION ( 'NONE',  ( 0.000000000000000000, -1.000000000000000000, 5.145227585319922065E-49 ) ) ;
#31819 = CONICAL_SURFACE ( 'NONE', #5667, 32.54542015209054995, 1.389864428407444175 ) ;
#31820 = ORIENTED_EDGE ( 'NONE', *, *, #17772, .T. ) ;
#31821 = CARTESIAN_POINT ( 'NONE',  ( -20.00000000000004619, -137.0000000000000000, -190.9999999999999716 ) ) ;
#31822 = DIRECTION ( 'NONE',  ( 0.000000000000000000, -1.000000000000000000, 6.123233995736766036E-17 ) ) ;
#31823 = DIRECTION ( 'NONE',  ( 1.000000000000000000, 0.000000000000000000, -0.000000000000000000 ) ) ;
#31824 = ORIENTED_EDGE ( 'NONE', *, *, #17870, .F. ) ;
#31825 = ORIENTED_EDGE ( 'NONE', *, *, #25543, .T. ) ;
#31826 = DIRECTION ( 'NONE',  ( -0.1063910735369017202, 0.9943243633099136947, -1.000770725407181676E-14 ) ) ;
#31827 = ORIENTED_EDGE ( 'NONE', *, *, #12660, .F. ) ;
#31828 = CARTESIAN_POINT ( 'NONE',  ( 1.991296462759137853, -32.48444414290483451, 68.31122994652405112 ) ) ;
#31829 = DIRECTION ( 'NONE',  ( 0.000000000000000000, 0.000000000000000000, 1.000000000000000000 ) ) ;
#31830 = DIRECTION ( 'NONE',  ( 0.000000000000000000, 0.000000000000000000, 1.000000000000000000 ) ) ;
#31831 = ORIENTED_EDGE ( 'NONE', *, *, #10125, .F. ) ;
#31832 = CARTESIAN_POINT ( 'NONE',  ( 143.0000000000000568, -90.29102463692674974, -73.95413108702814498 ) ) ;
#31833 = EDGE_CURVE ( 'NONE', #11932, #13361, #2457, .T. ) ;
#31834 = EDGE_CURVE ( 'NONE', #23118, #28220, #7924, .T. ) ;
#31835 = EDGE_CURVE ( 'NONE', #8890, #24034, #31605, .T. ) ;
#31837 = CARTESIAN_POINT ( 'NONE',  ( 2.265105736952408133, -2.869810969761243502, 33.25620129461680818 ) ) ;
#31836 = CARTESIAN_POINT ( 'NONE',  ( -418.0000000000000000, 105.0000000000000142, 107.9999999999999858 ) ) ;
#31838 = EDGE_LOOP ( 'NONE', ( #26967, #581, #22534, #17178 ) ) ;
#31839 = ORIENTED_EDGE ( 'NONE', *, *, #3366, .F. ) ;
#31840 = CARTESIAN_POINT ( 'NONE',  ( -21.41424479178918361, -24.50784553716277969, -36.68877005347593467 ) ) ;
#31841 = ORIENTED_EDGE ( 'NONE', *, *, #28802, .T. ) ;
#31842 = PRODUCT_DEFINITION ( 'UNKNOWN', '', #11032, #7847 ) ;
#31843 = CARTESIAN_POINT ( 'NONE',  ( -1.791748084920704960E-16, 30.58654839005191661, 2.143968220813881942 ) ) ;
#31844 = CARTESIAN_POINT ( 'NONE',  ( -117.4999999999997442, 1.530808498934191521E-15, 12.50000000000000000 ) ) ;
#31845 = VERTEX_POINT ( 'NONE', #13105 ) ;
#31846 = DIRECTION ( 'NONE',  ( -1.000000000000000000, 0.000000000000000000, 0.000000000000000000 ) ) ;
#31847 = CIRCLE ( 'NONE', #8054, 3.999999999999976019 ) ;
#31848=STYLED_ITEM('',(#35254),#23516);
#31849 = VERTEX_POINT ( 'NONE', #10248 ) ;
#31850 = DIRECTION ( 'NONE',  ( 0.000000000000000000, 1.000000000000000000, 1.224646799147353207E-16 ) ) ;
#31851 = DIRECTION ( 'NONE',  ( -0.000000000000000000, -0.000000000000000000, -1.000000000000000000 ) ) ;
#31852 = DIRECTION ( 'NONE',  ( 0.000000000000000000, 0.000000000000000000, 1.000000000000000000 ) ) ;
#31854 = CARTESIAN_POINT ( 'NONE',  ( -0.7181323043387221050, -1.866624223957557893, 5.429999999999999716 ) ) ;
#31853 = DIRECTION ( 'NONE',  ( 0.000000000000000000, 1.131431318426415506E-52, 1.000000000000000000 ) ) ;
#31855 = LINE ( 'NONE', #1624, #10478 ) ;
#31856 = CARTESIAN_POINT ( 'NONE',  ( 5.390701026406702567, -37.47456861236020131, 68.31122994652405112 ) ) ;
#31857 = CARTESIAN_POINT ( 'NONE',  ( -20.00000000000007461, -113.0000000000000000, -162.9999999999999716 ) ) ;
#31858 = CARTESIAN_POINT ( 'NONE',  ( 2.719010691449824879, 4.557722287734057076, 31.36513882472106474 ) ) ;
#31859 = AXIS2_PLACEMENT_3D ( 'NONE', #33385, #17571, #14890 ) ;
#31860 = ORIENTED_EDGE ( 'NONE', *, *, #17876, .T. ) ;
#31861 = DIRECTION ( 'NONE',  ( 6.982962677686340075E-15, -6.982962677686193346E-15, 1.000000000000000000 ) ) ;
#31862 = VERTEX_POINT ( 'NONE', #10424 ) ;
#31863 = ORIENTED_EDGE ( 'NONE', *, *, #26150, .T. ) ;
#31864 = B_SPLINE_CURVE_WITH_KNOTS ( 'NONE', 3,
 ( #11611, #30218, #16541, #507, #2640, #13508 ),
 .UNSPECIFIED., .F., .F.,
 ( 4, 2, 4 ),
 ( 2.040444213405217924E-07, 0.001873402343194273921, 0.003746600641967207362 ),
 .UNSPECIFIED. ) ;
#31865 = AXIS2_PLACEMENT_3D ( 'NONE', #5532, #19100, #8922 ) ;
#31866 = CARTESIAN_POINT ( 'NONE',  ( 107.0769369097902057, 5.352195967840122748, 5.254935570228769670 ) ) ;
#31867 = DIRECTION ( 'NONE',  ( 2.631201909438060585E-14, -5.396010391056496978E-16, 1.000000000000000000 ) ) ;
#31868 = EDGE_CURVE ( 'NONE', #18104, #22914, #26880, .T. ) ;
#31869 = ORIENTED_EDGE ( 'NONE', *, *, #11762, .T. ) ;
#31870 = AXIS2_PLACEMENT_3D ( 'NONE', #24990, #19680, #3456 ) ;
#31871 = VERTEX_POINT ( 'NONE', #34997 ) ;
#31872 = ORIENTED_EDGE ( 'NONE', *, *, #29244, .F. ) ;
#31873 = PLANE ( 'NONE',  #5945 ) ;
#31874 = DIRECTION ( 'NONE',  ( -1.000000000000000000, -0.000000000000000000, -0.000000000000000000 ) ) ;
#31875 = EDGE_CURVE ( 'NONE', #23345, #30647, #7563, .T. ) ;
#31876 = LINE ( 'NONE', #15531, #8417 ) ;
#31877 = CARTESIAN_POINT ( 'NONE',  ( -0.6763010051031069780, -1.505030548027689319, 3.180000000000000160 ) ) ;
#31878 = ORIENTED_EDGE ( 'NONE', *, *, #17194, .F. ) ;
#31879 = ORIENTED_EDGE ( 'NONE', *, *, #9038, .T. ) ;
#31880 = CARTESIAN_POINT ( 'NONE',  ( 1.040000000000001590, -33.39989884085085947, -8.296590337300607132 ) ) ;
#31882 = LINE ( 'NONE', #13048, #14711 ) ;
#31881 = VECTOR ( 'NONE', #6637, 1000.000000000000000 ) ;
#31883 = EDGE_CURVE ( 'NONE', #26418, #23829, #20117, .T. ) ;
#31884 = DIRECTION ( 'NONE',  ( -1.000000000000000000, 0.000000000000000000, 0.000000000000000000 ) ) ;
#31885 = CARTESIAN_POINT ( 'NONE',  ( -5.527271473480783293, -1.747512292859696226, 0.000000000000000000 ) ) ;
#31886 = DIRECTION ( 'NONE',  ( 0.3701381553399144542, -0.9289767198167915296, -1.706502549609061741E-16 ) ) ;
#31887 = ORIENTED_EDGE ( 'NONE', *, *, #29422, .F. ) ;
#31888 = CIRCLE ( 'NONE', #29075, 9.999999999999998224 ) ;
#31889 = DIRECTION ( 'NONE',  ( 1.000000000000000000, 0.000000000000000000, 0.000000000000000000 ) ) ;
#31890 = DIRECTION ( 'NONE',  ( 3.697785493223492838E-32, 1.934419779023891545E-16, -1.000000000000000000 ) ) ;
#31891 = EDGE_CURVE ( 'NONE', #173, #8775, #9858, .T. ) ;
#31892 = CARTESIAN_POINT ( 'NONE',  ( 1.040000000000001146, -25.27164158951551087, -23.36088151536945645 ) ) ;
#31893 = DIRECTION ( 'NONE',  ( 1.848892746611746419E-32, 6.842277657836020854E-49, -1.000000000000000000 ) ) ;
#31894 = EDGE_CURVE ( 'NONE', #13396, #26094, #14433, .T. ) ;
#31895 = EDGE_CURVE ( 'NONE', #640, #31947, #7742, .T. ) ;
#31896 = FACE_OUTER_BOUND ( 'NONE', #33906, .T. ) ;
#31898 = CARTESIAN_POINT ( 'NONE',  ( -109.8372293046274137, 1.696271239234544037, -7.312686146626635519 ) ) ;
#31897 = CARTESIAN_POINT ( 'NONE',  ( -414.0000000000000568, 105.0000000000000000, 132.0000000000000000 ) ) ;
#31899 = AXIS2_PLACEMENT_3D ( 'NONE', #7114, #9462, #9629 ) ;
#31900 = VECTOR ( 'NONE', #27890, 1000.000000000000000 ) ;
#31901 = DIRECTION ( 'NONE',  ( 1.000000000000000000, 0.000000000000000000, 0.000000000000000000 ) ) ;
#31903 = ORIENTED_EDGE ( 'NONE', *, *, #24371, .T. ) ;
#31902 = CIRCLE ( 'NONE', #29065, 1.155000000000000027 ) ;
#31905 = AXIS2_PLACEMENT_3D ( 'NONE', #7468, #26167, #1788 ) ;
#31904 = FACE_OUTER_BOUND ( 'NONE', #11297, .T. ) ;
#31907 = CARTESIAN_POINT ( 'NONE',  ( -30.58418286738120884, -22.31615353445080174, 68.31122994652405112 ) ) ;
#31906 = DIRECTION ( 'NONE',  ( 1.000000000000000000, 0.000000000000000000, 0.000000000000000000 ) ) ;
#31908 = VERTEX_POINT ( 'NONE', #2403 ) ;
#31909 = DIRECTION ( 'NONE',  ( 0.000000000000000000, -1.000000000000000000, 2.309213040847544338E-50 ) ) ;
#31910 = ORIENTED_EDGE ( 'NONE', *, *, #16538, .T. ) ;
#31911 = CIRCLE ( 'NONE', #17677, 2.033421858999711951 ) ;
#31912 =( REPRESENTATION_RELATIONSHIP ('NONE','NONE', #23037, #28231 ) REPRESENTATION_RELATIONSHIP_WITH_TRANSFORMATION ( #16821 )SHAPE_REPRESENTATION_RELATIONSHIP( ) );
#31913 = EDGE_LOOP ( 'NONE', ( #33678, #6382, #25491, #25132 ) ) ;
#31914 = CARTESIAN_POINT ( 'NONE',  ( 2.790000000000081748, -29.22921979676814175, 9.265873697118957253 ) ) ;
#31915 = ORIENTED_EDGE ( 'NONE', *, *, #7138, .T. ) ;
#31916 = ORIENTED_EDGE ( 'NONE', *, *, #21049, .F. ) ;
#31917 = PLANE ( 'NONE',  #18490 ) ;
#31918 = PRODUCT_DEFINITION_SHAPE ( 'NONE', 'NONE',  #35190 ) ;
#31919 =( GEOMETRIC_REPRESENTATION_CONTEXT ( 3 ) GLOBAL_UNCERTAINTY_ASSIGNED_CONTEXT ( ( #6746 ) ) GLOBAL_UNIT_ASSIGNED_CONTEXT ( ( #22080, #6211, #5680 ) ) REPRESENTATION_CONTEXT ( 'NONE', 'WORKASPACE' ) );
#31920 = DIRECTION ( 'NONE',  ( 0.000000000000000000, -0.000000000000000000, -1.000000000000000000 ) ) ;
#31921 = AXIS2_PLACEMENT_3D ( 'NONE', #6562, #15119, #17457 ) ;
#31922 = DIRECTION ( 'NONE',  ( 0.000000000000000000, -1.310824597558155437E-49, -1.000000000000000000 ) ) ;
#31923 = EDGE_LOOP ( 'NONE', ( #13997, #33859, #15281, #10973 ) ) ;
#31924 = ORIENTED_EDGE ( 'NONE', *, *, #1055, .T. ) ;
#31925 = AXIS2_PLACEMENT_3D ( 'NONE', #8501, #13334, #24164 ) ;
#31926 = DIRECTION ( 'NONE',  ( 0.000000000000000000, 1.000000000000000000, 0.000000000000000000 ) ) ;
#31927 = LINE ( 'NONE', #15581, #31495 ) ;
#31928 = VECTOR ( 'NONE', #2271, 1000.000000000000000 ) ;
#31929 = CARTESIAN_POINT ( 'NONE',  ( -499.9999999999999432, -137.0000000000000000, -194.9999999999999716 ) ) ;
#31930 = EDGE_CURVE ( 'NONE', #6016, #15632, #33183, .T. ) ;
#31931 = CARTESIAN_POINT ( 'NONE',  ( 129.3530333899765594, 6.000000000000000000, -62.49999999999999289 ) ) ;
#31932 = DIRECTION ( 'NONE',  ( 0.000000000000000000, -1.000000000000000000, -5.053935297177146739E-49 ) ) ;
#31933 = UNCERTAINTY_MEASURE_WITH_UNIT (LENGTH_MEASURE( 1.000000000000000082E-05 ), #8204, 'distance_accuracy_value', 'NONE');
#31934 = ORIENTED_EDGE ( 'NONE', *, *, #27562, .F. ) ;
#31935 = CARTESIAN_POINT ( 'NONE',  ( -500.0000000000000000, -137.0000000000000000, 162.9999999999999716 ) ) ;
#31936 = EDGE_CURVE ( 'NONE', #30882, #24475, #23423, .T. ) ;
#31937 = ADVANCED_FACE ( 'NONE', ( #91 ), #3105, .T. ) ;
#31938 = FACE_OUTER_BOUND ( 'NONE', #462, .T. ) ;
#31939 = ORIENTED_EDGE ( 'NONE', *, *, #20624, .T. ) ;
#31940 = DIRECTION ( 'NONE',  ( 0.000000000000000000, 0.000000000000000000, -1.000000000000000000 ) ) ;
#31941 = CARTESIAN_POINT ( 'NONE',  ( -365.0000000000000000, -119.0000000000000000, 128.0000000000000000 ) ) ;
#31942 = DIRECTION ( 'NONE',  ( 0.9941379571543595972, -0.1081190184239417262, -1.986114147597509048E-17 ) ) ;
#31943 = ORIENTED_EDGE ( 'NONE', *, *, #29437, .T. ) ;
#31944 = DIRECTION ( 'NONE',  ( 1.000000000000000000, 0.000000000000000000, 0.000000000000000000 ) ) ;
#31945 = ORIENTED_EDGE ( 'NONE', *, *, #3451, .T. ) ;
#31946 = DIRECTION ( 'NONE',  ( -3.469446951953832974E-18, -1.000000000000000000, 7.888609052210118054E-31 ) ) ;
#31947 = VERTEX_POINT ( 'NONE', #10782 ) ;
#31949 = DIRECTION ( 'NONE',  ( -1.000000000000000000, -0.000000000000000000, -0.000000000000000000 ) ) ;
#31948 = DIRECTION ( 'NONE',  ( -0.000000000000000000, 1.000000000000000000, -0.000000000000000000 ) ) ;
#31950 = CARTESIAN_POINT ( 'NONE',  ( 1.040000000000001146, -2.430610048906252985, 34.32897884578299852 ) ) ;
#31951 = ADVANCED_FACE ( 'NONE', ( #21628 ), #205, .T. ) ;
#31952 = AXIS2_PLACEMENT_3D ( 'NONE', #25218, #8675, #5816 ) ;
#31954 = EDGE_LOOP ( 'NONE', ( #20699, #11990, #28947, #5035 ) ) ;
#31953 = CIRCLE ( 'NONE', #5802, 44.99999999999997868 ) ;
#31955 =( GEOMETRIC_REPRESENTATION_CONTEXT ( 3 ) GLOBAL_UNCERTAINTY_ASSIGNED_CONTEXT ( ( #33809 ) ) GLOBAL_UNIT_ASSIGNED_CONTEXT ( ( #16805, #14118, #27803 ) ) REPRESENTATION_CONTEXT ( 'NONE', 'WORKASPACE' ) );
#31956 = VECTOR ( 'NONE', #17030, 1000.000000000000114 ) ;
#31957 = FACE_OUTER_BOUND ( 'NONE', #26133, .T. ) ;
#31958 = DIRECTION ( 'NONE',  ( -1.000000000000000000, 0.000000000000000000, 0.000000000000000000 ) ) ;
#31959 = EDGE_CURVE ( 'NONE', #12542, #8355, #621, .T. ) ;
#31960 = ORIENTED_EDGE ( 'NONE', *, *, #31895, .T. ) ;
#31961 = EDGE_CURVE ( 'NONE', #30502, #6872, #5760, .T. ) ;
#31962 = ADVANCED_FACE ( 'NONE', ( #271 ), #5587, .T. ) ;
#31963 = CARTESIAN_POINT ( 'NONE',  ( 774.6728052478960080, 1171.715138231090805, 1753.598338701303192 ) ) ;
#31964 = ORIENTED_EDGE ( 'NONE', *, *, #33516, .F. ) ;
#31965 = CARTESIAN_POINT ( 'NONE',  ( -361.0000000000000000, 134.9999999999999716, 126.0000000000000000 ) ) ;
#31966 = ORIENTED_EDGE ( 'NONE', *, *, #19808, .T. ) ;
#31967 = CARTESIAN_POINT ( 'NONE',  ( -70.00000000000000000, 4.559999999999908127, -172.9900000000000091 ) ) ;
#31968 = EDGE_CURVE ( 'NONE', #9649, #10216, #29197, .T. ) ;
#31969 = CARTESIAN_POINT ( 'NONE',  ( 0.000000000000000000, 0.000000000000000000, 0.000000000000000000 ) ) ;
#31970 = DIRECTION ( 'NONE',  ( -0.000000000000000000, 1.000000000000000000, -0.000000000000000000 ) ) ;
#31971 = DIRECTION ( 'NONE',  ( 0.000000000000000000, 1.000000000000000000, 1.224646799147353207E-16 ) ) ;
#31972 = CONTEXT_DEPENDENT_SHAPE_REPRESENTATION ( #13750, #20846 ) ;
#31973 = ORIENTED_EDGE ( 'NONE', *, *, #817, .T. ) ;
#31974 = ORIENTED_EDGE ( 'NONE', *, *, #17782, .T. ) ;
#31975 = ORIENTED_EDGE ( 'NONE', *, *, #33232, .T. ) ;
#31976 = DIRECTION ( 'NONE',  ( -1.000000000000000000, 0.000000000000000000, -0.000000000000000000 ) ) ;
#31977 = CARTESIAN_POINT ( 'NONE',  ( -37.58721499952019940, -4.609089608337754385, 68.31122994652405112 ) ) ;
#31978 = AXIS2_PLACEMENT_3D ( 'NONE', #1077, #25269, #11589 ) ;
#31979 = DIRECTION ( 'NONE',  ( 0.000000000000000000, 0.000000000000000000, 1.000000000000000000 ) ) ;
#31980 = DIRECTION ( 'NONE',  ( 0.000000000000000000, 0.000000000000000000, -1.000000000000000000 ) ) ;
#31981 = AXIS2_PLACEMENT_3D ( 'NONE', #29684, #15471, #7961 ) ;
#31982 = ADVANCED_FACE ( 'NONE', ( #19155 ), #3597, .T. ) ;
#31983 = EDGE_CURVE ( 'NONE', #4316, #2764, #24453, .T. ) ;
#31984 = CARTESIAN_POINT ( 'NONE',  ( -8.191443212915034962E-14, -27.65011189337360520, 13.25424764731395655 ) ) ;
#31985 = CIRCLE ( 'NONE', #16667, 4.000000000000003553 ) ;
#31986 = DIRECTION ( 'NONE',  ( 0.000000000000000000, 0.000000000000000000, 1.000000000000000000 ) ) ;
#31987 = VERTEX_POINT ( 'NONE', #24988 ) ;
#31988 = CARTESIAN_POINT ( 'NONE',  ( 2.789999999999999147, 30.93646776788807173, -7.943134866715984899 ) ) ;
#31989 = CARTESIAN_POINT ( 'NONE',  ( 99.56190681375883855, 1.868749050043680082, 12.36447865323539652 ) ) ;
#31990 = FACE_OUTER_BOUND ( 'NONE', #4881, .T. ) ;
#31991 = ORIENTED_EDGE ( 'NONE', *, *, #27408, .F. ) ;
#31992 = CARTESIAN_POINT ( 'NONE',  ( 0.000000000000000000, 1.653273178848927064E-15, -13.50000000000000178 ) ) ;
#31993 = ORIENTED_EDGE ( 'NONE', *, *, #1199, .T. ) ;
#31994 = CARTESIAN_POINT ( 'NONE',  ( -109.5901181662249542, 2.281765576240578852, -12.29396198687796726 ) ) ;
#31995 = DIRECTION ( 'NONE',  ( -1.000000000000000000, 0.000000000000000000, -0.000000000000000000 ) ) ;
#31996 = AXIS2_PLACEMENT_3D ( 'NONE', #23214, #17545, #31219 ) ;
#31997 = ORIENTED_EDGE ( 'NONE', *, *, #31693, .F. ) ;
#31998 = DIRECTION ( 'NONE',  ( 0.000000000000000000, 0.000000000000000000, -1.000000000000000000 ) ) ;
#31999 = CARTESIAN_POINT ( 'NONE',  ( -29.34345171400088859, 14.07715221144535533, 68.31122994652405112 ) ) ;
#32000 = DIRECTION ( 'NONE',  ( 0.000000000000000000, 0.000000000000000000, -1.000000000000000000 ) ) ;
#32001 = VERTEX_POINT ( 'NONE', #24283 ) ;
#32002 = ADVANCED_FACE ( 'NONE', ( #22332 ), #8094, .F. ) ;
#32003 = AXIS2_PLACEMENT_3D ( 'NONE', #27725, #683, #24510 ) ;
#32004 = ADVANCED_FACE ( 'NONE', ( #30340 ), #2925, .F. ) ;
#32005 = VERTEX_POINT ( 'NONE', #11483 ) ;
#32006 = AXIS2_PLACEMENT_3D ( 'NONE', #2233, #21102, #9896 ) ;
#32007 = DIRECTION ( 'NONE',  ( -1.137124490013589674E-14, 5.100966482838833881E-14, 0.9999999999999998890 ) ) ;
#32008 = ORIENTED_EDGE ( 'NONE', *, *, #34316, .F. ) ;
#32009 = DIRECTION ( 'NONE',  ( -1.000000000000000000, -0.000000000000000000, 0.000000000000000000 ) ) ;
#32010 = EDGE_CURVE ( 'NONE', #29274, #736, #32826, .T. ) ;
#32011 =( NAMED_UNIT ( * ) PLANE_ANGLE_UNIT ( ) SI_UNIT ( $, .RADIAN. ) );
#32012 = CARTESIAN_POINT ( 'NONE',  ( -12.00000000000001066, -145.0000000000000000, -190.9999999999999432 ) ) ;
#32013 = CARTESIAN_POINT ( 'NONE',  ( 5.048285286872369737E-16, -27.64940622781549351, -13.25307083675178887 ) ) ;
#32014 = ITEM_DEFINED_TRANSFORMATION ( 'NONE', 'NONE', #29729,  #28566 ) ;
#32016 = ADVANCED_FACE ( 'NONE', ( #452 ), #27666, .F. ) ;
#32015 = VERTEX_POINT ( 'NONE', #5942 ) ;
#32017 = DIRECTION ( 'NONE',  ( 0.000000000000000000, 0.000000000000000000, 1.000000000000000000 ) ) ;
#32018 = VECTOR ( 'NONE', #8154, 1000.000000000000000 ) ;
#32020 = DIRECTION ( 'NONE',  ( -1.000000000000000000, 0.000000000000000000, -0.000000000000000000 ) ) ;
#32019 = CARTESIAN_POINT ( 'NONE',  ( -19.99999999999998934, 134.9999999999999432, -186.9999999999999716 ) ) ;
#32021 = EDGE_LOOP ( 'NONE', ( #20515, #28860, #18040, #19777 ) ) ;
#32022 = ORIENTED_EDGE ( 'NONE', *, *, #9414, .F. ) ;
#32023 = CARTESIAN_POINT ( 'NONE',  ( 5.021133111224473033, 8.235406450278427215, -67.50000000000000000 ) ) ;
#32024 = ORIENTED_EDGE ( 'NONE', *, *, #18712, .T. ) ;
#32025 = LINE ( 'NONE', #21366, #1678 ) ;
#32026 = LINE ( 'NONE', #27047, #32460 ) ;
#32027 = ORIENTED_EDGE ( 'NONE', *, *, #18707, .T. ) ;
#32028 = AXIS2_PLACEMENT_3D ( 'NONE', #12593, #31619, #28779 ) ;
#32029 = DIRECTION ( 'NONE',  ( 0.000000000000000000, 7.888609052210118054E-31, 1.000000000000000000 ) ) ;
#32030 = VECTOR ( 'NONE', #18974, 1000.000000000000114 ) ;
#32031 = PRODUCT_DEFINITION_SHAPE ( 'NONE', 'NONE',  #35226 ) ;
#32032 = DIRECTION ( 'NONE',  ( -0.3193015301359797276, -0.9476531711828024562, 0.000000000000000000 ) ) ;
#32033 = ORIENTED_EDGE ( 'NONE', *, *, #18867, .F. ) ;
#32034 = EDGE_CURVE ( 'NONE', #7089, #29651, #5878, .T. ) ;
#32035 = PLANE ( 'NONE',  #456 ) ;
#32036 = SURFACE_STYLE_FILL_AREA ( #12322 ) ;
#32037 = FACE_OUTER_BOUND ( 'NONE', #25510, .T. ) ;
#32039 = DIRECTION ( 'NONE',  ( 1.000000000000000000, 0.000000000000000000, 0.000000000000000000 ) ) ;
#32038 = CARTESIAN_POINT ( 'NONE',  ( 145.0000000000000568, -78.33668825982579165, -63.00000000000000000 ) ) ;
#32040 = DIRECTION ( 'NONE',  ( 0.000000000000000000, 2.312964634635740689E-15, -1.000000000000000000 ) ) ;
#32041 = CARTESIAN_POINT ( 'NONE',  ( 0.01077896562537771982, 28.09136514857379296, -12.86217335695005559 ) ) ;
#32042 = FACE_OUTER_BOUND ( 'NONE', #6800, .T. ) ;
#32043 = EDGE_CURVE ( 'NONE', #26108, #23877, #2579, .T. ) ;
#32044 = ADVANCED_FACE ( 'NONE', ( #5420 ), #16309, .T. ) ;
#32045 = EDGE_CURVE ( 'NONE', #20392, #26810, #12019, .T. ) ;
#32046 = EDGE_LOOP ( 'NONE', ( #19945, #26734, #3788, #2410 ) ) ;
#32047 = DIRECTION ( 'NONE',  ( -0.8800945906173212041, 0.4747983904418058843, 9.738240694054581881E-15 ) ) ;
#32048 = ORIENTED_EDGE ( 'NONE', *, *, #31103, .F. ) ;
#32049 = ORIENTED_EDGE ( 'NONE', *, *, #8693, .F. ) ;
#32050 = LINE ( 'NONE', #16074, #33588 ) ;
#32051 = CIRCLE ( 'NONE', #29778, 11.80000000000000071 ) ;
#32052 = DIRECTION ( 'NONE',  ( -0.000000000000000000, -0.000000000000000000, -1.000000000000000000 ) ) ;
#32053 = DIRECTION ( 'NONE',  ( 0.000000000000000000, 0.000000000000000000, 1.000000000000000000 ) ) ;
#32054 = AXIS2_PLACEMENT_3D ( 'NONE', #10826, #30528, #31995 ) ;
#32055 = ORIENTED_EDGE ( 'NONE', *, *, #9768, .F. ) ;
#32056 = ORIENTED_EDGE ( 'NONE', *, *, #34557, .F. ) ;
#32057 = DIRECTION ( 'NONE',  ( 0.000000000000000000, 0.000000000000000000, 1.000000000000000000 ) ) ;
#32058 = FILL_AREA_STYLE_COLOUR ( '', #25522 ) ;
#32059 = AXIS2_PLACEMENT_3D ( 'NONE', #32799, #422, #19296 ) ;
#32060 = ITEM_DEFINED_TRANSFORMATION ( 'NONE', 'NONE', #20135,  #28566 ) ;
#32061 = DIRECTION ( 'NONE',  ( 0.000000000000000000, 0.000000000000000000, -1.000000000000000000 ) ) ;
#32062 = CARTESIAN_POINT ( 'NONE',  ( 28.23027531293552528, -17.65143121711728469, 0.000000000000000000 ) ) ;
#32063 = VERTEX_POINT ( 'NONE', #3629 ) ;
#32064 = EDGE_LOOP ( 'NONE', ( #9124, #444, #19332, #33514 ) ) ;
#32065 = DIRECTION ( 'NONE',  ( -1.000000000000000000, 0.000000000000000000, 0.000000000000000000 ) ) ;
#32066 = CARTESIAN_POINT ( 'NONE',  ( 3.235562306570555532E-30, -1.691831803474591833, -67.50000000000000000 ) ) ;
#32067 = CARTESIAN_POINT ( 'NONE',  ( 15.00000000000000000, 1.836970198721029589E-15, 0.000000000000000000 ) ) ;
#32068 = FACE_OUTER_BOUND ( 'NONE', #34947, .T. ) ;
#32069 = DIRECTION ( 'NONE',  ( 0.000000000000000000, 0.9961946980917455452, -0.08715574274765887364 ) ) ;
#32070 = ORIENTED_EDGE ( 'NONE', *, *, #1136, .T. ) ;
#32071 = CYLINDRICAL_SURFACE ( 'NONE', #5536, 4.750000000000004441 ) ;
#32072 = FACE_OUTER_BOUND ( 'NONE', #24327, .T. ) ;
#32073 = VECTOR ( 'NONE', #3425, 1000.000000000000000 ) ;
#32074 = AXIS2_PLACEMENT_3D ( 'NONE', #14452, #33117, #390 ) ;
#32075 = DIRECTION ( 'NONE',  ( 1.000000000000000000, 0.000000000000000000, -0.000000000000000000 ) ) ;
#32076 = CARTESIAN_POINT ( 'NONE',  ( -442.0000000000000000, 124.9999999999999432, -162.9999999999999716 ) ) ;
#32077 = ADVANCED_FACE ( 'NONE', ( #34425 ), #25570, .T. ) ;
#32078 = CARTESIAN_POINT ( 'NONE',  ( 105.9796427714311733, 5.657131480001861057, -4.924467467246998353 ) ) ;
#32080 = DIRECTION ( 'NONE',  ( -0.000000000000000000, 0.000000000000000000, 1.000000000000000000 ) ) ;
#32079 = CARTESIAN_POINT ( 'NONE',  ( -45.00000000000000000, -38.34433698000722046, 36.69637551990492597 ) ) ;
#32081 = CIRCLE ( 'NONE', #12221, 13.50000000000000178 ) ;
#32082 = VECTOR ( 'NONE', #413, 1000.000000000000000 ) ;
#32083 = ADVANCED_FACE ( 'NONE', ( #25165 ), #22518, .T. ) ;
#32084 = FACE_BOUND ( 'NONE', #27822, .T. ) ;
#32085 = ORIENTED_EDGE ( 'NONE', *, *, #33580, .T. ) ;
#32086 = CARTESIAN_POINT ( 'NONE',  ( 110.4380931862411899, 1.868749050043681192, -12.36447865323539475 ) ) ;
#32088 = CARTESIAN_POINT ( 'NONE',  ( -349.0000000000000000, 134.9999999999999716, 130.0000000000000000 ) ) ;
#32087 = LINE ( 'NONE', #29601, #5246 ) ;
#32089 = AXIS2_PLACEMENT_3D ( 'NONE', #16722, #30588, #14041 ) ;
#32090 = EDGE_CURVE ( 'NONE', #13032, #27734, #34898, .T. ) ;
#32091 = ADVANCED_FACE ( 'NONE', ( #30701 ), #21798, .T. ) ;
#32092 = ORIENTED_EDGE ( 'NONE', *, *, #31833, .F. ) ;
#32093 = CARTESIAN_POINT ( 'NONE',  ( -418.0000000000000000, -104.9999999999999716, -190.9999999999999716 ) ) ;
#32094 = EDGE_CURVE ( 'NONE', #19171, #19439, #6291, .T. ) ;
#32095 = ORIENTED_EDGE ( 'NONE', *, *, #23297, .F. ) ;
#32096 = AXIS2_PLACEMENT_3D ( 'NONE', #386, #11240, #25097 ) ;
#32097 = ORIENTED_EDGE ( 'NONE', *, *, #30128, .T. ) ;
#32098 = FACE_BOUND ( 'NONE', #17361, .T. ) ;
#32099 = ORIENTED_EDGE ( 'NONE', *, *, #27606, .F. ) ;
#32100 = EDGE_LOOP ( 'NONE', ( #34832, #30735, #28281, #15593 ) ) ;
#32101 = DIRECTION ( 'NONE',  ( -0.1081190184239421009, 0.9941379571543595972, 0.000000000000000000 ) ) ;
#32102 = CIRCLE ( 'NONE', #7074, 2.524999999999999911 ) ;
#32103 = EDGE_CURVE ( 'NONE', #25412, #30341, #11850, .T. ) ;
#32104 = CARTESIAN_POINT ( 'NONE',  ( -37.69926482250235722, 3.578808500140884252, -36.68877005347593467 ) ) ;
#32105 = AXIS2_PLACEMENT_3D ( 'NONE', #30388, #22379, #3847 ) ;
#32106 = DIRECTION ( 'NONE',  ( 0.000000000000000000, 1.000000000000000000, 0.000000000000000000 ) ) ;
#32107 = CARTESIAN_POINT ( 'NONE',  ( -6.500000000000000000, 0.000000000000000000, 3.930000000000000160 ) ) ;
#32108 = ORIENTED_EDGE ( 'NONE', *, *, #16323, .T. ) ;
#32109 = VERTEX_POINT ( 'NONE', #33897 ) ;
#32110 = CIRCLE ( 'NONE', #18504, 4.000000000000003553 ) ;
#32111 = CARTESIAN_POINT ( 'NONE',  ( 0.02407890056655781832, 7.350529080603967813, -30.20932655202929595 ) ) ;
#32112 = DIRECTION ( 'NONE',  ( 1.000000000000000000, 0.000000000000000000, 0.000000000000000000 ) ) ;
#32113 = CARTESIAN_POINT ( 'NONE',  ( -12.00000000000001066, -145.0000000000000000, -158.9999999999999716 ) ) ;
#32114 = AXIS2_PLACEMENT_3D ( 'NONE', #10379, #10204, #29250 ) ;
#32115 = DIRECTION ( 'NONE',  ( 1.000000000000000000, 0.000000000000000000, 0.000000000000000000 ) ) ;
#32116 = LINE ( 'NONE', #31761, #22227 ) ;
#32117 = ORIENTED_EDGE ( 'NONE', *, *, #19889, .F. ) ;
#32118 = CARTESIAN_POINT ( 'NONE',  ( -361.0000000000000000, -125.0000000000000284, 168.9999999999999716 ) ) ;
#32119 = DIRECTION ( 'NONE',  ( 0.000000000000000000, 0.8660254037844375974, -0.5000000000000019984 ) ) ;
#32120 = VERTEX_POINT ( 'NONE', #20028 ) ;
#32121 = CYLINDRICAL_SURFACE ( 'NONE', #2634, 9.999999999999996447 ) ;
#32122 = DIRECTION ( 'NONE',  ( 0.000000000000000000, 0.000000000000000000, -1.000000000000000000 ) ) ;
#32123 = CARTESIAN_POINT ( 'NONE',  ( 2.604019726408915769, -8.821517218320241938, 31.05303142369421465 ) ) ;
#32124 = ORIENTED_EDGE ( 'NONE', *, *, #13583, .T. ) ;
#32125 = CARTESIAN_POINT ( 'NONE',  ( 0.000000000000000000, 2.281310696040539424E-14, -36.68877005347592757 ) ) ;
#32126 = EDGE_LOOP ( 'NONE', ( #27334, #7212, #9027, #9061 ) ) ;
#32127 = AXIS2_PLACEMENT_3D ( 'NONE', #21486, #32327, #16335 ) ;
#32128 = VECTOR ( 'NONE', #1661, 1000.000000000000000 ) ;
#32129 = CARTESIAN_POINT ( 'NONE',  ( 1.395000000000002238, 31.89769921723006263, -12.91988538846923973 ) ) ;
#32130 = ORIENTED_EDGE ( 'NONE', *, *, #17902, .F. ) ;
#32132 = CARTESIAN_POINT ( 'NONE',  ( 0.000000000000000000, 9.869977788041397915, -30.37666815053925973 ) ) ;
#32131 = CARTESIAN_POINT ( 'NONE',  ( 0.2014843505975234261, 29.63244935463695739, 13.00174666746673324 ) ) ;
#32133 = VECTOR ( 'NONE', #6685, 1000.000000000000000 ) ;
#32134 = LINE ( 'NONE', #18634, #10269 ) ;
#32135 = EDGE_CURVE ( 'NONE', #27961, #20453, #4730, .T. ) ;
#32136 = ORIENTED_EDGE ( 'NONE', *, *, #9403, .F. ) ;
#32137 = TOROIDAL_SURFACE ( 'NONE', #20765, 30.47050528711512030, 8.000000000000000000 ) ;
#32138 =( REPRESENTATION_RELATIONSHIP ('NONE','NONE', #23037, #19821 ) REPRESENTATION_RELATIONSHIP_WITH_TRANSFORMATION ( #3034 )SHAPE_REPRESENTATION_RELATIONSHIP( ) );
#32139 = DIRECTION ( 'NONE',  ( 0.000000000000000000, 0.000000000000000000, 1.000000000000000000 ) ) ;
#32140 = CARTESIAN_POINT ( 'NONE',  ( 1.749999999999999778, 28.00026196654270905, 20.00929742917132970 ) ) ;
#32141 = EDGE_CURVE ( 'NONE', #23936, #7759, #15563, .T. ) ;
#32142 = VECTOR ( 'NONE', #30120, 1000.000000000000000 ) ;
#32143 = ADVANCED_FACE ( 'NONE', ( #12371 ), #24630, .T. ) ;
#32144 = ORIENTED_EDGE ( 'NONE', *, *, #5963, .T. ) ;
#32145 = EDGE_CURVE ( 'NONE', #26960, #32615, #4150, .T. ) ;
#32146 = EDGE_CURVE ( 'NONE', #29515, #13784, #27843, .T. ) ;
#32147 = DIRECTION ( 'NONE',  ( -0.1063910735369225230, 0.9943243633099118073, -1.000770725407345128E-14 ) ) ;
#32148 = VERTEX_POINT ( 'NONE', #25523 ) ;
#32149 = DIRECTION ( 'NONE',  ( -0.000000000000000000, -1.836970198721029688E-16, 1.000000000000000000 ) ) ;
#32150 = ORIENTED_EDGE ( 'NONE', *, *, #25780, .F. ) ;
#32151 = CARTESIAN_POINT ( 'NONE',  ( -20.02113311122488781, 6.201984591278717041, -67.50000000000000000 ) ) ;
#32152 = CARTESIAN_POINT ( 'NONE',  ( 15.99999999999998579, 136.9999999999999716, -155.0000000000000000 ) ) ;
#32153 = CIRCLE ( 'NONE', #12861, 3.999999999999976019 ) ;
#32154 = CARTESIAN_POINT ( 'NONE',  ( -108.1287192516100504, -4.059672565113384479, -6.310142985817148720 ) ) ;
#32155 = FACE_OUTER_BOUND ( 'NONE', #27769, .T. ) ;
#32156 = EDGE_LOOP ( 'NONE', ( #19954, #30303, #6830, #12835 ) ) ;
#32157 = VERTEX_POINT ( 'NONE', #9339 ) ;
#32158 = ORIENTED_EDGE ( 'NONE', *, *, #31804, .F. ) ;
#32159 = DIRECTION ( 'NONE',  ( 0.000000000000000000, 0.000000000000000000, 1.000000000000000000 ) ) ;
#32160 = FACE_OUTER_BOUND ( 'NONE', #33832, .T. ) ;
#32161 = VECTOR ( 'NONE', #5186, 1000.000000000000000 ) ;
#32162 = EDGE_CURVE ( 'NONE', #29128, #27741, #12895, .T. ) ;
#32163 = DIRECTION ( 'NONE',  ( -1.000000000000000000, -0.000000000000000000, -0.000000000000000000 ) ) ;
#32164 = FACE_OUTER_BOUND ( 'NONE', #21958, .T. ) ;
#32165 = CARTESIAN_POINT ( 'NONE',  ( -35.00000000000000000, 0.5883377166428923610, 68.31122994652405112 ) ) ;
#32166 = CARTESIAN_POINT ( 'NONE',  ( 1.649999999999999911, 2.020667218593132262E-16, 0.000000000000000000 ) ) ;
#32167 = DIRECTION ( 'NONE',  ( -0.000000000000000000, -0.000000000000000000, -1.000000000000000000 ) ) ;
#32168 = EDGE_LOOP ( 'NONE', ( #16888, #27815, #16157, #14316 ) ) ;
#32169 = B_SPLINE_CURVE_WITH_KNOTS ( 'NONE', 3,
 ( #26728, #34934, #26379, #7501 ),
 .UNSPECIFIED., .F., .F.,
 ( 4, 4 ),
 ( 4.608367445541821421E-07, 0.0006881987313283487910 ),
 .UNSPECIFIED. ) ;
#32170 = VECTOR ( 'NONE', #10867, 1000.000000000000000 ) ;
#32171 = DIRECTION ( 'NONE',  ( 0.000000000000000000, 1.836970198721029441E-16, -1.000000000000000000 ) ) ;
#32172 = CARTESIAN_POINT ( 'NONE',  ( 0.000000000000000000, 3.524919873834583163E-15, 68.31122994652405112 ) ) ;
#32173 = CARTESIAN_POINT ( 'NONE',  ( -410.0000000000000568, -137.0000000000000000, 154.9999999999999716 ) ) ;
#32175 = EDGE_CURVE ( 'NONE', #29708, #890, #14868, .T. ) ;
#32174 = EDGE_LOOP ( 'NONE', ( #33805, #18628, #14138, #8721, #26088, #11125, #20167, #31915, #21497, #32741, #11497, #8329, #12063, #26427, #7518, #27323 ) ) ;
#32176 = EDGE_CURVE ( 'NONE', #19981, #11239, #7579, .T. ) ;
#32177 = CARTESIAN_POINT ( 'NONE',  ( -20.00000000000004619, -134.9999999999999716, -162.9999999999999432 ) ) ;
#32178 = ORIENTED_EDGE ( 'NONE', *, *, #23425, .T. ) ;
#32179 = DIRECTION ( 'NONE',  ( -0.000000000000000000, -1.000000000000000000, -0.000000000000000000 ) ) ;
#32180 = CARTESIAN_POINT ( 'NONE',  ( -12.00000000000001066, -145.0000000000000000, -162.9999999999999432 ) ) ;
#32181 = AXIS2_PLACEMENT_3D ( 'NONE', #28537, #6805, #20358 ) ;
#32182 = EDGE_LOOP ( 'NONE', ( #20512, #8252, #33344, #8924 ) ) ;
#32183 = CARTESIAN_POINT ( 'NONE',  ( -15.99999999999998579, -32.99999999999997158, -175.0000000000000000 ) ) ;
#32184 = DIRECTION ( 'NONE',  ( 1.000000000000000000, 0.000000000000000000, 0.000000000000000000 ) ) ;
#32185 = CARTESIAN_POINT ( 'NONE',  ( -28.00450684652666311, 16.58167570419055892, -36.68877005347593467 ) ) ;
#32186 = VECTOR ( 'NONE', #19890, 1000.000000000000000 ) ;
#32187 = EDGE_LOOP ( 'NONE', ( #30519, #12037, #25503, #7722 ) ) ;
#32188 = ORIENTED_EDGE ( 'NONE', *, *, #2145, .F. ) ;
#32189 = EDGE_CURVE ( 'NONE', #33069, #21781, #23048, .T. ) ;
#32190 = EDGE_CURVE ( 'NONE', #21633, #7246, #17715, .T. ) ;
#32191 = DIRECTION ( 'NONE',  ( 0.7685687837533879962, 0.6397671643964215615, 1.320557265072203023E-14 ) ) ;
#32192 =( REPRESENTATION_RELATIONSHIP ('NONE','NONE', #23037, #28231 ) REPRESENTATION_RELATIONSHIP_WITH_TRANSFORMATION ( #13392 )SHAPE_REPRESENTATION_RELATIONSHIP( ) );
#32193 = CARTESIAN_POINT ( 'NONE',  ( -355.0000000000000000, -117.0000000000000000, 126.0000000000000000 ) ) ;
#32194 = ORIENTED_EDGE ( 'NONE', *, *, #25842, .F. ) ;
#32195 = VECTOR ( 'NONE', #29602, 1000.000000000000000 ) ;
#32196 = DIRECTION ( 'NONE',  ( 1.000000000000000000, 0.000000000000000000, -1.848892746611746966E-32 ) ) ;
#32197 = FACE_OUTER_BOUND ( 'NONE', #10145, .T. ) ;
#32198 = CARTESIAN_POINT ( 'NONE',  ( 129.3530333899765594, 6.000000000000000000, 62.49999999999999289 ) ) ;
#32199 = ITEM_DEFINED_TRANSFORMATION ( 'NONE', 'NONE', #24021,  #28566 ) ;
#32200 = ORIENTED_EDGE ( 'NONE', *, *, #29364, .T. ) ;
#32201 = CARTESIAN_POINT ( 'NONE',  ( -12.00000000000001066, -109.0000000000000142, 174.9999999999999432 ) ) ;
#32202 = VECTOR ( 'NONE', #28364, 1000.000000000000227 ) ;
#32204 = DIRECTION ( 'NONE',  ( 0.000000000000000000, 0.000000000000000000, 1.000000000000000000 ) ) ;
#32203 = DIRECTION ( 'NONE',  ( 0.000000000000000000, 0.000000000000000000, 1.000000000000000000 ) ) ;
#32205 = EDGE_LOOP ( 'NONE', ( #3337, #11778 ) ) ;
#32206 = ORIENTED_EDGE ( 'NONE', *, *, #20455, .T. ) ;
#32207 = CARTESIAN_POINT ( 'NONE',  ( -23.46927268871044348, -22.54767421130283012, -36.68877005347593467 ) ) ;
#32208 = ORIENTED_EDGE ( 'NONE', *, *, #26760, .F. ) ;
#32209 = ADVANCED_FACE ( 'NONE', ( #23893 ), #20720, .F. ) ;
#32210 = CARTESIAN_POINT ( 'NONE',  ( 2.783128945071976723, -3.550602046213238161, -30.66465032581545103 ) ) ;
#32211 = CARTESIAN_POINT ( 'NONE',  ( -36.80830595996284416, 8.862931941313782147, 24.65111515542800547 ) ) ;
#32212 = EDGE_LOOP ( 'NONE', ( #30544, #17214, #25587, #22246 ) ) ;
#32213 = ADVANCED_FACE ( 'NONE', ( #32084, #31733 ), #12719, .T. ) ;
#32215 = EDGE_CURVE ( 'NONE', #31108, #32651, #26399, .T. ) ;
#32214 = ADVANCED_BREP_SHAPE_REPRESENTATION ( '', ( #10712, #28566 ), #10929 ) ;
#32216 = CARTESIAN_POINT ( 'NONE',  ( 11.99999999999999645, 134.9999999999998863, 155.0000000000000000 ) ) ;
#32217 = CARTESIAN_POINT ( 'NONE',  ( 0.02849990174190952102, -12.35429686688394391, -5.601730134768054370 ) ) ;
#32218 = EDGE_LOOP ( 'NONE', ( #16231, #8119, #33272, #25726 ) ) ;
#32219 = FACE_OUTER_BOUND ( 'NONE', #18037, .T. ) ;
#32220 = LINE ( 'NONE', #7831, #4630 ) ;
#32221 = EDGE_CURVE ( 'NONE', #5645, #28398, #4185, .T. ) ;
#32222 = DIRECTION ( 'NONE',  ( -1.000000000000000000, -0.000000000000000000, 0.000000000000000000 ) ) ;
#32224 = CARTESIAN_POINT ( 'NONE',  ( -27.13361903382165963, -26.41607761506757868, 68.31122994652405112 ) ) ;
#32223 = DIRECTION ( 'NONE',  ( 0.000000000000000000, -1.000000000000000000, 0.000000000000000000 ) ) ;
#32225 = B_SPLINE_CURVE_WITH_KNOTS ( 'NONE', 3,
 ( #1939, #12823, #12470, #34515, #4423, #20471 ),
 .UNSPECIFIED., .F., .F.,
 ( 4, 2, 4 ),
 ( 2.257612537762607475E-07, 0.001873424083712463013, 0.003746622406171149465 ),
 .UNSPECIFIED. ) ;
#32226 = DIRECTION ( 'NONE',  ( -0.000000000000000000, 1.836970198721029688E-16, -1.000000000000000000 ) ) ;
#32227 = DIRECTION ( 'NONE',  ( 0.000000000000000000, 0.000000000000000000, -1.000000000000000000 ) ) ;
#32228 = CYLINDRICAL_SURFACE ( 'NONE', #1878, 1.999999999999999556 ) ;
#32229=STYLED_ITEM('',(#35254),#21945);
#32230 = AXIS2_PLACEMENT_3D ( 'NONE', #30601, #6192, #17087 ) ;
#32231 = VECTOR ( 'NONE', #18865, 1000.000000000000000 ) ;
#32232 = VERTEX_POINT ( 'NONE', #26748 ) ;
#32233 = FACE_BOUND ( 'NONE', #15868, .T. ) ;
#32234 = CARTESIAN_POINT ( 'NONE',  ( 787.0597240610638892, 1342.348721680655444, 1330.896119909291656 ) ) ;
#32235 = ORIENTED_EDGE ( 'NONE', *, *, #32793, .F. ) ;
#32236 = VERTEX_POINT ( 'NONE', #7702 ) ;
#32237 = CARTESIAN_POINT ( 'NONE',  ( 106.9002205115570376, 5.417593104495392886, 5.187149597110491506 ) ) ;
#32238 = VERTEX_POINT ( 'NONE', #23381 ) ;
#32239 = CARTESIAN_POINT ( 'NONE',  ( 19.99999999999998934, 4.559999999999908127, -172.9900000000000091 ) ) ;
#32240 = FILL_AREA_STYLE ('',( #5523 ) ) ;
#32241 = CARTESIAN_POINT ( 'NONE',  ( -23.46927268871045058, -22.54767421130284077, 68.31122994652405112 ) ) ;
#32242 = AXIS2_PLACEMENT_3D ( 'NONE', #4514, #27430, #7365 ) ;
#32243 = ORIENTED_EDGE ( 'NONE', *, *, #1100, .T. ) ;
#32244 = ORIENTED_EDGE ( 'NONE', *, *, #4751, .T. ) ;
#32245 = CARTESIAN_POINT ( 'NONE',  ( 12.00000000000001066, -134.9999999999999716, 194.9999999999999716 ) ) ;
#32246 = CARTESIAN_POINT ( 'NONE',  ( -365.0000000000000000, -125.0000000000000284, 113.9999999999999858 ) ) ;
#32247 = CARTESIAN_POINT ( 'NONE',  ( 0.7561992106246575585, 31.72496621377049308, 11.99023130257964986 ) ) ;
#32248 = CARTESIAN_POINT ( 'NONE',  ( 35.44043929807611448, -12.65143121711728291, 14.30932821646982411 ) ) ;
#32249 = CARTESIAN_POINT ( 'NONE',  ( 2.789999999999999591, 23.76428138080743224, 19.37504760381664326 ) ) ;
#32250 = VERTEX_POINT ( 'NONE', #28898 ) ;
#32251 = EDGE_CURVE ( 'NONE', #29816, #27865, #2019, .T. ) ;
#32253 = VECTOR ( 'NONE', #24483, 1000.000000000000000 ) ;
#32252 = FACE_OUTER_BOUND ( 'NONE', #29043, .T. ) ;
#32255 = DIRECTION ( 'NONE',  ( 0.8835120444460227151, -0.4684084406997903183, 0.000000000000000000 ) ) ;
#32254 = AXIS2_PLACEMENT_3D ( 'NONE', #16437, #25115, #19280 ) ;
#32256 = EDGE_CURVE ( 'NONE', #11246, #15089, #3068, .T. ) ;
#32257 = CARTESIAN_POINT ( 'NONE',  ( 50.00050000000000239, 12.80000000000000071, 3.000000000000000000 ) ) ;
#32258 = CARTESIAN_POINT ( 'NONE',  ( 0.5248941666463887712, -24.85743842207099874, -22.27820639183348916 ) ) ;
#32259 = FACE_OUTER_BOUND ( 'NONE', #27577, .T. ) ;
#32260 = CARTESIAN_POINT ( 'NONE',  ( -99.88497961182919482, 6.264093345946821604E-16, 60.00000000000000000 ) ) ;
#32262 = CARTESIAN_POINT ( 'NONE',  ( 8.000000000000003553, 0.000000000000000000, 0.000000000000000000 ) ) ;
#32261 = FACE_OUTER_BOUND ( 'NONE', #34563, .T. ) ;
#32263 = DIRECTION ( 'NONE',  ( -0.000000000000000000, 1.836970198721029934E-16, -1.000000000000000000 ) ) ;
#32264 = ORIENTED_EDGE ( 'NONE', *, *, #3010, .T. ) ;
#32265 = FACE_OUTER_BOUND ( 'NONE', #14597, .T. ) ;
#32267 = CARTESIAN_POINT ( 'NONE',  ( -45.00000000000000000, 0.000000000000000000, 0.000000000000000000 ) ) ;
#32266 = CARTESIAN_POINT ( 'NONE',  ( -5.021133111224989953, -3.725253662474300231, -87.50000000000000000 ) ) ;
#32268 = AXIS2_PLACEMENT_3D ( 'NONE', #18047, #10006, #13043 ) ;
#32269 = VERTEX_POINT ( 'NONE', #26218 ) ;
#32270 = CARTESIAN_POINT ( 'NONE',  ( -70.00000000000000000, 4.559999999999909015, 177.7400000000000091 ) ) ;
#32271 = ORIENTED_EDGE ( 'NONE', *, *, #4080, .T. ) ;
#32272 = CIRCLE ( 'NONE', #29439, 2.033421858999711951 ) ;
#32273 = VECTOR ( 'NONE', #4060, 1000.000000000000000 ) ;
#32274 = VERTEX_POINT ( 'NONE', #20888 ) ;
#32275 = CARTESIAN_POINT ( 'NONE',  ( -345.0000000000000000, -135.0000000000000000, 126.0000000000000000 ) ) ;
#32276 = ORIENTED_EDGE ( 'NONE', *, *, #16095, .T. ) ;
#32277 = VERTEX_POINT ( 'NONE', #21059 ) ;
#32278 = LINE ( 'NONE', #10049, #7626 ) ;
#32279 = CARTESIAN_POINT ( 'NONE',  ( -9.978866888775733912, -11.61907005722761532, -67.50000000000000000 ) ) ;
#32280 = FACE_OUTER_BOUND ( 'NONE', #24751, .T. ) ;
#32281 = EDGE_LOOP ( 'NONE', ( #32293, #34433, #21868, #29656, #25181, #31831 ) ) ;
#32282 = ORIENTED_EDGE ( 'NONE', *, *, #3704, .F. ) ;
#32283 = CARTESIAN_POINT ( 'NONE',  ( -365.0000000000000000, 130.9999999999999716, 128.0000000000000000 ) ) ;
#32284 = LINE ( 'NONE', #10766, #28311 ) ;
#32285 = EDGE_CURVE ( 'NONE', #16248, #10505, #5026, .T. ) ;
#32286 = FACE_OUTER_BOUND ( 'NONE', #21073, .T. ) ;
#32287 = CARTESIAN_POINT ( 'NONE',  ( 11.99999999999999645, 144.9999999999999716, 187.0000000000000000 ) ) ;
#32288 = ORIENTED_EDGE ( 'NONE', *, *, #31682, .T. ) ;
#32289 = CARTESIAN_POINT ( 'NONE',  ( 19.99999999999998934, -145.0000000000000000, -186.9999999999999716 ) ) ;
#32290 = EDGE_CURVE ( 'NONE', #693, #29128, #7611, .T. ) ;
#32291 = VECTOR ( 'NONE', #9457, 1000.000000000000000 ) ;
#32292 = DIRECTION ( 'NONE',  ( -1.000000000000000000, -0.000000000000000000, 0.000000000000000000 ) ) ;
#32293 = ORIENTED_EDGE ( 'NONE', *, *, #17058, .F. ) ;
#32294 = PRODUCT_DEFINITION ( 'UNKNOWN', '', #15587, #24216 ) ;
#32295 = DIRECTION ( 'NONE',  ( 1.232595164407830946E-32, 3.421138828918010427E-49, -1.000000000000000000 ) ) ;
#32296 = DIRECTION ( 'NONE',  ( -1.000000000000000000, -0.000000000000000000, -0.000000000000000000 ) ) ;
#32297 = LINE ( 'NONE', #17627, #10078 ) ;
#32298 = EDGE_LOOP ( 'NONE', ( #22764, #27100, #12924, #8016 ) ) ;
#32299 = DIRECTION ( 'NONE',  ( 1.000000000000000000, 0.000000000000000000, 0.000000000000000000 ) ) ;
#32300 = ORIENTED_EDGE ( 'NONE', *, *, #5379, .F. ) ;
#32301 = VECTOR ( 'NONE', #23315, 1000.000000000000000 ) ;
#32302 = VECTOR ( 'NONE', #21869, 1000.000000000000000 ) ;
#32303 = DIRECTION ( 'NONE',  ( 0.000000000000000000, 0.000000000000000000, 1.000000000000000000 ) ) ;
#32304 = ORIENTED_EDGE ( 'NONE', *, *, #232, .F. ) ;
#32306 = FACE_OUTER_BOUND ( 'NONE', #13684, .T. ) ;
#32305 = LINE ( 'NONE', #7745, #23350 ) ;
#32307 = DIRECTION ( 'NONE',  ( 0.000000000000000000, 0.000000000000000000, -1.000000000000000000 ) ) ;
#32308 = CIRCLE ( 'NONE', #22081, 2.000000000000001776 ) ;
#32309 = ORIENTED_EDGE ( 'NONE', *, *, #31304, .T. ) ;
#32310 = CARTESIAN_POINT ( 'NONE',  ( 2.789999999999999147, -20.92506858792771851, 22.14933852381669510 ) ) ;
#32311 = CARTESIAN_POINT ( 'NONE',  ( 2.604019738671253137, 26.80718912072147120, 17.98567582844242807 ) ) ;
#32312 = VERTEX_POINT ( 'NONE', #17895 ) ;
#32313 = CIRCLE ( 'NONE', #9617, 3.999999999999976019 ) ;
#32314 = DIRECTION ( 'NONE',  ( -7.893605728314051750E-14, 1.618803117314786530E-15, 1.000000000000000000 ) ) ;
#32315 = ORIENTED_EDGE ( 'NONE', *, *, #25953, .F. ) ;
#32316 = CARTESIAN_POINT ( 'NONE',  ( -103.3063056233373089, 4.837773223901916886, 5.733537676439135033 ) ) ;
#32317 = VERTEX_POINT ( 'NONE', #23557 ) ;
#32318 = CARTESIAN_POINT ( 'NONE',  ( -0.000000000000000000, 0.000000000000000000, 57.49999999999999289 ) ) ;
#32319 = DIRECTION ( 'NONE',  ( -1.232595164407830946E-32, -3.421138828918010427E-49, 1.000000000000000000 ) ) ;
#32320 = VECTOR ( 'NONE', #34298, 1000.000000000000000 ) ;
#32321 = CARTESIAN_POINT ( 'NONE',  ( -99.88497961182920903, -0.1727115935459978269, -7.500000000000000888 ) ) ;
#32322 = CARTESIAN_POINT ( 'NONE',  ( -6.500000000000000000, 0.000000000000000000, 0.000000000000000000 ) ) ;
#32323 = VERTEX_POINT ( 'NONE', #10030 ) ;
#32324 = ORIENTED_EDGE ( 'NONE', *, *, #15479, .T. ) ;
#32325 = PRODUCT_DEFINITION_SHAPE ( 'NONE', 'NONE',  #35242 ) ;
#32326 = ORIENTED_EDGE ( 'NONE', *, *, #33541, .F. ) ;
#32327 = DIRECTION ( 'NONE',  ( -1.000000000000000000, -0.000000000000000000, -0.000000000000000000 ) ) ;
#32328 = DIRECTION ( 'NONE',  ( 0.000000000000000000, 0.000000000000000000, 1.000000000000000000 ) ) ;
#32329 = EDGE_CURVE ( 'NONE', #173, #9401, #15922, .T. ) ;
#32330 = CARTESIAN_POINT ( 'NONE',  ( 2.790000000000000924, 9.539392014169456147, 3.000000000000000000 ) ) ;
#32331 = CIRCLE ( 'NONE', #7296, 32.54542015209056416 ) ;
#32332 = CARTESIAN_POINT ( 'NONE',  ( -5.210000000000000853, 0.000000000000000000, 0.000000000000000000 ) ) ;
#32333 = CARTESIAN_POINT ( 'NONE',  ( 2.604019717250312560, 4.859980099383894192, -31.91379830674618390 ) ) ;
#32334 = DIRECTION ( 'NONE',  ( 0.000000000000000000, 0.000000000000000000, 1.000000000000000000 ) ) ;
#32335 = CARTESIAN_POINT ( 'NONE',  ( -8.000000000000000000, 0.000000000000000000, 0.000000000000000000 ) ) ;
#32336 = VERTEX_POINT ( 'NONE', #2359 ) ;
#32337 = EDGE_CURVE ( 'NONE', #17138, #4500, #29064, .T. ) ;
#32338 = LINE ( 'NONE', #10466, #364 ) ;
#32339 = EDGE_CURVE ( 'NONE', #18246, #14020, #6932, .T. ) ;
#32340 = CARTESIAN_POINT ( 'NONE',  ( -12.00000000000001243, 144.9999999999999147, 194.9999999999999716 ) ) ;
#32341 = DIRECTION ( 'NONE',  ( 0.000000000000000000, 1.000000000000000000, 0.000000000000000000 ) ) ;
#32342 = ORIENTED_EDGE ( 'NONE', *, *, #6255, .T. ) ;
#32343 = VECTOR ( 'NONE', #11251, 1000.000000000000000 ) ;
#32344 = EDGE_CURVE ( 'NONE', #20271, #33601, #34595, .T. ) ;
#32345 = PLANE ( 'NONE',  #18388 ) ;
#32346 = ORIENTED_EDGE ( 'NONE', *, *, #11704, .F. ) ;
#32347 = CARTESIAN_POINT ( 'NONE',  ( -99.88497961182919482, 0.3368795255050330839, -12.50000000000000178 ) ) ;
#32348 = ADVANCED_FACE ( 'NONE', ( #10206 ), #29253, .F. ) ;
#32349 = FACE_OUTER_BOUND ( 'NONE', #30219, .T. ) ;
#32350 = AXIS2_PLACEMENT_3D ( 'NONE', #24041, #13215, #3823 ) ;
#32351 = ORIENTED_EDGE ( 'NONE', *, *, #31804, .T. ) ;
#32352 = DIRECTION ( 'NONE',  ( 0.000000000000000000, 0.000000000000000000, 1.000000000000000000 ) ) ;
#32353 = CARTESIAN_POINT ( 'NONE',  ( 3.235562306570555532E-30, -5.758675521474015291, -67.50000000000000000 ) ) ;
#32354 = DIRECTION ( 'NONE',  ( 1.000000000000000000, 0.000000000000000000, 0.000000000000000000 ) ) ;
#32355 = ORIENTED_EDGE ( 'NONE', *, *, #7180, .F. ) ;
#32356 = AXIS2_PLACEMENT_3D ( 'NONE', #33526, #9142, #32816 ) ;
#32357 = ORIENTED_EDGE ( 'NONE', *, *, #14858, .T. ) ;
#32358 = DIRECTION ( 'NONE',  ( 8.207130398226635590E-15, 4.027475412456323609E-14, 0.9999999999999998890 ) ) ;
#32359 = CARTESIAN_POINT ( 'NONE',  ( 31.83311414508813897, -6.771795677801486057, 68.31122994652405112 ) ) ;
#32360 = VERTEX_POINT ( 'NONE', #4494 ) ;
#32361 = DIRECTION ( 'NONE',  ( -0.000000000000000000, 1.836970198721029934E-16, -1.000000000000000000 ) ) ;
#32362 = CYLINDRICAL_SURFACE ( 'NONE', #27171, 2.000000000000001776 ) ;
#32363 = AXIS2_PLACEMENT_3D ( 'NONE', #25104, #14806, #739 ) ;
#32364 = CARTESIAN_POINT ( 'NONE',  ( -8.271081742788348749E-14, -25.79732705422383177, -16.24908268024335101 ) ) ;
#32365 = CARTESIAN_POINT ( 'NONE',  ( 110.7380848894536598, -0.3983872338823410408, 7.499999999999998224 ) ) ;
#32366 = ITEM_DEFINED_TRANSFORMATION ( 'NONE', 'NONE', #24600,  #28566 ) ;
#32367 = VERTEX_POINT ( 'NONE', #15742 ) ;
#32368 = CARTESIAN_POINT ( 'NONE',  ( 2.789999999999999147, 0.000000000000000000, 0.000000000000000000 ) ) ;
#32370 = CARTESIAN_POINT ( 'NONE',  ( -143.0000000000000568, -12.50000000000001066, 1.224646799147353217E-14 ) ) ;
#32369 = CARTESIAN_POINT ( 'NONE',  ( -99.88497961182919482, 6.264093345946822590E-16, 57.49999999999999289 ) ) ;
#32371 = EDGE_LOOP ( 'NONE', ( #15335, #30363, #14301, #33262 ) ) ;
#32372 = ORIENTED_EDGE ( 'NONE', *, *, #8282, .T. ) ;
#32373 = CARTESIAN_POINT ( 'NONE',  ( -12.00000000000001066, 140.9999999999999716, -155.0000000000000000 ) ) ;
#32374 = ORIENTED_EDGE ( 'NONE', *, *, #30869, .T. ) ;
#32375 = LINE ( 'NONE', #18706, #31189 ) ;
#32376 = EDGE_CURVE ( 'NONE', #31497, #16394, #15384, .T. ) ;
#32377 = CARTESIAN_POINT ( 'NONE',  ( -418.0000000000000000, 105.0000000000000142, 107.9999999999999858 ) ) ;
#32378 = ORIENTED_EDGE ( 'NONE', *, *, #13517, .F. ) ;
#32379 = CIRCLE ( 'NONE', #11936, 7.999999999999979572 ) ;
#32380 = ORIENTED_EDGE ( 'NONE', *, *, #12907, .F. ) ;
#32381 = DIRECTION ( 'NONE',  ( -0.000000000000000000, -0.000000000000000000, -1.000000000000000000 ) ) ;
#32382 = EDGE_CURVE ( 'NONE', #14594, #2181, #27627, .T. ) ;
#32383 = EDGE_CURVE ( 'NONE', #29500, #5880, #235, .T. ) ;
#32384 = CARTESIAN_POINT ( 'NONE',  ( 0.8386200322165885401, -14.95253250404442902, -1.101454001170013353 ) ) ;
#32385 = VERTEX_POINT ( 'NONE', #13587 ) ;
#32386 = CARTESIAN_POINT ( 'NONE',  ( -12.00000000000001066, -141.0000000000000000, -154.9999999999999716 ) ) ;
#32387 = CARTESIAN_POINT ( 'NONE',  ( 11.99999999999995559, -134.9999999999999716, -154.9999999999999716 ) ) ;
#32388 = DIRECTION ( 'NONE',  ( -1.000000000000000000, -0.000000000000000000, 0.000000000000000000 ) ) ;
#32389 = DIRECTION ( 'NONE',  ( 0.000000000000000000, 0.000000000000000000, 1.000000000000000000 ) ) ;
#32390 =( REPRESENTATION_RELATIONSHIP ('NONE','NONE', #23037, #15767 ) REPRESENTATION_RELATIONSHIP_WITH_TRANSFORMATION ( #12784 )SHAPE_REPRESENTATION_RELATIONSHIP( ) );
#32391 = DIRECTION ( 'NONE',  ( 0.000000000000000000, 1.000000000000000000, 0.000000000000000000 ) ) ;
#32392 = FACE_OUTER_BOUND ( 'NONE', #6920, .T. ) ;
#32393 = CARTESIAN_POINT ( 'NONE',  ( 2.765921099433441555, 4.286445725888036407, 30.79383171238946204 ) ) ;
#32394 = EDGE_CURVE ( 'NONE', #20123, #5102, #10912, .T. ) ;
#32395 = ORIENTED_EDGE ( 'NONE', *, *, #32145, .F. ) ;
#32396 = DIRECTION ( 'NONE',  ( -1.000000000000000000, 0.000000000000000000, 0.000000000000000000 ) ) ;
#32397 = DIRECTION ( 'NONE',  ( -1.000000000000000000, 6.990337062275415289E-15, 6.982748503361810019E-15 ) ) ;
#32398 = PRODUCT_DEFINITION_CONTEXT ( 'detailed design', #18758, 'design' ) ;
#32399 = VERTEX_POINT ( 'NONE', #16268 ) ;
#32401 = ORIENTED_EDGE ( 'NONE', *, *, #16453, .T. ) ;
#32400 = EDGE_CURVE ( 'NONE', #11811, #17161, #19461, .T. ) ;
#32402 = VECTOR ( 'NONE', #22089, 1000.000000000000000 ) ;
#32403 = EDGE_CURVE ( 'NONE', #12523, #34039, #4713, .T. ) ;
#32404 = DIRECTION ( 'NONE',  ( 0.000000000000000000, -1.000000000000000000, 0.000000000000000000 ) ) ;
#32405 = SHAPE_DEFINITION_REPRESENTATION ( #25113, #23037 ) ;
#32406 = ORIENTED_EDGE ( 'NONE', *, *, #1011, .T. ) ;
#32407 = CARTESIAN_POINT ( 'NONE',  ( -442.0000000000000000, -125.0000000000000000, -109.9999999999999574 ) ) ;
#32408 = CYLINDRICAL_SURFACE ( 'NONE', #28401, 1.999999999999999556 ) ;
#32409 = ADVANCED_FACE ( 'NONE', ( #5381 ), #24098, .T. ) ;
#32410 = CONTEXT_DEPENDENT_SHAPE_REPRESENTATION ( #34009, #30691 ) ;
#32411 = DIRECTION ( 'NONE',  ( 0.000000000000000000, 1.000000000000000000, 0.000000000000000000 ) ) ;
#32413 = VERTEX_POINT ( 'NONE', #29598 ) ;
#32412 = AXIS2_PLACEMENT_3D ( 'NONE', #10277, #20616, #31980 ) ;
#32414 = VERTEX_POINT ( 'NONE', #24417 ) ;
#32415 = CARTESIAN_POINT ( 'NONE',  ( -12.25939112814508825, 30.14816249862104769, -36.68877005347593467 ) ) ;
#32416 = DIRECTION ( 'NONE',  ( -1.000000000000000000, -0.000000000000000000, -0.000000000000000000 ) ) ;
#32417 = FACE_BOUND ( 'NONE', #31742, .T. ) ;
#32418 = DIRECTION ( 'NONE',  ( 0.000000000000000000, -1.131431318426415506E-52, -1.000000000000000000 ) ) ;
#32419 = CARTESIAN_POINT ( 'NONE',  ( -9.978866888775733912, -13.65249191622732461, -87.50000000000000000 ) ) ;
#32420 = ORIENTED_EDGE ( 'NONE', *, *, #7336, .F. ) ;
#32421 = CARTESIAN_POINT ( 'NONE',  ( -414.0000000000000568, 113.0000000000000000, -175.0000000000000000 ) ) ;
#32422 = PLANE ( 'NONE',  #15152 ) ;
#32423 = DIRECTION ( 'NONE',  ( 1.000000000000000000, 3.040835319149746090E-31, 1.232595164407830946E-32 ) ) ;
#32424 = ADVANCED_FACE ( 'NONE', ( #5196 ), #16443, .F. ) ;
#32425 = CIRCLE ( 'NONE', #27968, 34.41491905851385269 ) ;
#32426 = CARTESIAN_POINT ( 'NONE',  ( 0.02407890056655825201, -23.70329957282570632, -20.11932597908854703 ) ) ;
#32427 = PRESENTATION_STYLE_ASSIGNMENT (( #13754 ) ) ;
#32428 = AXIS2_PLACEMENT_3D ( 'NONE', #15810, #10449, #1564 ) ;
#32429 = CARTESIAN_POINT ( 'NONE',  ( -500.0000000000000000, -113.0000000000000000, 187.0000000000000000 ) ) ;
#32431 = CARTESIAN_POINT ( 'NONE',  ( 19.99999999999998934, 75.55999999999990280, 172.9900000000000091 ) ) ;
#32430 = CARTESIAN_POINT ( 'NONE',  ( 26.04754872656010178, -19.51229300245306320, 68.31122994652405112 ) ) ;
#32432 = ORIENTED_EDGE ( 'NONE', *, *, #3450, .F. ) ;
#32433 = DIRECTION ( 'NONE',  ( -3.040835319149746528E-31, -1.000000000000000000, 0.000000000000000000 ) ) ;
#32434 = CARTESIAN_POINT ( 'NONE',  ( 110.7277013283863170, -0.3974226492620277496, -7.492047161373153408 ) ) ;
#32435 = ORIENTED_EDGE ( 'NONE', *, *, #31658, .F. ) ;
#32436 = VECTOR ( 'NONE', #25865, 1000.000000000000000 ) ;
#32437 = PLANE ( 'NONE',  #20042 ) ;
#32438 = AXIS2_PLACEMENT_3D ( 'NONE', #10786, #13109, #23941 ) ;
#32439 = ORIENTED_EDGE ( 'NONE', *, *, #8934, .T. ) ;
#32440 = EDGE_CURVE ( 'NONE', #8699, #29138, #14531, .T. ) ;
#32441 = EDGE_CURVE ( 'NONE', #23190, #21389, #6474, .T. ) ;
#32442 = EDGE_LOOP ( 'NONE', ( #6596, #26758, #22261, #24228 ) ) ;
#32443 = PLANE ( 'NONE',  #16186 ) ;
#32444 = EDGE_LOOP ( 'NONE', ( #28685, #14427, #5456, #3708, #13645, #33548, #26612, #33777, #25625 ) ) ;
#32445 = ORIENTED_EDGE ( 'NONE', *, *, #12230, .T. ) ;
#32446 = VECTOR ( 'NONE', #7727, 1000.000000000000000 ) ;
#32447 = LINE ( 'NONE', #15574, #13926 ) ;
#32448 = AXIS2_PLACEMENT_3D ( 'NONE', #18431, #29273, #18779 ) ;
#32449 = DIRECTION ( 'NONE',  ( 0.000000000000000000, 1.000000000000000000, 5.053935297177146739E-49 ) ) ;
#32450 = CARTESIAN_POINT ( 'NONE',  ( -410.0000000000000568, -112.9999999999999858, -174.9999999999999716 ) ) ;
#32451 = ORIENTED_EDGE ( 'NONE', *, *, #5810, .F. ) ;
#32452 = VERTEX_POINT ( 'NONE', #19116 ) ;
#32453 = CARTESIAN_POINT ( 'NONE',  ( -441.9999999999999432, 105.0000000000000000, 135.9999999999999716 ) ) ;
#32454 = EDGE_CURVE ( 'NONE', #28176, #10430, #27455, .T. ) ;
#32455 = PRESENTATION_STYLE_ASSIGNMENT (( #34620 ) ) ;
#32456 = CARTESIAN_POINT ( 'NONE',  ( 105.9525633024387332, -5.661646449284257976, -11.14439484353662735 ) ) ;
#32457 = LINE ( 'NONE', #24094, #2875 ) ;
#32458 = EDGE_LOOP ( 'NONE', ( #23324, #27380 ) ) ;
#32459 = CARTESIAN_POINT ( 'NONE',  ( -35.00000000000000000, 3.353962854566122864, 15.81122994652406355 ) ) ;
#32460 = VECTOR ( 'NONE', #2481, 1000.000000000000000 ) ;
#32461 = DIRECTION ( 'NONE',  ( 0.000000000000000000, 1.836970198721029688E-16, -1.000000000000000000 ) ) ;
#32462 = ORIENTED_EDGE ( 'NONE', *, *, #29202, .T. ) ;
#32463 = VECTOR ( 'NONE', #12113, 1000.000000000000000 ) ;
#32464 = AXIS2_PLACEMENT_3D ( 'NONE', #34247, #9862, #20727 ) ;
#32465 = VECTOR ( 'NONE', #30654, 1000.000000000000000 ) ;
#32466 = DIRECTION ( 'NONE',  ( 0.000000000000000000, -0.7071067811865489050, -0.7071067811865462405 ) ) ;
#32467 = DIRECTION ( 'NONE',  ( 0.000000000000000000, 1.000000000000000000, -1.310824597558155437E-49 ) ) ;
#32468 = DIRECTION ( 'NONE',  ( 0.000000000000000000, -1.000000000000000000, -2.465190328815662439E-32 ) ) ;
#32469 = DIRECTION ( 'NONE',  ( 0.000000000000000000, 0.000000000000000000, 1.000000000000000000 ) ) ;
#32470 = EDGE_LOOP ( 'NONE', ( #7362, #14559, #12406, #31964, #7541, #20333, #34295, #27918 ) ) ;
#32471 = DIRECTION ( 'NONE',  ( 1.000000000000000000, 0.000000000000000000, 0.000000000000000000 ) ) ;
#32472 = VERTEX_POINT ( 'NONE', #13761 ) ;
#32473 = EDGE_CURVE ( 'NONE', #32015, #31695, #5900, .T. ) ;
#32474 =( LENGTH_UNIT ( ) NAMED_UNIT ( * ) SI_UNIT ( .MILLI., .METRE. ) );
#32475 = DIRECTION ( 'NONE',  ( -1.000000000000000000, -0.000000000000000000, 0.000000000000000000 ) ) ;
#32476 = AXIS2_PLACEMENT_3D ( 'NONE', #19918, #873, #20444 ) ;
#32477 = ORIENTED_EDGE ( 'NONE', *, *, #15862, .T. ) ;
#32478 = CARTESIAN_POINT ( 'NONE',  ( -34.04247984038124031, 16.56841925338180488, 68.31122994652405112 ) ) ;
#32479 = CARTESIAN_POINT ( 'NONE',  ( 3.235562306570555532E-30, -5.758675521474015291, -67.50000000000000000 ) ) ;
#32480 = EDGE_CURVE ( 'NONE', #9466, #6872, #24779, .T. ) ;
#32481 = ORIENTED_EDGE ( 'NONE', *, *, #18677, .F. ) ;
#32482 = ADVANCED_FACE ( 'NONE', ( #16802 ), #26365, .T. ) ;
#32483 = VECTOR ( 'NONE', #21943, 1000.000000000000000 ) ;
#32484 = EDGE_CURVE ( 'NONE', #30633, #28125, #32051, .T. ) ;
#32486 = ORIENTED_EDGE ( 'NONE', *, *, #13949, .F. ) ;
#32485 = VECTOR ( 'NONE', #22083, 1000.000000000000114 ) ;
#32487 = DIRECTION ( 'NONE',  ( 0.000000000000000000, 0.000000000000000000, 1.000000000000000000 ) ) ;
#32488 = CARTESIAN_POINT ( 'NONE',  ( -18.45373714011839539, 26.80790850550480542, 68.31122994652405112 ) ) ;
#32489 = ORIENTED_EDGE ( 'NONE', *, *, #10253, .F. ) ;
#32490 = VERTEX_POINT ( 'NONE', #3244 ) ;
#32491 = VECTOR ( 'NONE', #7082, 1000.000000000000000 ) ;
#32492 = LINE ( 'NONE', #7760, #32626 ) ;
#32493 = DIRECTION ( 'NONE',  ( 0.000000000000000000, 0.000000000000000000, -1.000000000000000000 ) ) ;
#32494 = DIRECTION ( 'NONE',  ( -1.000000000000000000, -3.040835319149746090E-31, -1.232595164407830946E-32 ) ) ;
#32495 = CARTESIAN_POINT ( 'NONE',  ( 0.000000000000000000, 0.000000000000000000, 3.180000000000000160 ) ) ;
#32496 = VERTEX_POINT ( 'NONE', #30297 ) ;
#32497 = VERTEX_POINT ( 'NONE', #29954 ) ;
#32498 = DIRECTION ( 'NONE',  ( 0.000000000000000000, 0.000000000000000000, -1.000000000000000000 ) ) ;
#32499 = CARTESIAN_POINT ( 'NONE',  ( -15.99999999999998579, 4.559999999999908127, -172.9900000000000091 ) ) ;
#32500 = DIRECTION ( 'NONE',  ( -1.000000000000000000, 0.000000000000000000, 0.000000000000000000 ) ) ;
#32502 = CIRCLE ( 'NONE', #29671, 2.525000000000001243 ) ;
#32501 = CARTESIAN_POINT ( 'NONE',  ( -418.0000000000000000, -105.0000000000000142, 162.9999999999999716 ) ) ;
#32503 = CARTESIAN_POINT ( 'NONE',  ( -349.0000000000000000, -125.0000000000000284, 183.0000000000000000 ) ) ;
#32504 = CARTESIAN_POINT ( 'NONE',  ( 15.99999999999998579, -137.0000000000000000, 174.9999999999999432 ) ) ;
#32505 = DIRECTION ( 'NONE',  ( 1.000000000000000000, 0.000000000000000000, 0.000000000000000000 ) ) ;
#32506 = DIRECTION ( 'NONE',  ( 0.000000000000000000, -1.000000000000000000, -0.000000000000000000 ) ) ;
#32507 = ORIENTED_EDGE ( 'NONE', *, *, #17340, .T. ) ;
#32508 = DIRECTION ( 'NONE',  ( -1.000000000000000000, 0.000000000000000000, 0.000000000000000000 ) ) ;
#32509 = CARTESIAN_POINT ( 'NONE',  ( -365.0000000000000000, -117.0000000000000000, 126.0000000000000000 ) ) ;
#32510 = CARTESIAN_POINT ( 'NONE',  ( 2.765921099433441999, -0.3931553186915530129, 31.08824725498900321 ) ) ;
#32511 = VERTEX_POINT ( 'NONE', #28128 ) ;
#32512 = VECTOR ( 'NONE', #30863, 1000.000000000000000 ) ;
#32513 = CIRCLE ( 'NONE', #26271, 2.033421858999711951 ) ;
#32514 = CARTESIAN_POINT ( 'NONE',  ( -418.0000000000000000, 105.0000000000000142, -175.0000000000000000 ) ) ;
#32515 = EDGE_LOOP ( 'NONE', ( #22086, #26925, #33039, #31160, #26474, #24888 ) ) ;
#32516 = CARTESIAN_POINT ( 'NONE',  ( -441.9999999999999432, -105.0000000000000142, 190.9999999999999716 ) ) ;
#32517 = CARTESIAN_POINT ( 'NONE',  ( 2.765921099433443331, 18.59128259035506758, -24.91982945642901726 ) ) ;
#32518 = EDGE_LOOP ( 'NONE', ( #2980, #14413, #13320, #26988, #24785, #24184, #33387, #17564 ) ) ;
#32519 = ADVANCED_FACE ( 'NONE', ( #5545 ), #27274, .T. ) ;
#32520 = DIRECTION ( 'NONE',  ( 0.000000000000000000, -1.224646799147353207E-16, 1.000000000000000000 ) ) ;
#32521 = DIRECTION ( 'NONE',  ( -0.000000000000000000, -0.000000000000000000, -1.000000000000000000 ) ) ;
#32522 = DIRECTION ( 'NONE',  ( -1.000000000000000000, 0.000000000000000000, 0.000000000000000000 ) ) ;
#32523 = EDGE_CURVE ( 'NONE', #30447, #18562, #6245, .T. ) ;
#32524 = ORIENTED_EDGE ( 'NONE', *, *, #19016, .T. ) ;
#32526 = ORIENTED_EDGE ( 'NONE', *, *, #8099, .T. ) ;
#32525 = EDGE_CURVE ( 'NONE', #33041, #18637, #23522, .T. ) ;
#32527 = CARTESIAN_POINT ( 'NONE',  ( 819.0176343340062886, 1330.073034875954363, 1753.598338701303419 ) ) ;
#32528 = B_SPLINE_CURVE_WITH_KNOTS ( 'NONE', 3,
 ( #23844, #29007, #21179, #1956, #12834, #23674 ),
 .UNSPECIFIED., .F., .F.,
 ( 4, 2, 4 ),
 ( 2.178692866010994808E-07, 0.001873416183138254271, 0.003746614496989907669 ),
 .UNSPECIFIED. ) ;
#32529 = CARTESIAN_POINT ( 'NONE',  ( -355.0000000000000000, 130.9999999999999716, 111.9999999999999858 ) ) ;
#32530 = ADVANCED_FACE ( 'NONE', ( #16979 ), #4104, .T. ) ;
#32531 = EDGE_LOOP ( 'NONE', ( #30238, #3562, #21649, #32372 ) ) ;
#32532 = DIRECTION ( 'NONE',  ( 0.000000000000000000, 0.000000000000000000, -1.000000000000000000 ) ) ;
#32533 =( GEOMETRIC_REPRESENTATION_CONTEXT ( 3 ) GLOBAL_UNCERTAINTY_ASSIGNED_CONTEXT ( ( #31306 ) ) GLOBAL_UNIT_ASSIGNED_CONTEXT ( ( #16628, #17336, #27461 ) ) REPRESENTATION_CONTEXT ( 'NONE', 'WORKASPACE' ) );
#32534 = VECTOR ( 'NONE', #5500, 1000.000000000000000 ) ;
#32535 = LINE ( 'NONE', #10675, #15047 ) ;
#32536 = CARTESIAN_POINT ( 'NONE',  ( -108.8320610496387246, -3.403480489512942686, 6.688370467007148434 ) ) ;
#32538 = VECTOR ( 'NONE', #5548, 1000.000000000000000 ) ;
#32537 = ITEM_DEFINED_TRANSFORMATION ( 'NONE', 'NONE', #11578,  #28566 ) ;
#32539 = ORIENTED_EDGE ( 'NONE', *, *, #27113, .F. ) ;
#32540 = CIRCLE ( 'NONE', #20073, 7.999999999999979572 ) ;
#32541 = VERTEX_POINT ( 'NONE', #8757 ) ;
#32542 = DIRECTION ( 'NONE',  ( 0.000000000000000000, 1.131431318426415506E-52, 1.000000000000000000 ) ) ;
#32543 = EDGE_CURVE ( 'NONE', #32705, #33757, #11625, .T. ) ;
#32545 = CARTESIAN_POINT ( 'NONE',  ( -70.00000000000000000, 4.559999999999908127, -177.7400000000000091 ) ) ;
#32544 = DIRECTION ( 'NONE',  ( -0.7071067811865513475, 0.000000000000000000, 0.7071067811865435759 ) ) ;
#32546 = ORIENTED_EDGE ( 'NONE', *, *, #15449, .F. ) ;
#32547 = VERTEX_POINT ( 'NONE', #8941 ) ;
#32548 = CARTESIAN_POINT ( 'NONE',  ( 2.719010745927727513, -28.42160548755730787, 14.02701190433877265 ) ) ;
#32549 = ORIENTED_EDGE ( 'NONE', *, *, #15853, .T. ) ;
#32550 = DIRECTION ( 'NONE',  ( -0.000000000000000000, 1.836970198721029934E-16, -1.000000000000000000 ) ) ;
#32551 = CARTESIAN_POINT ( 'NONE',  ( 2.789999999999999147, 0.000000000000000000, 0.000000000000000000 ) ) ;
#32552 = ORIENTED_EDGE ( 'NONE', *, *, #26914, .T. ) ;
#32553 = VERTEX_POINT ( 'NONE', #11435 ) ;
#32554 = DIRECTION ( 'NONE',  ( -1.000000000000000000, -0.000000000000000000, -0.000000000000000000 ) ) ;
#32555 = CARTESIAN_POINT ( 'NONE',  ( -355.0000000000000000, 130.9999999999999716, 126.0000000000000000 ) ) ;
#32556 = ORIENTED_EDGE ( 'NONE', *, *, #29558, .F. ) ;
#32557 = CARTESIAN_POINT ( 'NONE',  ( 1.040000000000001590, 32.09669216789235691, 12.41728656686385968 ) ) ;
#32558 = DIRECTION ( 'NONE',  ( 0.000000000000000000, -1.836970198721030181E-16, 1.000000000000000000 ) ) ;
#32559 = DIRECTION ( 'NONE',  ( -1.000000000000000000, -0.000000000000000000, -0.000000000000000000 ) ) ;
#32561 = LINE ( 'NONE', #24205, #14588 ) ;
#32560 = AXIS2_PLACEMENT_3D ( 'NONE', #15891, #24215, #194 ) ;
#32562 = CIRCLE ( 'NONE', #12694, 30.47050528711512030 ) ;
#32563 = CIRCLE ( 'NONE', #21194, 10.00000000000000888 ) ;
#32564 = VECTOR ( 'NONE', #34589, 1000.000000000000000 ) ;
#32565 = FACE_OUTER_BOUND ( 'NONE', #27320, .T. ) ;
#32566 = DIRECTION ( 'NONE',  ( 1.000000000000000000, 0.000000000000000000, 0.000000000000000000 ) ) ;
#32567 = DIRECTION ( 'NONE',  ( 0.000000000000000000, 0.000000000000000000, 1.000000000000000000 ) ) ;
#32568 = ORIENTED_EDGE ( 'NONE', *, *, #28641, .T. ) ;
#32569 = LINE ( 'NONE', #19422, #17185 ) ;
#32570 = DIRECTION ( 'NONE',  ( -6.982962677686339286E-15, 6.990357483066008800E-15, -1.000000000000000000 ) ) ;
#32571 = ADVANCED_FACE ( 'NONE', ( #25123 ), #33142, .T. ) ;
#32572 = VERTEX_POINT ( 'NONE', #14472 ) ;
#32573 = ORIENTED_EDGE ( 'NONE', *, *, #33140, .T. ) ;
#32574 = ADVANCED_FACE ( 'NONE', ( #19979 ), #17510, .F. ) ;
#32575 = AXIS2_PLACEMENT_3D ( 'NONE', #19851, #976, #33531 ) ;
#32576 = EDGE_CURVE ( 'NONE', #27211, #26816, #14994, .T. ) ;
#32577 = CARTESIAN_POINT ( 'NONE',  ( 99.65514493969531884, 2.096151729099205774, 7.203423290846323823 ) ) ;
#32578 = ADVANCED_FACE ( 'NONE', ( #25480 ), #22476, .F. ) ;
#32579 = PRODUCT_CONTEXT ( 'NONE', #23061, 'mechanical' ) ;
#32580 = ORIENTED_EDGE ( 'NONE', *, *, #34974, .F. ) ;
#32581 = CARTESIAN_POINT ( 'NONE',  ( 2.783107618245967085, 20.89684813776040428, -22.72149230800609487 ) ) ;
#32582 = CARTESIAN_POINT ( 'NONE',  ( -19.99999999999998934, -32.99999999999997158, -154.9999999999999716 ) ) ;
#32583 = AXIS2_PLACEMENT_3D ( 'NONE', #25039, #6173, #2809 ) ;
#32584 = CARTESIAN_POINT ( 'NONE',  ( -19.99999999999996092, 125.0000000000000568, 162.9999999999999716 ) ) ;
#32585 = AXIS2_PLACEMENT_3D ( 'NONE', #11668, #22699, #6119 ) ;
#32586 = EDGE_LOOP ( 'NONE', ( #13841, #21128, #2366, #10684, #25057, #8930, #3868, #29525 ) ) ;
#32587 = VERTEX_POINT ( 'NONE', #936 ) ;
#32588 = VECTOR ( 'NONE', #15507, 1000.000000000000000 ) ;
#32589 = CARTESIAN_POINT ( 'NONE',  ( 19.99999999999998224, 134.9999999999998863, 162.9999999999999716 ) ) ;
#32590 = DIRECTION ( 'NONE',  ( -0.6051742151937647973, 0.7960930657056438653, 0.000000000000000000 ) ) ;
#32591 = DIRECTION ( 'NONE',  ( -3.469446951953832974E-18, -1.000000000000000000, -7.888609052210116302E-31 ) ) ;
#32593 = EDGE_CURVE ( 'NONE', #30730, #13606, #33324, .T. ) ;
#32592 = DIRECTION ( 'NONE',  ( -0.000000000000000000, 1.000000000000000000, -0.000000000000000000 ) ) ;
#32594 = DIRECTION ( 'NONE',  ( -1.000000000000000000, 0.000000000000000000, -0.000000000000000000 ) ) ;
#32595 = VERTEX_POINT ( 'NONE', #30660 ) ;
#32596 = DIRECTION ( 'NONE',  ( 2.736911063134582149E-48, -7.888609052210118054E-31, -1.000000000000000000 ) ) ;
#32597 = FACE_OUTER_BOUND ( 'NONE', #8818, .T. ) ;
#32598 = CARTESIAN_POINT ( 'NONE',  ( -10.00000000000000000, 0.000000000000000000, 0.000000000000000000 ) ) ;
#32599 =( REPRESENTATION_RELATIONSHIP ('NONE','NONE', #23037, #28231 ) REPRESENTATION_RELATIONSHIP_WITH_TRANSFORMATION ( #12602 )SHAPE_REPRESENTATION_RELATIONSHIP( ) );
#32600 = B_SPLINE_CURVE_WITH_KNOTS ( 'NONE', 3,
 ( #23879, #26904, #2518, #34748 ),
 .UNSPECIFIED., .F., .F.,
 ( 4, 4 ),
 ( 1.980634265047890748E-07, 0.0006879337600918691668 ),
 .UNSPECIFIED. ) ;
#32601 = DIRECTION ( 'NONE',  ( 0.000000000000000000, 0.000000000000000000, -1.000000000000000000 ) ) ;
#32602 = CARTESIAN_POINT ( 'NONE',  ( -499.9999999999999432, 136.9999999999999432, -187.0000000000000000 ) ) ;
#32604 = DIRECTION ( 'NONE',  ( 0.000000000000000000, -1.131431318426415506E-52, -1.000000000000000000 ) ) ;
#32603 = CARTESIAN_POINT ( 'NONE',  ( 0.006871088337153627955, -23.57967537501776789, 19.92301408446852307 ) ) ;
#32605 = EDGE_CURVE ( 'NONE', #3111, #23519, #21757, .T. ) ;
#32606 = AXIS2_PLACEMENT_3D ( 'NONE', #335, #10669, #14036 ) ;
#32607 = ADVANCED_FACE ( 'NONE', ( #6783 ), #33494, .T. ) ;
#32608 = CARTESIAN_POINT ( 'NONE',  ( 5.021133111224162171, -23.57973016998034765, -67.50000000000000000 ) ) ;
#32609 = VERTEX_POINT ( 'NONE', #25653 ) ;
#32610 = CARTESIAN_POINT ( 'NONE',  ( 3.235562306570555532E-30, 1.325223266901699007E-14, -67.50000000000000000 ) ) ;
#32612 = CARTESIAN_POINT ( 'NONE',  ( 1.749999999999999778, -34.41385771548412720, -0.2702793785573802121 ) ) ;
#32611 = DIRECTION ( 'NONE',  ( -1.000000000000000000, 0.000000000000000000, -0.000000000000000000 ) ) ;
#32613 = AXIS2_PLACEMENT_3D ( 'NONE', #34384, #31867, #7311 ) ;
#32615 = VERTEX_POINT ( 'NONE', #33669 ) ;
#32614 = VECTOR ( 'NONE', #13939, 1000.000000000000000 ) ;
#32616 = ORIENTED_EDGE ( 'NONE', *, *, #10376, .T. ) ;
#32617 = EDGE_CURVE ( 'NONE', #28456, #7179, #17116, .T. ) ;
#32618 = EDGE_CURVE ( 'NONE', #4151, #4421, #1283, .T. ) ;
#32619 = ORIENTED_EDGE ( 'NONE', *, *, #4485, .T. ) ;
#32620 = CARTESIAN_POINT ( 'NONE',  ( -442.0000000000000000, 124.9999999999999574, -187.0000000000000000 ) ) ;
#32621 = VERTEX_POINT ( 'NONE', #28509 ) ;
#32622 = ORIENTED_EDGE ( 'NONE', *, *, #23121, .T. ) ;
#32623 = CARTESIAN_POINT ( 'NONE',  ( 20.89386240318430055, 24.95297350523386015, 68.31122994652405112 ) ) ;
#32624 = B_SPLINE_CURVE_WITH_KNOTS ( 'NONE', 3,
 ( #10928, #16460, #32969, #16818 ),
 .UNSPECIFIED., .F., .F.,
 ( 4, 4 ),
 ( 2.180635439307184488E-07, 0.0006879539277919237373 ),
 .UNSPECIFIED. ) ;
#32625 = EDGE_CURVE ( 'NONE', #7170, #32547, #5905, .T. ) ;
#32626 = VECTOR ( 'NONE', #24131, 1000.000000000000000 ) ;
#32627 = CARTESIAN_POINT ( 'NONE',  ( -145.0000000000000568, -88.29863524074325198, -74.12844257252345415 ) ) ;
#32628 = CARTESIAN_POINT ( 'NONE',  ( -361.0000000000000000, -125.0000000000000284, 126.0000000000000000 ) ) ;
#32629 = VERTEX_POINT ( 'NONE', #12497 ) ;
#32630 = VERTEX_POINT ( 'NONE', #31347 ) ;
#32631 = DIRECTION ( 'NONE',  ( 1.000000000000000000, 3.040835319149746528E-31, 1.232595164407830946E-32 ) ) ;
#32632 = CIRCLE ( 'NONE', #16176, 30.47050528711512030 ) ;
#32633 = CARTESIAN_POINT ( 'NONE',  ( 99.78004831670104124, -2.390228624448383243, -12.27061385718275943 ) ) ;
#32634 = DIRECTION ( 'NONE',  ( 0.000000000000000000, 0.000000000000000000, 1.000000000000000000 ) ) ;
#32635 = VERTEX_POINT ( 'NONE', #9986 ) ;
#32636 = CARTESIAN_POINT ( 'NONE',  ( 11.99999999999999645, 112.9999999999999574, -155.0000000000000000 ) ) ;
#32637 = DIRECTION ( 'NONE',  ( -1.000000000000000000, -0.000000000000000000, -0.000000000000000000 ) ) ;
#32638 = VECTOR ( 'NONE', #7515, 1000.000000000000114 ) ;
#32639 = AXIS2_PLACEMENT_3D ( 'NONE', #30088, #32920, #21555 ) ;
#32640 = CYLINDRICAL_SURFACE ( 'NONE', #16455, 2.524999999999999467 ) ;
#32641 = VERTEX_POINT ( 'NONE', #7473 ) ;
#32642 = VECTOR ( 'NONE', #4505, 1000.000000000000000 ) ;
#32643 = CARTESIAN_POINT ( 'NONE',  ( 15.04122381213380244, 28.86114964982166597, 68.31122994652405112 ) ) ;
#32644 = CARTESIAN_POINT ( 'NONE',  ( 0.02407890056655781832, 4.286445725888479608, -30.79383171238939809 ) ) ;
#32645 = CARTESIAN_POINT ( 'NONE',  ( -19.99999999999998934, -145.0000000000000000, -162.9999999999999432 ) ) ;
#32646 = EDGE_CURVE ( 'NONE', #10891, #3383, #23339, .T. ) ;
#32647 = DIRECTION ( 'NONE',  ( -0.000000000000000000, -0.000000000000000000, 1.000000000000000000 ) ) ;
#32648 = ORIENTED_EDGE ( 'NONE', *, *, #12233, .F. ) ;
#32649 = ADVANCED_FACE ( 'NONE', ( #28679 ), #23690, .T. ) ;
#32650 = DIRECTION ( 'NONE',  ( 0.000000000000000000, -0.000000000000000000, 1.000000000000000000 ) ) ;
#32651 = VERTEX_POINT ( 'NONE', #4804 ) ;
#32653 = SURFACE_SIDE_STYLE ('',( #16136 ) ) ;
#32652 = CARTESIAN_POINT ( 'NONE',  ( 9.199999999999999289, 0.000000000000000000, 0.000000000000000000 ) ) ;
#32654 =( LENGTH_UNIT ( ) NAMED_UNIT ( * ) SI_UNIT ( .MILLI., .METRE. ) );
#32655 = EDGE_CURVE ( 'NONE', #30998, #22969, #9643, .T. ) ;
#32656 = AXIS2_PLACEMENT_3D ( 'NONE', #14491, #6798, #3947 ) ;
#32657 = EDGE_CURVE ( 'NONE', #8838, #25584, #31855, .T. ) ;
#32658 = ORIENTED_EDGE ( 'NONE', *, *, #21255, .T. ) ;
#32659 = LINE ( 'NONE', #32478, #29683 ) ;
#32660 = EDGE_CURVE ( 'NONE', #25172, #19146, #13886, .T. ) ;
#32661 = DIRECTION ( 'NONE',  ( 0.000000000000000000, 1.000000000000000000, 0.000000000000000000 ) ) ;
#32662 = AXIS2_PLACEMENT_3D ( 'NONE', #16731, #22589, #27564 ) ;
#32663 = ORIENTED_EDGE ( 'NONE', *, *, #28807, .T. ) ;
#32664 = ORIENTED_EDGE ( 'NONE', *, *, #2470, .T. ) ;
#32665 = EDGE_LOOP ( 'NONE', ( #9726, #1295, #2029, #13963, #7112, #10009, #5811, #32693 ) ) ;
#32666 = AXIS2_PLACEMENT_3D ( 'NONE', #29384, #2147, #16527 ) ;
#32667 = AXIS2_PLACEMENT_3D ( 'NONE', #24028, #16228, #19246 ) ;
#32668 = VERTEX_POINT ( 'NONE', #18196 ) ;
#32669 = PLANE ( 'NONE',  #1012 ) ;
#32670 = CARTESIAN_POINT ( 'NONE',  ( -107.7224926025144498, 4.333302303957496271, 6.122453330911801217 ) ) ;
#32671 = ORIENTED_EDGE ( 'NONE', *, *, #7106, .T. ) ;
#32672 = VERTEX_POINT ( 'NONE', #34545 ) ;
#32673 = CARTESIAN_POINT ( 'NONE',  ( 11.99999999999999645, -145.0000000000000000, 190.9999999999999716 ) ) ;
#32674 = AXIS2_PLACEMENT_3D ( 'NONE', #3694, #6714, #17610 ) ;
#32675 = CARTESIAN_POINT ( 'NONE',  ( 2.789999999999999591, 30.58654839005191306, -2.143968220813880166 ) ) ;
#32676 = DIRECTION ( 'NONE',  ( -1.000000000000000000, -0.000000000000000000, -0.000000000000000000 ) ) ;
#32677 = PLANE ( 'NONE',  #23889 ) ;
#32678 = VERTEX_POINT ( 'NONE', #15342 ) ;
#32679 = ORIENTED_EDGE ( 'NONE', *, *, #7892, .F. ) ;
#32680 = DIRECTION ( 'NONE',  ( 0.000000000000000000, 0.000000000000000000, -1.000000000000000000 ) ) ;
#32681 = CARTESIAN_POINT ( 'NONE',  ( -20.02113311122478123, 16.12922284503174097, -87.50000000000000000 ) ) ;
#32682 = CARTESIAN_POINT ( 'NONE',  ( 2.789999999999999147, -16.83127206196721914, -25.36297913013192584 ) ) ;
#32683 = CARTESIAN_POINT ( 'NONE',  ( 2.765921099433441999, 7.350529080603541487, 30.20932655202940254 ) ) ;
#32684 = AXIS2_PLACEMENT_3D ( 'NONE', #4466, #32057, #29225 ) ;
#32685 = CYLINDRICAL_SURFACE ( 'NONE', #16230, 34.41491905851385269 ) ;
#32686 = CARTESIAN_POINT ( 'NONE',  ( -418.0000000000000000, 105.0000000000000142, 155.0000000000000000 ) ) ;
#32687 = DIRECTION ( 'NONE',  ( -0.000000000000000000, 1.000000000000000000, -0.000000000000000000 ) ) ;
#32688 = ORIENTED_EDGE ( 'NONE', *, *, #14532, .T. ) ;
#32689 = VECTOR ( 'NONE', #11520, 1000.000000000000000 ) ;
#32690 = TOROIDAL_SURFACE ( 'NONE', #30443, 13.00000000000000000, 1.799999999999999822 ) ;
#32691 = DIRECTION ( 'NONE',  ( -1.000000000000000000, 6.792721752314501023E-48, -3.697785493223492838E-32 ) ) ;
#32692 = CARTESIAN_POINT ( 'NONE',  ( -19.99999999999998934, 134.9999999999998863, 162.9999999999999716 ) ) ;
#32693 = ORIENTED_EDGE ( 'NONE', *, *, #30328, .T. ) ;
#32694 = EDGE_CURVE ( 'NONE', #15311, #423, #4617, .T. ) ;
#32695 = PLANE ( 'NONE',  #8105 ) ;
#32696 = ORIENTED_EDGE ( 'NONE', *, *, #26275, .F. ) ;
#32697 = EDGE_CURVE ( 'NONE', #6316, #20279, #10162, .T. ) ;
#32698 = AXIS2_PLACEMENT_3D ( 'NONE', #30211, #5815, #27543 ) ;
#32699 = AXIS2_PLACEMENT_3D ( 'NONE', #29077, #26762, #7012 ) ;
#32700 = DIRECTION ( 'NONE',  ( -1.000000000000000000, -0.000000000000000000, -0.000000000000000000 ) ) ;
#32701 = VERTEX_POINT ( 'NONE', #18024 ) ;
#32703 = CIRCLE ( 'NONE', #12279, 15.69999999999999929 ) ;
#32702 = CARTESIAN_POINT ( 'NONE',  ( -106.8169753891507838, 4.784316299155410235, -11.54838096230724176 ) ) ;
#32704 = DIRECTION ( 'NONE',  ( 0.000000000000000000, 0.000000000000000000, -1.000000000000000000 ) ) ;
#32705 = VERTEX_POINT ( 'NONE', #12674 ) ;
#32706 = DIRECTION ( 'NONE',  ( 0.000000000000000000, 0.000000000000000000, 1.000000000000000000 ) ) ;
#32707 = LINE ( 'NONE', #26668, #16233 ) ;
#32708 = LINE ( 'NONE', #27194, #17208 ) ;
#32709 = EDGE_LOOP ( 'NONE', ( #5308, #22177, #26276, #3636, #26100, #8668, #9660, #14932 ) ) ;
#32710 = VECTOR ( 'NONE', #25013, 1000.000000000000000 ) ;
#32711 = VERTEX_POINT ( 'NONE', #26529 ) ;
#32712 = DIRECTION ( 'NONE',  ( 2.631201909438060585E-14, -5.396010391056496978E-16, 1.000000000000000000 ) ) ;
#32713 = CARTESIAN_POINT ( 'NONE',  ( -442.0000000000000000, 105.0000000000000142, 187.0000000000000000 ) ) ;
#32714 = ORIENTED_EDGE ( 'NONE', *, *, #26617, .F. ) ;
#32715 = AXIS2_PLACEMENT_3D ( 'NONE', #3440, #27658, #25157 ) ;
#32716 = CARTESIAN_POINT ( 'NONE',  ( 0.07098931521633271291, 24.79335165344852854, -19.74422662903591785 ) ) ;
#32717 = CARTESIAN_POINT ( 'NONE',  ( -442.0000000000000000, -104.9999999999999858, -155.0000000000000000 ) ) ;
#32718 = LINE ( 'NONE', #16378, #34956 ) ;
#32719 = CARTESIAN_POINT ( 'NONE',  ( -110.1150203881707910, -0.1727115935459996587, 7.500000000000000888 ) ) ;
#32720 = ORIENTED_EDGE ( 'NONE', *, *, #25061, .T. ) ;
#32721 = ORIENTED_EDGE ( 'NONE', *, *, #3202, .F. ) ;
#32722 = VERTEX_POINT ( 'NONE', #20497 ) ;
#32723 = DIRECTION ( 'NONE',  ( 0.000000000000000000, 0.9980267284282708928, 0.06279051952932451774 ) ) ;
#32724 = VECTOR ( 'NONE', #34018, 1000.000000000000000 ) ;
#32725 = CARTESIAN_POINT ( 'NONE',  ( 1.749999999999999778, -30.28730148581149706, -16.34215476954067015 ) ) ;
#32726 = AXIS2_PLACEMENT_3D ( 'NONE', #17736, #1170, #31415 ) ;
#32727 = CARTESIAN_POINT ( 'NONE',  ( 2.789999999999999147, 27.98916443103598439, 15.38717335695048227 ) ) ;
#32728 = ORIENTED_EDGE ( 'NONE', *, *, #31646, .F. ) ;
#32729 = ORIENTED_EDGE ( 'NONE', *, *, #14235, .T. ) ;
#32730 = CARTESIAN_POINT ( 'NONE',  ( 2.790000000000082192, -17.84469521343956444, -24.93532764985541661 ) ) ;
#32731 = VERTEX_POINT ( 'NONE', #29020 ) ;
#32732 = ADVANCED_FACE ( 'NONE', ( #15516 ), #2151, .T. ) ;
#32733 = CYLINDRICAL_SURFACE ( 'NONE', #20945, 2.524999999999999467 ) ;
#32734 = CARTESIAN_POINT ( 'NONE',  ( 1.155000000000000027, 1.414467053015192657E-16, 4.679999999999999716 ) ) ;
#32735 = ORIENTED_EDGE ( 'NONE', *, *, #27209, .T. ) ;
#32736 = ORIENTED_EDGE ( 'NONE', *, *, #26484, .T. ) ;
#32737 = AXIS2_PLACEMENT_3D ( 'NONE', #16290, #23551, #31926 ) ;
#32738 = FACE_OUTER_BOUND ( 'NONE', #23915, .T. ) ;
#32739 = ADVANCED_FACE ( 'NONE', ( #23512 ), #6954, .F. ) ;
#32740 = CARTESIAN_POINT ( 'NONE',  ( 1.394999999999999574, 28.00026196654270905, 20.00929742917132970 ) ) ;
#32741 = ORIENTED_EDGE ( 'NONE', *, *, #31891, .T. ) ;
#32742 = EDGE_CURVE ( 'NONE', #28976, #26108, #26957, .T. ) ;
#32743 = CARTESIAN_POINT ( 'NONE',  ( 15.99999999999998579, 124.9999999999999716, 162.9999999999999716 ) ) ;
#32744 = DIRECTION ( 'NONE',  ( 0.000000000000000000, -0.6845471059286900584, 0.7289686274214099981 ) ) ;
#32745 = CARTESIAN_POINT ( 'NONE',  ( 2.789999999999999147, -26.96806452364392470, 14.11722088188904145 ) ) ;
#32746 = CARTESIAN_POINT ( 'NONE',  ( -19.99999999999998934, -112.9999999999999858, 174.9999999999999432 ) ) ;
#32747 = PLANE ( 'NONE',  #1779 ) ;
#32748 = DIRECTION ( 'NONE',  ( -1.000000000000000000, 0.000000000000000000, 0.000000000000000000 ) ) ;
#32749 = PLANE ( 'NONE',  #31433 ) ;
#32750 = AXIS2_PLACEMENT_3D ( 'NONE', #32746, #23856, #6 ) ;
#32751 = VERTEX_POINT ( 'NONE', #23175 ) ;
#32752 = CARTESIAN_POINT ( 'NONE',  ( -145.0000000000000568, -12.50000000000001066, 15.00000000000001243 ) ) ;
#32753 = DIRECTION ( 'NONE',  ( 0.1063910735368947813, -0.9943243633099144718, -3.335902418024520312E-15 ) ) ;
#32754 = ORIENTED_EDGE ( 'NONE', *, *, #19794, .T. ) ;
#32755 = ORIENTED_EDGE ( 'NONE', *, *, #4935, .T. ) ;
#32756 = VECTOR ( 'NONE', #11788, 1000.000000000000000 ) ;
#32757 = DIRECTION ( 'NONE',  ( 0.000000000000000000, 0.000000000000000000, -1.000000000000000000 ) ) ;
#32758 = ITEM_DEFINED_TRANSFORMATION ( 'NONE', 'NONE', #26316,  #28566 ) ;
#32759 = VERTEX_POINT ( 'NONE', #15168 ) ;
#32760 = DIRECTION ( 'NONE',  ( -1.000000000000000000, -0.000000000000000000, -0.000000000000000000 ) ) ;
#32761 = AXIS2_PLACEMENT_3D ( 'NONE', #32818, #28018, #8447 ) ;
#32762 = CARTESIAN_POINT ( 'NONE',  ( 37.71145559917817280, 3.353962854566119756, 49.43553178847298568 ) ) ;
#32764 = CARTESIAN_POINT ( 'NONE',  ( -4.875000000000000000, 2.702098422956710877, 0.000000000000000000 ) ) ;
#32763 = PLANE ( 'NONE',  #27138 ) ;
#32765 = VERTEX_POINT ( 'NONE', #32925 ) ;
#32766 = ORIENTED_EDGE ( 'NONE', *, *, #16910, .F. ) ;
#32767 = DIRECTION ( 'NONE',  ( -0.000000000000000000, -1.000000000000000000, -0.000000000000000000 ) ) ;
#32768 = DIRECTION ( 'NONE',  ( 0.000000000000000000, 1.000000000000000000, 0.000000000000000000 ) ) ;
#32769 = CIRCLE ( 'NONE', #19159, 3.999999999999976019 ) ;
#32770 = EDGE_CURVE ( 'NONE', #4571, #14102, #2505, .T. ) ;
#32771 = DIRECTION ( 'NONE',  ( -1.000000000000000000, 0.000000000000000000, 0.000000000000000000 ) ) ;
#32772 = CARTESIAN_POINT ( 'NONE',  ( -32.54223829851967764, 0.4550817492056196678, 15.81122994652406355 ) ) ;
#32773 = CARTESIAN_POINT ( 'NONE',  ( -35.00000000000000000, -46.95407462254104303, 36.69637551990492597 ) ) ;
#32774 = VERTEX_POINT ( 'NONE', #17547 ) ;
#32775 = CARTESIAN_POINT ( 'NONE',  ( 19.99999999999998934, 4.559999999999908127, 172.9900000000000091 ) ) ;
#32776 = CARTESIAN_POINT ( 'NONE',  ( 110.7380848894536598, 7.027143731242819742E-16, -12.50000000000000000 ) ) ;
#32777 = LINE ( 'NONE', #24058, #30976 ) ;
#32778 = PRODUCT ( 'hex structural bolt gradec short_iso_ISO 7412 - M16 x 45 --- 26-WN', 'hex structural bolt gradec short_iso_ISO 7412 - M16 x 45 --- 26-WN', '', ( #7489 ) ) ;
#32779 = EDGE_CURVE ( 'NONE', #2667, #6345, #17712, .T. ) ;
#32780 = CARTESIAN_POINT ( 'NONE',  ( 0.7561992263366478229, -10.98362253094209606, -32.08736770015226369 ) ) ;
#32781 = EDGE_CURVE ( 'NONE', #30105, #192, #8792, .T. ) ;
#32782 = CARTESIAN_POINT ( 'NONE',  ( 22.89764159710611224, 13.56412600238610366, -77.50000000000000000 ) ) ;
#32784 = CARTESIAN_POINT ( 'NONE',  ( -99.88497961182923746, 0.3459610470522913594, -7.500000000000001776 ) ) ;
#32783 = CARTESIAN_POINT ( 'NONE',  ( 2.789999999999999147, 23.28319895603611300, -21.86437915510192909 ) ) ;
#32785 = AXIS2_PLACEMENT_3D ( 'NONE', #18873, #19056, #19398 ) ;
#32786 = EDGE_CURVE ( 'NONE', #23404, #10477, #28381, .T. ) ;
#32787 = EDGE_CURVE ( 'NONE', #16809, #27823, #29394, .T. ) ;
#32788 = DIRECTION ( 'NONE',  ( 0.000000000000000000, 1.000000000000000000, -3.374343856708137958E-53 ) ) ;
#32789 = ORIENTED_EDGE ( 'NONE', *, *, #2326, .T. ) ;
#32790 = CYLINDRICAL_SURFACE ( 'NONE', #23008, 7.999999999999979572 ) ;
#32792 = CARTESIAN_POINT ( 'NONE',  ( 110.5373916640127590, -1.553728400065965687, -7.347407880389961399 ) ) ;
#32791 = LINE ( 'NONE', #8415, #12619 ) ;
#32793 = EDGE_CURVE ( 'NONE', #26941, #23024, #3804, .T. ) ;
#32794 = ORIENTED_EDGE ( 'NONE', *, *, #13187, .F. ) ;
#32795 = DIRECTION ( 'NONE',  ( 1.000000000000000000, 0.000000000000000000, 0.000000000000000000 ) ) ;
#32796 = AXIS2_PLACEMENT_3D ( 'NONE', #24839, #30548, #21646 ) ;
#32797 = ORIENTED_EDGE ( 'NONE', *, *, #22356, .T. ) ;
#32798 = VERTEX_POINT ( 'NONE', #14696 ) ;
#32799 = CARTESIAN_POINT ( 'NONE',  ( 1.040000000000000924, 0.000000000000000000, 0.000000000000000000 ) ) ;
#32800 = ORIENTED_EDGE ( 'NONE', *, *, #24121, .T. ) ;
#32801 = ORIENTED_EDGE ( 'NONE', *, *, #7106, .F. ) ;
#32802 = DIRECTION ( 'NONE',  ( 1.000000000000000000, 0.000000000000000000, 0.000000000000000000 ) ) ;
#32803 = AXIS2_PLACEMENT_3D ( 'NONE', #31809, #2095, #7593 ) ;
#32804 = AXIS2_PLACEMENT_3D ( 'NONE', #20879, #34760, #21050 ) ;
#32805 = DIRECTION ( 'NONE',  ( 1.000000000000000000, 0.000000000000000000, 0.000000000000000000 ) ) ;
#32806 = LINE ( 'NONE', #32450, #2319 ) ;
#32807 = EDGE_LOOP ( 'NONE', ( #30266, #2104, #33951, #5139, #14874, #33148, #24873, #28451, #24167, #16241, #5473 ) ) ;
#32808 = EDGE_LOOP ( 'NONE', ( #24519, #25249, #31192, #2966, #18015, #19062, #2649 ) ) ;
#32809 = DIRECTION ( 'NONE',  ( -1.000000000000000000, -0.000000000000000000, -0.000000000000000000 ) ) ;
#32810 = CARTESIAN_POINT ( 'NONE',  ( -418.0000000000000000, -125.0000000000000000, -105.9999999999999574 ) ) ;
#32811 = CARTESIAN_POINT ( 'NONE',  ( 110.1383142917281646, -2.560920621327495983, -12.23601723495363380 ) ) ;
#32812 = CARTESIAN_POINT ( 'NONE',  ( 0.000000000000000000, 0.000000000000000000, 87.50000000000000000 ) ) ;
#32813 = VERTEX_POINT ( 'NONE', #20373 ) ;
#32814 = CIRCLE ( 'NONE', #18641, 30.47050528711511674 ) ;
#32815 = CARTESIAN_POINT ( 'NONE',  ( -1.649999999999999911, 0.000000000000000000, 3.180000000000000160 ) ) ;
#32816 = DIRECTION ( 'NONE',  ( 0.000000000000000000, -0.000000000000000000, -1.000000000000000000 ) ) ;
#32817 = ORIENTED_EDGE ( 'NONE', *, *, #12070, .F. ) ;
#32818 = CARTESIAN_POINT ( 'NONE',  ( 21.85761591200894216, 30.91355005303805825, 68.31122994652405112 ) ) ;
#32819 = DIRECTION ( 'NONE',  ( -0.000000000000000000, 0.000000000000000000, 1.000000000000000000 ) ) ;
#32820 = CARTESIAN_POINT ( 'NONE',  ( 2.033800773547048024, -32.71371797491563882, -8.947166372575045656 ) ) ;
#32821 = DIRECTION ( 'NONE',  ( 1.000000000000000000, 0.000000000000000000, -1.848892746611746966E-32 ) ) ;
#32822 = EDGE_LOOP ( 'NONE', ( #9706, #22662, #21308, #21660 ) ) ;
#32823 = AXIS2_PLACEMENT_3D ( 'NONE', #24999, #2594, #27504 ) ;
#32824 = EDGE_CURVE ( 'NONE', #6833, #31113, #15038, .T. ) ;
#32825 = ADVANCED_FACE ( 'NONE', ( #17892 ), #31051, .F. ) ;
#32826 = LINE ( 'NONE', #24818, #32030 ) ;
#32827 = EDGE_LOOP ( 'NONE', ( #28101, #18872, #19679 ) ) ;
#32828 = PRESENTATION_STYLE_ASSIGNMENT (( #19158 ) ) ;
#32829 = DIRECTION ( 'NONE',  ( -0.000000000000000000, -0.000000000000000000, -1.000000000000000000 ) ) ;
#32830 = VECTOR ( 'NONE', #27030, 1000.000000000000000 ) ;
#32831 = CIRCLE ( 'NONE', #4982, 30.47050528711512030 ) ;
#32832 = ORIENTED_EDGE ( 'NONE', *, *, #35084, .T. ) ;
#32833 = CARTESIAN_POINT ( 'NONE',  ( 36.10877985260814427, 11.38239727801116352, 49.43553178847298568 ) ) ;
#32834 = DIRECTION ( 'NONE',  ( 0.9289767198167914186, 0.3701381553399144542, -0.000000000000000000 ) ) ;
#32835 = EDGE_LOOP ( 'NONE', ( #33268, #32206, #29897, #19949 ) ) ;
#32836 = ADVANCED_FACE ( 'NONE', ( #1497 ), #7165, .T. ) ;
#32837 = AXIS2_PLACEMENT_3D ( 'NONE', #21968, #24616, #27826 ) ;
#32838 = ORIENTED_EDGE ( 'NONE', *, *, #20336, .F. ) ;
#32839 = DIRECTION ( 'NONE',  ( -1.000000000000000000, -0.000000000000000000, -0.000000000000000000 ) ) ;
#32840 = CARTESIAN_POINT ( 'NONE',  ( -110.1150203881707625, 0.3459610470522903047, 7.499999999999997335 ) ) ;
#32841 = ORIENTED_EDGE ( 'NONE', *, *, #3593, .T. ) ;
#32842 = ORIENTED_EDGE ( 'NONE', *, *, #15287, .F. ) ;
#32843 = CARTESIAN_POINT ( 'NONE',  ( 19.99999999999998224, 144.9999999999999147, 187.0000000000000000 ) ) ;
#32844 = EDGE_CURVE ( 'NONE', #18562, #19944, #11657, .T. ) ;
#32845 = EDGE_CURVE ( 'NONE', #10974, #10245, #23376, .T. ) ;
#32846 = CARTESIAN_POINT ( 'NONE',  ( 0.000000000000000000, 2.281310696040539424E-14, -36.68877005347592757 ) ) ;
#32847 = EDGE_CURVE ( 'NONE', #25253, #31542, #33711, .T. ) ;
#32848 = CIRCLE ( 'NONE', #22070, 7.999999999999979572 ) ;
#32849 = CARTESIAN_POINT ( 'NONE',  ( 2.719010697917859876, -22.12324074713392719, -22.69596835361152998 ) ) ;
#32850 = DIRECTION ( 'NONE',  ( 0.000000000000000000, 0.7071067811865489050, 0.7071067811865462405 ) ) ;
#32851 = ORIENTED_EDGE ( 'NONE', *, *, #14033, .F. ) ;
#32852 = ORIENTED_EDGE ( 'NONE', *, *, #16945, .T. ) ;
#32853 = CARTESIAN_POINT ( 'NONE',  ( -365.0000000000000000, -114.9999999999999858, 113.9999999999999858 ) ) ;
#32854 = CARTESIAN_POINT ( 'NONE',  ( -355.0000000000000000, -119.0000000000000000, 111.9999999999999858 ) ) ;
#32855 = DIRECTION ( 'NONE',  ( 0.8276889981568912313, 0.5611870653623813876, 1.030883914978405312E-16 ) ) ;
#32856 = EDGE_CURVE ( 'NONE', #7282, #16746, #28722, .T. ) ;
#32857 = CYLINDRICAL_SURFACE ( 'NONE', #600, 9.999999999999998224 ) ;
#32858 = VECTOR ( 'NONE', #17816, 1000.000000000000114 ) ;
#32859 = DIRECTION ( 'NONE',  ( 0.000000000000000000, 0.000000000000000000, 1.000000000000000000 ) ) ;
#32861 = DIRECTION ( 'NONE',  ( 1.000000000000000000, 0.000000000000000000, 0.000000000000000000 ) ) ;
#32860 =( REPRESENTATION_RELATIONSHIP ('NONE','NONE', #23037, #28231 ) REPRESENTATION_RELATIONSHIP_WITH_TRANSFORMATION ( #8555 )SHAPE_REPRESENTATION_RELATIONSHIP( ) );
#32863 = VECTOR ( 'NONE', #34167, 1000.000000000000000 ) ;
#32862 = CARTESIAN_POINT ( 'NONE',  ( -418.0000000000000000, 104.9999999999999858, -194.9999999999999716 ) ) ;
#32864 = EDGE_LOOP ( 'NONE', ( #4783, #18565, #1090, #7825 ) ) ;
#32865 = DIRECTION ( 'NONE',  ( 1.000000000000000000, 0.000000000000000000, 1.300283923313630633E-47 ) ) ;
#32866 = CARTESIAN_POINT ( 'NONE',  ( 2.783128676084626552, 4.186936631163378664, -30.58426604563490159 ) ) ;
#32867 = AXIS2_PLACEMENT_3D ( 'NONE', #12701, #31374, #34399 ) ;
#32868 = DIRECTION ( 'NONE',  ( 2.530127506375325574E-80, -1.000000000000000000, -6.842277657836020854E-49 ) ) ;
#32869 = VERTEX_POINT ( 'NONE', #4321 ) ;
#32870 = EDGE_CURVE ( 'NONE', #28035, #22441, #34349, .T. ) ;
#32871 = LINE ( 'NONE', #13659, #15532 ) ;
#32872 = ORIENTED_EDGE ( 'NONE', *, *, #26520, .T. ) ;
#32873 = CARTESIAN_POINT ( 'NONE',  ( -8.499999999999998224, 0.000000000000000000, 4.679999999999999716 ) ) ;
#32874 = CARTESIAN_POINT ( 'NONE',  ( -104.6588445208797822, 5.114806216612618250, 11.40564585725303992 ) ) ;
#32875 = CIRCLE ( 'NONE', #17567, 4.306175033202026547 ) ;
#32876 = AXIS2_PLACEMENT_3D ( 'NONE', #20480, #31326, #17825 ) ;
#32877 = ORIENTED_EDGE ( 'NONE', *, *, #20176, .T. ) ;
#32878 = CARTESIAN_POINT ( 'NONE',  ( 5.021133111224369117, -1.691831803474591833, -67.50000000000000000 ) ) ;
#32879 = LINE ( 'NONE', #30575, #12826 ) ;
#32880 = CARTESIAN_POINT ( 'NONE',  ( 32.40067729534749219, 3.066020821660472517, 68.31122994652405112 ) ) ;
#32881 = ORIENTED_EDGE ( 'NONE', *, *, #29304, .F. ) ;
#32882 = CIRCLE ( 'NONE', #14159, 12.00000000000001066 ) ;
#32883 = EDGE_LOOP ( 'NONE', ( #7573, #8005, #6317, #26700 ) ) ;
#32884 = CARTESIAN_POINT ( 'NONE',  ( 820.4007175367466971, 1317.146825192654205, 1753.598338701302737 ) ) ;
#32885 = DIRECTION ( 'NONE',  ( 0.000000000000000000, 0.000000000000000000, 1.000000000000000000 ) ) ;
#32886 = ORIENTED_EDGE ( 'NONE', *, *, #10871, .F. ) ;
#32887 = EDGE_CURVE ( 'NONE', #17261, #35062, #13356, .T. ) ;
#32888 = CARTESIAN_POINT ( 'NONE',  ( 19.99999999999998934, -115.0000000000000000, 162.9999999999999716 ) ) ;
#32889 = AXIS2_PLACEMENT_3D ( 'NONE', #27875, #19534, #27527 ) ;
#32890 = EDGE_CURVE ( 'NONE', #24367, #14830, #19607, .T. ) ;
#32891 = EDGE_CURVE ( 'NONE', #10877, #28025, #31562, .T. ) ;
#32892 = LINE ( 'NONE', #14222, #854 ) ;
#32893 = CARTESIAN_POINT ( 'NONE',  ( 110.7380848894536598, -4.118294838564020743E-16, 7.500000000000000000 ) ) ;
#32894 = ITEM_DEFINED_TRANSFORMATION ( 'NONE', 'NONE', #25170,  #28566 ) ;
#32895 = EDGE_LOOP ( 'NONE', ( #23904, #7219, #33682, #20800 ) ) ;
#32896 = ORIENTED_EDGE ( 'NONE', *, *, #4562, .T. ) ;
#32897 = EDGE_LOOP ( 'NONE', ( #27037, #16713, #24137, #20776 ) ) ;
#32898 = LINE ( 'NONE', #16200, #12440 ) ;
#32899 = CARTESIAN_POINT ( 'NONE',  ( 29.63313772848249883, -13.45665341906702572, 68.31122994652405112 ) ) ;
#32900 = CARTESIAN_POINT ( 'NONE',  ( 2.604019720910715652, -22.69026646801078329, 22.96218055026789528 ) ) ;
#32901 = AXIS2_PLACEMENT_3D ( 'NONE', #7726, #32115, #28925 ) ;
#32902 = VERTEX_POINT ( 'NONE', #14865 ) ;
#32903 = VERTEX_POINT ( 'NONE', #22867 ) ;
#32904 = DIRECTION ( 'NONE',  ( 0.000000000000000000, 1.000000000000000000, 0.000000000000000000 ) ) ;
#32905 = ORIENTED_EDGE ( 'NONE', *, *, #32010, .F. ) ;
#32906 = DIRECTION ( 'NONE',  ( 0.000000000000000000, 0.000000000000000000, 1.000000000000000000 ) ) ;
#32907 = LINE ( 'NONE', #356, #16002 ) ;
#32908 = ORIENTED_EDGE ( 'NONE', *, *, #15863, .F. ) ;
#32909 = CIRCLE ( 'NONE', #7913, 3.999999999999976019 ) ;
#32910 = VERTEX_POINT ( 'NONE', #9333 ) ;
#32911 = CARTESIAN_POINT ( 'NONE',  ( -499.9999999999999432, 140.9999999999999716, -162.9999999999999716 ) ) ;
#32912 = LINE ( 'NONE', #32740, #6951 ) ;
#32913 = ORIENTED_EDGE ( 'NONE', *, *, #31070, .F. ) ;
#32914 = CARTESIAN_POINT ( 'NONE',  ( 0.000000000000000000, 0.000000000000000000, 0.000000000000000000 ) ) ;
#32915 = CARTESIAN_POINT ( 'NONE',  ( 3.235562306570555532E-30, -11.61907005722761532, -67.50000000000000000 ) ) ;
#32916 = CARTESIAN_POINT ( 'NONE',  ( -32.32899628990713126, -3.747048406849353697, 68.31122994652405112 ) ) ;
#32917 = AXIS2_PLACEMENT_3D ( 'NONE', #22509, #30860, #8794 ) ;
#32918 = CARTESIAN_POINT ( 'NONE',  ( 0.000000000000000000, 1.592040838891559095E-15, -13.00000000000000000 ) ) ;
#32919 = CARTESIAN_POINT ( 'NONE',  ( 2.719051660475461762, -3.385765165811317701, -31.51266256086719153 ) ) ;
#32920 = DIRECTION ( 'NONE',  ( 0.000000000000000000, 0.000000000000000000, 1.000000000000000000 ) ) ;
#32921 = EDGE_CURVE ( 'NONE', #3404, #22677, #25699, .T. ) ;
#32922 = FACE_BOUND ( 'NONE', #31090, .T. ) ;
#32923 = AXIS2_PLACEMENT_3D ( 'NONE', #31718, #7325, #18054 ) ;
#32924 = ORIENTED_EDGE ( 'NONE', *, *, #13301, .T. ) ;
#32925 = CARTESIAN_POINT ( 'NONE',  ( -20.82057426567703473, -31.63141042832694083, 68.31122994652405112 ) ) ;
#32926 = CARTESIAN_POINT ( 'NONE',  ( 838.8197622696438884, 1145.003577474997201, 1753.598338701303192 ) ) ;
#32927 = ORIENTED_EDGE ( 'NONE', *, *, #14484, .T. ) ;
#32928 = ORIENTED_EDGE ( 'NONE', *, *, #29412, .F. ) ;
#32929 = EDGE_CURVE ( 'NONE', #22259, #32269, #5375, .T. ) ;
#32930 = EDGE_CURVE ( 'NONE', #17595, #5551, #10909, .T. ) ;
#32931 = ADVANCED_FACE ( 'NONE', ( #32261 ), #16086, .F. ) ;
#32932 = CARTESIAN_POINT ( 'NONE',  ( 99.80463941335877109, 2.443267496989373733, 7.093208238637026319 ) ) ;
#32933 = SHAPE_DEFINITION_REPRESENTATION ( #33071, #34141 ) ;
#32934 = ORIENTED_EDGE ( 'NONE', *, *, #14083, .T. ) ;
#32935 = EDGE_CURVE ( 'NONE', #30302, #31113, #13237, .T. ) ;
#32936 = CARTESIAN_POINT ( 'NONE',  ( -31.68358972719163091, 7.440061483287530919, 68.31122994652405112 ) ) ;
#32938 = DIRECTION ( 'NONE',  ( 0.000000000000000000, 0.000000000000000000, 1.000000000000000000 ) ) ;
#32937 = LINE ( 'NONE', #19788, #23548 ) ;
#32939 = ORIENTED_EDGE ( 'NONE', *, *, #13717, .F. ) ;
#32940 = VERTEX_POINT ( 'NONE', #2016 ) ;
#32941 = DIRECTION ( 'NONE',  ( 0.000000000000000000, 0.000000000000000000, 1.000000000000000000 ) ) ;
#32942 = CARTESIAN_POINT ( 'NONE',  ( -20.00000000000004619, 124.9999999999999716, 162.9999999999999716 ) ) ;
#32943 = DIRECTION ( 'NONE',  ( -0.000000000000000000, 1.836970198721029688E-16, -1.000000000000000000 ) ) ;
#32944 = CYLINDRICAL_SURFACE ( 'NONE', #29770, 8.000000000000000000 ) ;
#32945 = EDGE_LOOP ( 'NONE', ( #7048, #10085, #2374, #26455 ) ) ;
#32946 = DIRECTION ( 'NONE',  ( -3.040835319149746090E-31, -1.000000000000000000, 3.748118910144520367E-63 ) ) ;
#32947 = DIRECTION ( 'NONE',  ( 0.000000000000000000, 1.310824597558155437E-49, 1.000000000000000000 ) ) ;
#32948 = LINE ( 'NONE', #2528, #22617 ) ;
#32949 = VERTEX_POINT ( 'NONE', #27096 ) ;
#32950 = CARTESIAN_POINT ( 'NONE',  ( 2.265105771424310355, 33.20489141755878393, -3.412611943275337900 ) ) ;
#32951 = CARTESIAN_POINT ( 'NONE',  ( -410.0000000000000568, 124.9999999999999574, -187.0000000000000000 ) ) ;
#32952 = DIRECTION ( 'NONE',  ( -0.000000000000000000, -0.000000000000000000, -1.000000000000000000 ) ) ;
#32954 = CARTESIAN_POINT ( 'NONE',  ( 145.0000000000000568, -88.29863524074325198, -74.12844257252345415 ) ) ;
#32953 = CARTESIAN_POINT ( 'NONE',  ( -365.0000000000000000, -135.0000000000000000, 126.0000000000000000 ) ) ;
#32955 = DIRECTION ( 'NONE',  ( 0.000000000000000000, 0.000000000000000000, -1.000000000000000000 ) ) ;
#32956 = VERTEX_POINT ( 'NONE', #2536 ) ;
#32957 = CARTESIAN_POINT ( 'NONE',  ( 0.02407890056655695096, 30.61125888652969707, -5.439165181698684570 ) ) ;
#32958 = FACE_BOUND ( 'NONE', #21559, .T. ) ;
#32959 = AXIS2_PLACEMENT_3D ( 'NONE', #34346, #2163, #24220 ) ;
#32960 = VERTEX_POINT ( 'NONE', #13584 ) ;
#32961 = EDGE_CURVE ( 'NONE', #15892, #28736, #10203, .T. ) ;
#32962 = ORIENTED_EDGE ( 'NONE', *, *, #15153, .T. ) ;
#32963 = EDGE_CURVE ( 'NONE', #10974, #20895, #29252, .T. ) ;
#32964 = VERTEX_POINT ( 'NONE', #13411 ) ;
#32965 = CARTESIAN_POINT ( 'NONE',  ( -418.0000000000000000, -124.9999999999999858, -77.99999999999997158 ) ) ;
#32966 = VERTEX_POINT ( 'NONE', #32079 ) ;
#32967 = VERTEX_POINT ( 'NONE', #2188 ) ;
#32968 = EDGE_CURVE ( 'NONE', #34030, #2667, #21327, .T. ) ;
#32969 = CARTESIAN_POINT ( 'NONE',  ( 2.790000000000081748, 20.82920972943033888, 22.50217193233309487 ) ) ;
#32970 = ITEM_DEFINED_TRANSFORMATION ( 'NONE', 'NONE', #34297,  #28566 ) ;
#32971 = ORIENTED_EDGE ( 'NONE', *, *, #6212, .T. ) ;
#32972 = CARTESIAN_POINT ( 'NONE',  ( 11.99999999999999645, 112.9999999999999574, -175.0000000000000284 ) ) ;
#32973 = CARTESIAN_POINT ( 'NONE',  ( -5.021133111224886036, 6.201984591278720593, -87.50000000000000000 ) ) ;
#32974 = ORIENTED_EDGE ( 'NONE', *, *, #7854, .F. ) ;
#32975 = EDGE_CURVE ( 'NONE', #4511, #20828, #21055, .T. ) ;
#32976 = ORIENTED_EDGE ( 'NONE', *, *, #5875, .F. ) ;
#32977 = DIRECTION ( 'NONE',  ( 1.000000000000000000, 0.000000000000000000, 0.000000000000000000 ) ) ;
#32978 = LINE ( 'NONE', #11293, #9564 ) ;
#32979 = EDGE_CURVE ( 'NONE', #21650, #13146, #17947, .T. ) ;
#32980 = CARTESIAN_POINT ( 'NONE',  ( 105.7618603918998303, -5.690476701307018104, -11.12964202013672654 ) ) ;
#32981 = DIRECTION ( 'NONE',  ( 0.000000000000000000, 0.000000000000000000, -1.000000000000000000 ) ) ;
#32982 = ORIENTED_EDGE ( 'NONE', *, *, #9437, .F. ) ;
#32983 = AXIS2_PLACEMENT_3D ( 'NONE', #17963, #15279, #1729 ) ;
#32984 = EDGE_CURVE ( 'NONE', #1890, #12135, #10741, .T. ) ;
#32985 = DIRECTION ( 'NONE',  ( 0.9818488882034280829, 0.1609659548241204607, 0.1003131203843820457 ) ) ;
#32986 = DIRECTION ( 'NONE',  ( -0.000000000000000000, -0.000000000000000000, -1.000000000000000000 ) ) ;
#32987 = ORIENTED_EDGE ( 'NONE', *, *, #24153, .T. ) ;
#32988 = CARTESIAN_POINT ( 'NONE',  ( -6.500000000000000000, 0.000000000000000000, 0.000000000000000000 ) ) ;
#32989 = CARTESIAN_POINT ( 'NONE',  ( -414.0000000000000568, 104.9999999999999858, -187.0000000000000000 ) ) ;
#32990 = DIRECTION ( 'NONE',  ( -0.000000000000000000, -1.836970198721029688E-16, 1.000000000000000000 ) ) ;
#32991 = DIRECTION ( 'NONE',  ( 1.000000000000000000, 0.000000000000000000, 0.000000000000000000 ) ) ;
#32992 = EDGE_LOOP ( 'NONE', ( #8548, #22436, #32976, #15229 ) ) ;
#32993 = VECTOR ( 'NONE', #12353, 1000.000000000000000 ) ;
#32994 = PRESENTATION_LAYER_ASSIGNMENT (  '', '', ( #31848 ) ) ;
#32995 = DIRECTION ( 'NONE',  ( 2.891205793294675861E-16, 0.000000000000000000, 1.000000000000000000 ) ) ;
#32996 = ORIENTED_EDGE ( 'NONE', *, *, #7340, .F. ) ;
#32998 = LINE ( 'NONE', #94, #23682 ) ;
#32997 = CARTESIAN_POINT ( 'NONE',  ( 1.749999999999999778, 28.00026196654299326, -20.00929742917092469 ) ) ;
#32999 = ORIENTED_EDGE ( 'NONE', *, *, #21975, .T. ) ;
#33000 = FACE_OUTER_BOUND ( 'NONE', #5862, .T. ) ;
#33001 = CARTESIAN_POINT ( 'NONE',  ( 0.000000000000000000, 23.28319895603611300, -19.33937915510192695 ) ) ;
#33002 = AXIS2_PLACEMENT_3D ( 'NONE', #33216, #9188, #6148 ) ;
#33003 = ORIENTED_EDGE ( 'NONE', *, *, #28406, .F. ) ;
#33004 = AXIS2_PLACEMENT_3D ( 'NONE', #25904, #1858, #9698 ) ;
#33005 = EDGE_LOOP ( 'NONE', ( #28874, #12527, #2298, #20140 ) ) ;
#33006 = ORIENTED_EDGE ( 'NONE', *, *, #12423, .F. ) ;
#33007 = FACE_OUTER_BOUND ( 'NONE', #21172, .T. ) ;
#33008 = DIRECTION ( 'NONE',  ( -0.000000000000000000, 0.000000000000000000, -1.000000000000000000 ) ) ;
#33009 = ORIENTED_EDGE ( 'NONE', *, *, #10037, .T. ) ;
#33010 = VERTEX_POINT ( 'NONE', #7880 ) ;
#33011 = CARTESIAN_POINT ( 'NONE',  ( -499.9999999999999432, -137.0000000000000000, -187.0000000000000000 ) ) ;
#33012 = ADVANCED_FACE ( 'NONE', ( #29768 ), #3096, .T. ) ;
#33013 = CARTESIAN_POINT ( 'NONE',  ( 19.99999999999990763, -134.9999999999999716, -186.9999999999999716 ) ) ;
#33014 = CARTESIAN_POINT ( 'NONE',  ( 0.000000000000000000, -17.83604598421647935, -24.70480026434186982 ) ) ;
#33015 = CIRCLE ( 'NONE', #5746, 7.500000000000000000 ) ;
#33016 = DIRECTION ( 'NONE',  ( 0.000000000000000000, 1.836970198721029441E-16, -1.000000000000000000 ) ) ;
#33017 = EDGE_CURVE ( 'NONE', #29292, #28354, #8225, .T. ) ;
#33018 = VERTEX_POINT ( 'NONE', #34590 ) ;
#33019 = EDGE_CURVE ( 'NONE', #33515, #32629, #24125, .T. ) ;
#33020 = ORIENTED_EDGE ( 'NONE', *, *, #30836, .T. ) ;
#33021 = CIRCLE ( 'NONE', #2330, 34.41491905851385269 ) ;
#33022 = CARTESIAN_POINT ( 'NONE',  ( 0.02407890056655651728, 29.44518845714764765, 9.980709654879525772 ) ) ;
#33023 = LINE ( 'NONE', #27693, #11826 ) ;
#33024 = AXIS2_PLACEMENT_3D ( 'NONE', #11672, #25526, #5763 ) ;
#33025 = CIRCLE ( 'NONE', #13729, 3.999999999999976019 ) ;
#33026 = CARTESIAN_POINT ( 'NONE',  ( -35.00000000000000000, 16.36947364650383818, 36.69637551990492597 ) ) ;
#33027 = DIRECTION ( 'NONE',  ( -1.000000000000000000, 0.000000000000000000, 0.000000000000000000 ) ) ;
#33028 = CARTESIAN_POINT ( 'NONE',  ( 0.07094833961210175732, 14.74858964725109267, -28.05334937082576374 ) ) ;
#33029 = B_SPLINE_CURVE_WITH_KNOTS ( 'NONE', 3,
 ( #29839, #18817, #29492, #8115, #18994, #5439 ),
 .UNSPECIFIED., .F., .F.,
 ( 4, 2, 4 ),
 ( 2.380729204614878139E-07, 0.003943479449179622918, 0.007886720825438783139 ),
 .UNSPECIFIED. ) ;
#33030 = DIRECTION ( 'NONE',  ( 0.000000000000000000, 5.145227585319922065E-49, 1.000000000000000000 ) ) ;
#33031 = CARTESIAN_POINT ( 'NONE',  ( -410.0000000000000568, -105.0000000000000142, 187.0000000000000000 ) ) ;
#33032 = ORIENTED_EDGE ( 'NONE', *, *, #22851, .T. ) ;
#33033 = AXIS2_PLACEMENT_3D ( 'NONE', #25685, #606, #25509 ) ;
#33034 = PLANE ( 'NONE',  #34476 ) ;
#33035 = CARTESIAN_POINT ( 'NONE',  ( -12.00000000000001066, 134.9999999999999432, -162.9999999999999432 ) ) ;
#33036 = ADVANCED_FACE ( 'NONE', ( #2355 ), #24065, .F. ) ;
#33037 = VECTOR ( 'NONE', #33258, 1000.000000000000000 ) ;
#33038 = LINE ( 'NONE', #30035, #9234 ) ;
#33039 = ORIENTED_EDGE ( 'NONE', *, *, #9384, .F. ) ;
#33040 = CARTESIAN_POINT ( 'NONE',  ( 105.0000000000000000, 0.000000000000000000, -57.49999999999999289 ) ) ;
#33041 = VERTEX_POINT ( 'NONE', #24244 ) ;
#33042 = CARTESIAN_POINT ( 'NONE',  ( -35.00000000000000000, 28.28427124746189136, -36.69637551990492597 ) ) ;
#33043 = DIRECTION ( 'NONE',  ( 0.000000000000000000, 0.000000000000000000, -1.000000000000000000 ) ) ;
#33044 = EDGE_CURVE ( 'NONE', #23276, #16809, #7078, .T. ) ;
#33045 = EDGE_CURVE ( 'NONE', #17362, #12453, #30957, .T. ) ;
#33046 = EDGE_CURVE ( 'NONE', #20784, #18455, #32081, .T. ) ;
#33048 = ORIENTED_EDGE ( 'NONE', *, *, #18123, .F. ) ;
#33047 = AXIS2_PLACEMENT_3D ( 'NONE', #27221, #30426, #6023 ) ;
#33049 = CIRCLE ( 'NONE', #4055, 7.999999999999979572 ) ;
#33050 = CARTESIAN_POINT ( 'NONE',  ( 0.006892399591254335864, -7.987299431473847910, 29.81857704081742355 ) ) ;
#33051 = AXIS2_PLACEMENT_3D ( 'NONE', #31233, #28563, #4333 ) ;
#33052 = CARTESIAN_POINT ( 'NONE',  ( 15.99999999999998579, 136.9999999999999716, -175.0000000000000284 ) ) ;
#33053 = CARTESIAN_POINT ( 'NONE',  ( -10.00000000000000000, 0.000000000000000000, 0.000000000000000000 ) ) ;
#33054 = EDGE_CURVE ( 'NONE', #29286, #32553, #14469, .T. ) ;
#33055 = VERTEX_POINT ( 'NONE', #24588 ) ;
#33056 = DIRECTION ( 'NONE',  ( 0.1063910735369155841, -0.9943243633099125844, -3.335902418025060287E-15 ) ) ;
#33057 = CARTESIAN_POINT ( 'NONE',  ( 2.790000000000079972, -30.07763130521186312, -5.961539033704989166 ) ) ;
#33058 = ORIENTED_EDGE ( 'NONE', *, *, #31153, .T. ) ;
#33059 = CARTESIAN_POINT ( 'NONE',  ( -442.0000000000000000, 105.0000000000000142, 100.0000000000000000 ) ) ;
#33060 = VECTOR ( 'NONE', #7240, 1000.000000000000000 ) ;
#33061 = CARTESIAN_POINT ( 'NONE',  ( 2.765921099433441999, -31.05158812718222450, 1.559667679918499417 ) ) ;
#33062 = CARTESIAN_POINT ( 'NONE',  ( -15.99999999999998579, 75.55999999999990280, -168.2400000000000091 ) ) ;
#33063 = CARTESIAN_POINT ( 'NONE',  ( -99.88497961182919482, -2.585407550593147656E-15, 7.500000000000000000 ) ) ;
#33064 = ITEM_DEFINED_TRANSFORMATION ( 'NONE', 'NONE', #5294,  #28566 ) ;
#33065 = EDGE_CURVE ( 'NONE', #31447, #34682, #21296, .T. ) ;
#33066 = ORIENTED_EDGE ( 'NONE', *, *, #5241, .T. ) ;
#33067 = EDGE_CURVE ( 'NONE', #8689, #16065, #4782, .T. ) ;
#33069 = VERTEX_POINT ( 'NONE', #8410 ) ;
#33068 =( REPRESENTATION_RELATIONSHIP ('NONE','NONE', #23037, #15767 ) REPRESENTATION_RELATIONSHIP_WITH_TRANSFORMATION ( #11731 )SHAPE_REPRESENTATION_RELATIONSHIP( ) );
#33070 = VERTEX_POINT ( 'NONE', #32953 ) ;
#33071 = PRODUCT_DEFINITION_SHAPE ( 'NONE', 'NONE',  #22952 ) ;
#33072 =( LENGTH_UNIT ( ) NAMED_UNIT ( * ) SI_UNIT ( .MILLI., .METRE. ) );
#33073 = ADVANCED_FACE ( 'NONE', ( #27977 ), #16618, .F. ) ;
#33074 = CARTESIAN_POINT ( 'NONE',  ( 2.719051683612535797, -28.42120447776860104, -14.02663268823320486 ) ) ;
#33075 = CIRCLE ( 'NONE', #22854, 13.50000000000000178 ) ;
#33076 = CARTESIAN_POINT ( 'NONE',  ( -20.00000000000007461, 104.9999999999999858, -187.0000000000000000 ) ) ;
#33078 = ORIENTED_EDGE ( 'NONE', *, *, #29931, .T. ) ;
#33077 = AXIS2_PLACEMENT_3D ( 'NONE', #9672, #20535, #32032 ) ;
#33079 = ORIENTED_EDGE ( 'NONE', *, *, #26237, .F. ) ;
#33080 = CARTESIAN_POINT ( 'NONE',  ( 2.630124765083918348, -1.866624223957557893, 5.429999999999999716 ) ) ;
#33081 = CIRCLE ( 'NONE', #25122, 32.54542015209054284 ) ;
#33082 = EDGE_LOOP ( 'NONE', ( #3431, #16640, #26491, #24912 ) ) ;
#33083 = AXIS2_PLACEMENT_3D ( 'NONE', #25074, #3889, #25608 ) ;
#33084 = DIRECTION ( 'NONE',  ( 0.000000000000000000, 1.836970198721029441E-16, -1.000000000000000000 ) ) ;
#33085 = CARTESIAN_POINT ( 'NONE',  ( -499.9999999999999432, 136.9999999999999432, -155.0000000000000000 ) ) ;
#33086 = VERTEX_POINT ( 'NONE', #13935 ) ;
#33087 = ORIENTED_EDGE ( 'NONE', *, *, #10348, .F. ) ;
#33088 = DIRECTION ( 'NONE',  ( 0.000000000000000000, 0.000000000000000000, -1.000000000000000000 ) ) ;
#33089 = DIRECTION ( 'NONE',  ( 0.9075754196709575616, -0.4198891015602635446, 0.000000000000000000 ) ) ;
#33090 = ORIENTED_EDGE ( 'NONE', *, *, #11807, .T. ) ;
#33091 = DIRECTION ( 'NONE',  ( -0.000000000000000000, -1.000000000000000000, -0.000000000000000000 ) ) ;
#33092 = PRESENTATION_STYLE_ASSIGNMENT (( #14782 ) ) ;
#33093 = FACE_OUTER_BOUND ( 'NONE', #4992, .T. ) ;
#33094 = ADVANCED_FACE ( 'NONE', ( #19112 ), #19282, .F. ) ;
#33095 = EDGE_CURVE ( 'NONE', #14920, #10924, #21937, .T. ) ;
#33096 = CARTESIAN_POINT ( 'NONE',  ( -108.3782164809644115, -3.855135278743967664, 11.89320834461816112 ) ) ;
#33097 = CLOSED_SHELL ( 'NONE', ( #15847, #23699, #4429, #13488 ) ) ;
#33098 = CARTESIAN_POINT ( 'NONE',  ( 145.0000000000000568, -78.33668825982573480, -65.00000000000000000 ) ) ;
#33099 = FACE_OUTER_BOUND ( 'NONE', #7741, .T. ) ;
#33100 = ADVANCED_FACE ( 'NONE', ( #408 ), #3582, .F. ) ;
#33101 = AXIS2_PLACEMENT_3D ( 'NONE', #2026, #18242, #1846 ) ;
#33102 = ORIENTED_EDGE ( 'NONE', *, *, #23664, .T. ) ;
#33103 = VECTOR ( 'NONE', #30080, 1000.000000000000000 ) ;
#33104 = CIRCLE ( 'NONE', #31405, 4.306175033202026547 ) ;
#33105 = CARTESIAN_POINT ( 'NONE',  ( 831.9043462559408226, 1209.634625891497308, 1753.598338701303419 ) ) ;
#33106 = VECTOR ( 'NONE', #3146, 1000.000000000000000 ) ;
#33107 = ADVANCED_FACE ( 'NONE', ( #14294 ), #27271, .T. ) ;
#33108 = B_SPLINE_CURVE_WITH_KNOTS ( 'NONE', 3,
 ( #31278, #20600, #7055, #4546, #15623, #34294, #12596, #4209, #17769, #7398, #34473, #4381, #15095, #20432, #25939, #15271, #1894, #28609, #12951, #26109, #1723, #23439, #9913, #20774, #1556, #23793, #31621, #18476, #33950, #15442, #26281, #21118, #18295, #12430, #12777, #23619, #10089, #29315, #4905, #15802, #23277, #23105, #26633 ),
 .UNSPECIFIED., .F., .F.,
 ( 4, 2, 2, 2, 2, 2, 2, 2, 2, 2, 2, 1, 2, 2, 2, 2, 2, 2, 2, 2, 2, 4 ),
 ( 0.01819865299508306375, 0.01933465672311147215, 0.02047066045113988403, 0.02103866231515407956, 0.02160666417916827509, 0.02217466604318247062, 0.02274266790719666614, 0.02387867163522502945, 0.02501467536325339275, 0.02615067909128175605, 0.02671868095529594117, 0.02728668281931011935, 0.02785468468332430100, 0.02842268654733848265, 0.02955869027536688412, 0.03069469400339528906, 0.03183069773142369052, 0.03296670145945209546, 0.03353470332346629446, 0.03410270518748049345, 0.03523870891550889839, 0.03637471264353730332 ),
 .UNSPECIFIED. ) ;
#33109 = EDGE_LOOP ( 'NONE', ( #24722, #7929, #33958, #9902 ) ) ;
#33110 = ORIENTED_EDGE ( 'NONE', *, *, #15657, .T. ) ;
#33111 = LINE ( 'NONE', #28129, #23776 ) ;
#33112 = DIRECTION ( 'NONE',  ( 0.000000000000000000, 1.000000000000000000, 5.145227585319922065E-49 ) ) ;
#33113 = ORIENTED_EDGE ( 'NONE', *, *, #14231, .T. ) ;
#33114 = CARTESIAN_POINT ( 'NONE',  ( 9.199999999999999289, -11.69134295108991850, -6.750000000000008882 ) ) ;
#33115 = CARTESIAN_POINT ( 'NONE',  ( -100.5759650167679951, -2.572809509134356354, -12.23328267615805665 ) ) ;
#33116 = CONTEXT_DEPENDENT_SHAPE_REPRESENTATION ( #31061, #34900 ) ;
#33118 = DIRECTION ( 'NONE',  ( 1.000000000000000000, -0.000000000000000000, -0.000000000000000000 ) ) ;
#33117 = DIRECTION ( 'NONE',  ( -3.469446951953832974E-18, -1.000000000000000000, -7.888609052210116302E-31 ) ) ;
#33119 = VERTEX_POINT ( 'NONE', #11268 ) ;
#33120 = ORIENTED_EDGE ( 'NONE', *, *, #29581, .T. ) ;
#33121 = DIRECTION ( 'NONE',  ( -1.000000000000000000, 0.000000000000000000, -0.000000000000000000 ) ) ;
#33122 = ADVANCED_FACE ( 'NONE', ( #25303 ), #30119, .T. ) ;
#33123 = FACE_OUTER_BOUND ( 'NONE', #29785, .T. ) ;
#33124 = DIRECTION ( 'NONE',  ( -1.000000000000000000, 0.000000000000000000, 0.000000000000000000 ) ) ;
#33125 = LINE ( 'NONE', #30468, #7016 ) ;
#33126 = ORIENTED_EDGE ( 'NONE', *, *, #682, .F. ) ;
#33127 = CARTESIAN_POINT ( 'NONE',  ( -500.0000000000000000, -109.0000000000000142, 187.0000000000000000 ) ) ;
#33128 = CARTESIAN_POINT ( 'NONE',  ( 0.000000000000000000, 3.524919873834583163E-15, 68.31122994652405112 ) ) ;
#33129 = FACE_OUTER_BOUND ( 'NONE', #24464, .T. ) ;
#33130 = VECTOR ( 'NONE', #15649, 1000.000000000000000 ) ;
#33131 = VECTOR ( 'NONE', #4659, 1000.000000000000000 ) ;
#33132 = ORIENTED_EDGE ( 'NONE', *, *, #22190, .F. ) ;
#33133 = CARTESIAN_POINT ( 'NONE',  ( 15.44711578872682267, -28.64595934308657377, 49.43553178847298568 ) ) ;
#33134 = EDGE_CURVE ( 'NONE', #13146, #34260, #16208, .T. ) ;
#33135 = CARTESIAN_POINT ( 'NONE',  ( -499.9999999999998863, -109.0000000000000142, -162.9999999999999716 ) ) ;
#33136 = CARTESIAN_POINT ( 'NONE',  ( 35.63428259149705468, -12.79065496477506869, 49.43553178847298568 ) ) ;
#33137 = EDGE_CURVE ( 'NONE', #11027, #28736, #3410, .T. ) ;
#33139 = DIRECTION ( 'NONE',  ( 1.000000000000000000, 0.000000000000000000, 0.000000000000000000 ) ) ;
#33138 = DIRECTION ( 'NONE',  ( 0.000000000000000000, 0.000000000000000000, -1.000000000000000000 ) ) ;
#33140 = EDGE_CURVE ( 'NONE', #19088, #28627, #16976, .T. ) ;
#33141 = UNCERTAINTY_MEASURE_WITH_UNIT (LENGTH_MEASURE( 1.000000000000000082E-05 ), #29332, 'distance_accuracy_value', 'NONE');
#33142 = PLANE ( 'NONE',  #14454 ) ;
#33143 = ORIENTED_EDGE ( 'NONE', *, *, #30883, .F. ) ;
#33144 = LINE ( 'NONE', #8760, #21849 ) ;
#33145 = PLANE ( 'NONE',  #9759 ) ;
#33146 = B_SPLINE_CURVE_WITH_KNOTS ( 'NONE', 3,
 ( #33351, #22687, #14685, #9320 ),
 .UNSPECIFIED., .F., .F.,
 ( 4, 4 ),
 ( 3.346525879968219986E-07, 0.0006880714927763689238 ),
 .UNSPECIFIED. ) ;
#33147 = CIRCLE ( 'NONE', #25185, 3.999999999999976019 ) ;
#33148 = ORIENTED_EDGE ( 'NONE', *, *, #8386, .T. ) ;
#33149 = ORIENTED_EDGE ( 'NONE', *, *, #19455, .F. ) ;
#33150 = AXIS2_PLACEMENT_3D ( 'NONE', #18688, #19036, #6524 ) ;
#33151 = AXIS2_PLACEMENT_3D ( 'NONE', #33761, #20247, #20417 ) ;
#33152 = VECTOR ( 'NONE', #27623, 1000.000000000000114 ) ;
#33153 = ORIENTED_EDGE ( 'NONE', *, *, #19986, .T. ) ;
#33154 = B_SPLINE_CURVE_WITH_KNOTS ( 'NONE', 3,
 ( #27011, #21596, #32434, #16447, #8058, #32792, #18936, #8416, #19289, #6834, #19871, #12385, #31067, #22884, #31237, #14713, #11862, #3985, #14882, #25535, #3640, #17390, #811, #28396, #3818, #15055, #8815, #30885, #9530, #28218, #30542, #30713, #23232, #12215, #17727, #33549, #33729, #1344, #1164, #12036, #1513, #19691 ),
 .UNSPECIFIED., .F., .F.,
 ( 4, 2, 2, 2, 2, 2, 2, 2, 2, 2, 2, 2, 2, 2, 2, 2, 2, 2, 2, 2, 4 ),
 ( 0.01884718663114543988, 0.01943499450852638824, 0.02002280238590734007, 0.02119841814066924027, 0.02237403389543114046, 0.02354964965019304066, 0.02472526540495494085, 0.02590088115971684452, 0.02707649691447874471, 0.02766430479185969654, 0.02825211266924064490, 0.02883992054662159674, 0.02942772842400254510, 0.03060334417876444529, 0.03177895993352634896, 0.03295457568828825262, 0.03413019144305015629, 0.03471799932043109771, 0.03530580719781203913, 0.03648142295257392198, 0.03765703870733580483 ),
 .UNSPECIFIED. ) ;
#33155 = EDGE_LOOP ( 'NONE', ( #14668, #569, #3554, #5285 ) ) ;
#33156 = ORIENTED_EDGE ( 'NONE', *, *, #21891, .F. ) ;
#33157 = LINE ( 'NONE', #24430, #32073 ) ;
#33158 = ITEM_DEFINED_TRANSFORMATION ( 'NONE', 'NONE', #17284,  #28566 ) ;
#33159 = ORIENTED_EDGE ( 'NONE', *, *, #1253, .F. ) ;
#33160 = DIRECTION ( 'NONE',  ( 0.000000000000000000, -1.310824597558155437E-49, -1.000000000000000000 ) ) ;
#33161 = DIRECTION ( 'NONE',  ( -1.000000000000000000, 0.000000000000000000, 0.000000000000000000 ) ) ;
#33162 = ORIENTED_EDGE ( 'NONE', *, *, #28945, .F. ) ;
#33163 = EDGE_LOOP ( 'NONE', ( #15364, #15952, #29052, #14623 ) ) ;
#33164 = LINE ( 'NONE', #11292, #2052 ) ;
#33165 = DIRECTION ( 'NONE',  ( -0.000000000000000000, 1.836970198721029934E-16, -1.000000000000000000 ) ) ;
#33166 = CARTESIAN_POINT ( 'NONE',  ( 0.000000000000000000, 3.524919873834583163E-15, 68.31122994652405112 ) ) ;
#33167 = CARTESIAN_POINT ( 'NONE',  ( -430.0000000000000000, -119.0000000000000000, 128.0000000000000000 ) ) ;
#33168 = CARTESIAN_POINT ( 'NONE',  ( -19.99999999999998934, 75.55999999999990280, -168.2400000000000091 ) ) ;
#33169 = ORIENTED_EDGE ( 'NONE', *, *, #19114, .F. ) ;
#33170 = CARTESIAN_POINT ( 'NONE',  ( -5.021133111224989953, -5.758675521474015291, -67.50000000000000000 ) ) ;
#33171 = AXIS2_PLACEMENT_3D ( 'NONE', #25290, #9101, #22639 ) ;
#33172 = CARTESIAN_POINT ( 'NONE',  ( 0.07098932641069075067, -3.385659728283963332, -31.51320498992189911 ) ) ;
#33173 = ORIENTED_EDGE ( 'NONE', *, *, #20451, .F. ) ;
#33174 = EDGE_CURVE ( 'NONE', #18486, #18999, #6243, .T. ) ;
#33175 = DIRECTION ( 'NONE',  ( 0.000000000000000000, 0.000000000000000000, -1.000000000000000000 ) ) ;
#33176 = CARTESIAN_POINT ( 'NONE',  ( -430.0000000000000000, 130.9999999999999716, 128.0000000000000000 ) ) ;
#33177 = EDGE_CURVE ( 'NONE', #32711, #14881, #29951, .T. ) ;
#33178 = LINE ( 'NONE', #27135, #18603 ) ;
#33179 = PRODUCT_DEFINITION_FORMATION_WITH_SPECIFIED_SOURCE ( 'ANY', '', #22286, .NOT_KNOWN. ) ;
#33180 = CARTESIAN_POINT ( 'NONE',  ( -3.250000000000000000, -5.838643359331793015, 3.930000000000000160 ) ) ;
#33181 = CYLINDRICAL_SURFACE ( 'NONE', #3127, 3.999999999999976019 ) ;
#33182 = EDGE_CURVE ( 'NONE', #11239, #30715, #25477, .T. ) ;
#33183 = CIRCLE ( 'NONE', #18972, 2.033421858999711951 ) ;
#33184 = AXIS2_PLACEMENT_3D ( 'NONE', #15924, #5028, #26574 ) ;
#33185 = CARTESIAN_POINT ( 'NONE',  ( -9.978866888775527855, 6.201984591278717041, -67.50000000000000000 ) ) ;
#33186 = ORIENTED_EDGE ( 'NONE', *, *, #18312, .T. ) ;
#33187 = ADVANCED_FACE ( 'NONE', ( #23507 ), #14819, .F. ) ;
#33189 = CARTESIAN_POINT ( 'NONE',  ( 35.44043929807611448, -17.65143121711728469, 5.690671783530174999 ) ) ;
#33188 = CARTESIAN_POINT ( 'NONE',  ( 110.7380848894536598, 7.027127293105237708E-16, 57.49999999999999289 ) ) ;
#33190 = ORIENTED_EDGE ( 'NONE', *, *, #10859, .F. ) ;
#33191 = CARTESIAN_POINT ( 'NONE',  ( -32.37866696771086339, 3.290334066652079947, 68.31122994652405112 ) ) ;
#33192 = FACE_OUTER_BOUND ( 'NONE', #9745, .T. ) ;
#33193 = EDGE_CURVE ( 'NONE', #34596, #7115, #12383, .T. ) ;
#33194 = VERTEX_POINT ( 'NONE', #4099 ) ;
#33195 = VECTOR ( 'NONE', #641, 1000.000000000000000 ) ;
#33196 = VERTEX_POINT ( 'NONE', #28848 ) ;
#33197 = CARTESIAN_POINT ( 'NONE',  ( -70.00000000000000000, 4.559999999999908127, 168.2400000000000091 ) ) ;
#33198 = DIRECTION ( 'NONE',  ( 0.000000000000000000, 0.000000000000000000, 1.000000000000000000 ) ) ;
#33199 = ORIENTED_EDGE ( 'NONE', *, *, #25602, .T. ) ;
#33200 = ORIENTED_EDGE ( 'NONE', *, *, #21992, .F. ) ;
#33201 = CARTESIAN_POINT ( 'NONE',  ( -5.344999999999999751, 1.414467053015192657E-16, -0.7500000000000000000 ) ) ;
#33202 = AXIS2_PLACEMENT_3D ( 'NONE', #6052, #8915, #11413 ) ;
#33203 = AXIS2_PLACEMENT_3D ( 'NONE', #290, #13994, #11153 ) ;
#33204 = DIRECTION ( 'NONE',  ( -1.000000000000000000, 0.000000000000000000, -0.000000000000000000 ) ) ;
#33205 = AXIS2_PLACEMENT_3D ( 'NONE', #18235, #9852, #1839 ) ;
#33206 = CARTESIAN_POINT ( 'NONE',  ( 11.99999999999995559, -145.0000000000000000, 162.9999999999999716 ) ) ;
#33207 = CARTESIAN_POINT ( 'NONE',  ( -499.9999999999999432, 136.9999999999999432, -155.0000000000000000 ) ) ;
#33208 = ORIENTED_EDGE ( 'NONE', *, *, #4038, .F. ) ;
#33209 = ORIENTED_EDGE ( 'NONE', *, *, #18858, .T. ) ;
#33210 = VECTOR ( 'NONE', #10337, 1000.000000000000000 ) ;
#33211 = CARTESIAN_POINT ( 'NONE',  ( 60.00000000000000000, -33.69708579775584667, 49.43553178847298568 ) ) ;
#33212 = DIRECTION ( 'NONE',  ( 1.000000000000000000, 0.000000000000000000, 0.000000000000000000 ) ) ;
#33213 = FACE_OUTER_BOUND ( 'NONE', #13566, .T. ) ;
#33214 = CIRCLE ( 'NONE', #26961, 2.000000000000001776 ) ;
#33215 = CARTESIAN_POINT ( 'NONE',  ( -143.0000000000000568, -90.29102463692674974, -73.95413108702814498 ) ) ;
#33216 = CARTESIAN_POINT ( 'NONE',  ( -442.0000000000000000, -105.0000000000000142, 187.0000000000000000 ) ) ;
#33217 = CARTESIAN_POINT ( 'NONE',  ( -442.0000000000000000, -105.0000000000000142, 162.9999999999999716 ) ) ;
#33218 = LINE ( 'NONE', #833, #11315 ) ;
#33219 = ORIENTED_EDGE ( 'NONE', *, *, #15040, .T. ) ;
#33220 = FACE_BOUND ( 'NONE', #18261, .T. ) ;
#33221 = LINE ( 'NONE', #12408, #11471 ) ;
#33222 = EDGE_CURVE ( 'NONE', #27222, #32157, #25276, .T. ) ;
#33223 = CARTESIAN_POINT ( 'NONE',  ( 2.789999999999999147, -0.09145294252698496495, 30.47036804522407749 ) ) ;
#33224 = ORIENTED_EDGE ( 'NONE', *, *, #28057, .T. ) ;
#33225 = AXIS2_PLACEMENT_3D ( 'NONE', #12340, #4297, #33866 ) ;
#33226 = FACE_OUTER_BOUND ( 'NONE', #4204, .T. ) ;
#33227 = ORIENTED_EDGE ( 'NONE', *, *, #12870, .T. ) ;
#33228 = EDGE_CURVE ( 'NONE', #5130, #23546, #12324, .T. ) ;
#33229 = CARTESIAN_POINT ( 'NONE',  ( -35.00000000000000000, 3.432458613951613557, 15.93718699791191185 ) ) ;
#33230 = CIRCLE ( 'NONE', #20737, 7.999999999999979572 ) ;
#33231 = PLANE ( 'NONE',  #17765 ) ;
#33232 = EDGE_CURVE ( 'NONE', #32751, #3477, #28338, .T. ) ;
#33233 = LINE ( 'NONE', #8030, #18128 ) ;
#33234 = AXIS2_PLACEMENT_3D ( 'NONE', #20716, #15382, #25520 ) ;
#33235 = EDGE_LOOP ( 'NONE', ( #20751, #18726, #17269, #16676 ) ) ;
#33236 = EDGE_CURVE ( 'NONE', #30543, #23102, #25651, .T. ) ;
#33237 = EDGE_CURVE ( 'NONE', #23877, #28310, #28130, .T. ) ;
#33238 = VECTOR ( 'NONE', #3896, 1000.000000000000000 ) ;
#33239 = CARTESIAN_POINT ( 'NONE',  ( -3.250000000000000000, 5.404196845913421754, -0.7500000000000000000 ) ) ;
#33240 = CARTESIAN_POINT ( 'NONE',  ( 0.000000000000000000, 3.524919873834583163E-15, 68.31122994652405112 ) ) ;
#33241 = CARTESIAN_POINT ( 'NONE',  ( -500.0000000000000000, -113.0000000000000000, -155.0000000000000000 ) ) ;
#33242 = AXIS2_PLACEMENT_3D ( 'NONE', #340, #865, #8515 ) ;
#33243 = ORIENTED_EDGE ( 'NONE', *, *, #22676, .F. ) ;
#33244 = CARTESIAN_POINT ( 'NONE',  ( 836.7451374655331620, 1164.392891999947324, 1753.598338701303419 ) ) ;
#33245 = DIRECTION ( 'NONE',  ( 0.000000000000000000, 0.000000000000000000, 1.000000000000000000 ) ) ;
#33246 = ORIENTED_EDGE ( 'NONE', *, *, #34109, .F. ) ;
#33247 = CARTESIAN_POINT ( 'NONE',  ( 0.000000000000000000, -25.83993731729781729, -18.77381338200996552 ) ) ;
#33248 = ADVANCED_FACE ( 'NONE', ( #9109 ), #22818, .F. ) ;
#33249 = CARTESIAN_POINT ( 'NONE',  ( 2.630124765083918348, -1.866624223957557893, 5.429999999999999716 ) ) ;
#33250 = AXIS2_PLACEMENT_3D ( 'NONE', #22796, #28656, #19955 ) ;
#33251 = FACE_OUTER_BOUND ( 'NONE', #28526, .T. ) ;
#33252 = CARTESIAN_POINT ( 'NONE',  ( -347.0000000000000000, -125.0000000000000284, 181.0000000000000000 ) ) ;
#33253 = VERTEX_POINT ( 'NONE', #20672 ) ;
#33254 = ORIENTED_EDGE ( 'NONE', *, *, #8348, .T. ) ;
#33255 = ORIENTED_EDGE ( 'NONE', *, *, #10011, .F. ) ;
#33256 = DIRECTION ( 'NONE',  ( 0.000000000000000000, 2.309213040847544338E-50, 1.000000000000000000 ) ) ;
#33257 = VECTOR ( 'NONE', #10239, 1000.000000000000000 ) ;
#33258 = DIRECTION ( 'NONE',  ( 0.000000000000000000, 1.000000000000000000, -6.842277657836020854E-49 ) ) ;
#33259 = DIRECTION ( 'NONE',  ( 0.000000000000000000, 1.000000000000000000, 1.224646799147353207E-16 ) ) ;
#33260 = CARTESIAN_POINT ( 'NONE',  ( 2.783107609940381533, 11.66157578832064345, 28.58237449055242152 ) ) ;
#33261 = VERTEX_POINT ( 'NONE', #3929 ) ;
#33262 = ORIENTED_EDGE ( 'NONE', *, *, #5883, .T. ) ;
#33263 = FACE_OUTER_BOUND ( 'NONE', #21929, .T. ) ;
#33264 = VERTEX_POINT ( 'NONE', #9290 ) ;
#33265 = VECTOR ( 'NONE', #33534, 1000.000000000000000 ) ;
#33266 = DIRECTION ( 'NONE',  ( -1.000000000000000000, -0.000000000000000000, -0.000000000000000000 ) ) ;
#33267 = CARTESIAN_POINT ( 'NONE',  ( -20.00000000000004619, 112.9999999999999574, 155.0000000000000000 ) ) ;
#33268 = ORIENTED_EDGE ( 'NONE', *, *, #23510, .F. ) ;
#33269 = ORIENTED_EDGE ( 'NONE', *, *, #32793, .T. ) ;
#33270 = SURFACE_SIDE_STYLE ('',( #3884 ) ) ;
#33271 = DIRECTION ( 'NONE',  ( -0.000000000000000000, -0.000000000000000000, 1.000000000000000000 ) ) ;
#33272 = ORIENTED_EDGE ( 'NONE', *, *, #28791, .T. ) ;
#33273 = CARTESIAN_POINT ( 'NONE',  ( 0.000000000000000000, 29.94779062842788164, 5.619744560739158068 ) ) ;
#33274 = CARTESIAN_POINT ( 'NONE',  ( 34.58310883014599568, -15.42890216704096851, 49.43553178847298568 ) ) ;
#33275 = DIRECTION ( 'NONE',  ( -0.000000000000000000, 1.000000000000000000, -0.000000000000000000 ) ) ;
#33276 = LINE ( 'NONE', #6865, #29918 ) ;
#33277 = CIRCLE ( 'NONE', #24784, 2.525000000000000799 ) ;
#33278 = EDGE_CURVE ( 'NONE', #319, #28991, #15166, .T. ) ;
#33279 = EDGE_CURVE ( 'NONE', #30178, #30541, #13937, .T. ) ;
#33280 = VECTOR ( 'NONE', #25516, 1000.000000000000000 ) ;
#33281 = CARTESIAN_POINT ( 'NONE',  ( 0.7561992229685223776, -1.599833918847833880, 33.87742110695030107 ) ) ;
#33282 = DIRECTION ( 'NONE',  ( 0.000000000000000000, 1.000000000000000000, 0.000000000000000000 ) ) ;
#33283 = PLANE ( 'NONE',  #29084 ) ;
#33284 = VECTOR ( 'NONE', #4140, 1000.000000000000000 ) ;
#33285 = ORIENTED_EDGE ( 'NONE', *, *, #2637, .T. ) ;
#33286 = VERTEX_POINT ( 'NONE', #17670 ) ;
#33287 = DIRECTION ( 'NONE',  ( 2.631201909438060269E-14, -5.396010391056495992E-16, 0.9999999999999998890 ) ) ;
#33288 =( REPRESENTATION_RELATIONSHIP ('NONE','NONE', #23037, #15767 ) REPRESENTATION_RELATIONSHIP_WITH_TRANSFORMATION ( #3561 )SHAPE_REPRESENTATION_RELATIONSHIP( ) );
#33289 = VERTEX_POINT ( 'NONE', #20495 ) ;
#33290 = VECTOR ( 'NONE', #7472, 1000.000000000000000 ) ;
#33291 = ORIENTED_EDGE ( 'NONE', *, *, #11136, .T. ) ;
#33292 = EDGE_CURVE ( 'NONE', #34395, #6886, #5984, .T. ) ;
#33293 = CARTESIAN_POINT ( 'NONE',  ( -499.9999999999999432, -137.0000000000000000, -190.9999999999999716 ) ) ;
#33294 = DIRECTION ( 'NONE',  ( 0.000000000000000000, 1.836970198721029441E-16, -1.000000000000000000 ) ) ;
#33295 = APPLICATION_PROTOCOL_DEFINITION ( 'draft international standard', 'automotive_design', 1998, #29182 ) ;
#33296 = VERTEX_POINT ( 'NONE', #34017 ) ;
#33297 = DIRECTION ( 'NONE',  ( 1.000000000000000000, 0.000000000000000000, 5.546364386991661285E-52 ) ) ;
#33298 = EDGE_CURVE ( 'NONE', #32277, #14545, #28677, .T. ) ;
#33299 = ADVANCED_FACE ( 'NONE', ( #26004, #1622 ), #23336, .T. ) ;
#33300 = CONTEXT_DEPENDENT_SHAPE_REPRESENTATION ( #14011, #32325 ) ;
#33301 = EDGE_CURVE ( 'NONE', #32672, #6398, #22136, .T. ) ;
#33302 = CIRCLE ( 'NONE', #22517, 32.54542015209054995 ) ;
#33304 = DIRECTION ( 'NONE',  ( -1.000000000000000000, 0.000000000000000000, 0.000000000000000000 ) ) ;
#33303 = DIRECTION ( 'NONE',  ( 0.000000000000000000, -6.123233995736766036E-17, -1.000000000000000000 ) ) ;
#33305 = ORIENTED_EDGE ( 'NONE', *, *, #33922, .F. ) ;
#33306 = ORIENTED_EDGE ( 'NONE', *, *, #27125, .T. ) ;
#33307 = DIRECTION ( 'NONE',  ( 0.8276889981568904542, -0.5611870653623824978, 0.000000000000000000 ) ) ;
#33308 = VECTOR ( 'NONE', #29859, 1000.000000000000000 ) ;
#33309 = EDGE_CURVE ( 'NONE', #22892, #7203, #13024, .T. ) ;
#33310 = DIRECTION ( 'NONE',  ( 0.05413890858541543089, 0.9985334138511240409, 0.000000000000000000 ) ) ;
#33311 = DIRECTION ( 'NONE',  ( 0.000000000000000000, -0.000000000000000000, -1.000000000000000000 ) ) ;
#33312 = DIRECTION ( 'NONE',  ( -1.000000000000000000, -0.000000000000000000, -0.000000000000000000 ) ) ;
#33313 = ORIENTED_EDGE ( 'NONE', *, *, #31412, .F. ) ;
#33314 = CARTESIAN_POINT ( 'NONE',  ( -499.9999999999999432, 112.9999999999999574, -190.9999999999999716 ) ) ;
#33315 = DIRECTION ( 'NONE',  ( 1.000000000000000000, 0.000000000000000000, 5.546364386991661285E-52 ) ) ;
#33316 = CYLINDRICAL_SURFACE ( 'NONE', #19800, 1.154999999999999805 ) ;
#33317 = ORIENTED_EDGE ( 'NONE', *, *, #1589, .T. ) ;
#33318 = AXIS2_PLACEMENT_3D ( 'NONE', #25259, #15085, #3545 ) ;
#33319 = CARTESIAN_POINT ( 'NONE',  ( -143.0000000000000568, -175.8248315648716016, -46.05325008164006562 ) ) ;
#33320 = CARTESIAN_POINT ( 'NONE',  ( 0.000000000000000000, 2.296212748401288367E-15, 47.49999999999999289 ) ) ;
#33321 = LINE ( 'NONE', #17503, #7562 ) ;
#33323 = LINE ( 'NONE', #9110, #19107 ) ;
#33322 = DIRECTION ( 'NONE',  ( 0.000000000000000000, 0.000000000000000000, 1.000000000000000000 ) ) ;
#33324 = LINE ( 'NONE', #20331, #21272 ) ;
#33325 = VERTEX_POINT ( 'NONE', #26352 ) ;
#33326 = CARTESIAN_POINT ( 'NONE',  ( -31.87924797510909869, -6.551177101682124970, 68.31122994652405112 ) ) ;
#33327 = CYLINDRICAL_SURFACE ( 'NONE', #16666, 7.999999999999979572 ) ;
#33328 = PRODUCT_DEFINITION_SHAPE ( 'NONE', 'NONE',  #35164 ) ;
#33329 = AXIS2_PLACEMENT_3D ( 'NONE', #9795, #9098, #20657 ) ;
#33330 = ORIENTED_EDGE ( 'NONE', *, *, #25717, .F. ) ;
#33331 = AXIS2_PLACEMENT_3D ( 'NONE', #5059, #16124, #31940 ) ;
#33332 = ORIENTED_EDGE ( 'NONE', *, *, #5675, .F. ) ;
#33333 = ORIENTED_EDGE ( 'NONE', *, *, #20886, .F. ) ;
#33334 = CARTESIAN_POINT ( 'NONE',  ( -45.00000000000000000, -4.831299144296466785, 15.81122994652406355 ) ) ;
#33335 = ORIENTED_EDGE ( 'NONE', *, *, #13932, .F. ) ;
#33336 = ORIENTED_EDGE ( 'NONE', *, *, #8643, .F. ) ;
#33337 = DIRECTION ( 'NONE',  ( -1.000000000000000000, -3.469446951953834515E-18, 0.000000000000000000 ) ) ;
#33338 = AXIS2_PLACEMENT_3D ( 'NONE', #29820, #5422, #21631 ) ;
#33339 = ADVANCED_FACE ( 'NONE', ( #15697 ), #24022, .F. ) ;
#33340 = ADVANCED_FACE ( 'NONE', ( #16704 ), #5808, .F. ) ;
#33341 = ORIENTED_EDGE ( 'NONE', *, *, #17193, .T. ) ;
#33342 = DIRECTION ( 'NONE',  ( 0.000000000000000000, 0.000000000000000000, 1.000000000000000000 ) ) ;
#33343 = CARTESIAN_POINT ( 'NONE',  ( -349.0000000000000000, -125.0000000000000284, 185.0000000000000000 ) ) ;
#33344 = ORIENTED_EDGE ( 'NONE', *, *, #26968, .F. ) ;
#33345 = ORIENTED_EDGE ( 'NONE', *, *, #13300, .F. ) ;
#33346 = DIRECTION ( 'NONE',  ( -1.000000000000000000, 2.530127506375325948E-80, -1.848892746611746419E-32 ) ) ;
#33347 = DIRECTION ( 'NONE',  ( -1.000000000000000000, 0.000000000000000000, 0.000000000000000000 ) ) ;
#33348 = VECTOR ( 'NONE', #31846, 1000.000000000000000 ) ;
#33349 = CARTESIAN_POINT ( 'NONE',  ( -7.057945688734196724E-17, 18.19930456030807164, -24.67628137665877830 ) ) ;
#33350 = DIRECTION ( 'NONE',  ( 0.000000000000000000, 1.000000000000000000, 1.224646799147353207E-16 ) ) ;
#33351 = CARTESIAN_POINT ( 'NONE',  ( 2.765921099433444663, 29.44518845714764765, 9.980709654879525772 ) ) ;
#33352 = ORIENTED_EDGE ( 'NONE', *, *, #13428, .T. ) ;
#33353 = VECTOR ( 'NONE', #27044, 1000.000000000000000 ) ;
#33354 = LINE ( 'NONE', #29806, #12292 ) ;
#33355 = CARTESIAN_POINT ( 'NONE',  ( 0.000000000000000000, -23.41952779159775488, 19.49300927180538778 ) ) ;
#33356 = VERTEX_POINT ( 'NONE', #14023 ) ;
#33357 = LINE ( 'NONE', #789, #3777 ) ;
#33358 = CARTESIAN_POINT ( 'NONE',  ( -28.00450684652667022, 16.58167570419054471, 68.31122994652405112 ) ) ;
#33359 = LINE ( 'NONE', #30522, #31442 ) ;
#33360 = CARTESIAN_POINT ( 'NONE',  ( 19.99999999999998224, 134.9999999999999432, -162.9999999999999432 ) ) ;
#33361 = FACE_OUTER_BOUND ( 'NONE', #30141, .T. ) ;
#33362 = VECTOR ( 'NONE', #10801, 1000.000000000000000 ) ;
#33363 = CARTESIAN_POINT ( 'NONE',  ( 0.000000000000000000, 0.000000000000000000, 0.000000000000000000 ) ) ;
#33364 = EDGE_LOOP ( 'NONE', ( #16502, #1258 ) ) ;
#33365 = CARTESIAN_POINT ( 'NONE',  ( -20.00000000000001776, -113.0000000000000000, 187.0000000000000000 ) ) ;
#33366 = LINE ( 'NONE', #19858, #6876 ) ;
#33367 = B_SPLINE_CURVE_WITH_KNOTS ( 'NONE', 3,
 ( #7034, #20738, #8090, #267 ),
 .UNSPECIFIED., .F., .F.,
 ( 4, 4 ),
 ( 3.668583969211562668E-07, 0.0006881039678813115779 ),
 .UNSPECIFIED. ) ;
#33368 = ORIENTED_EDGE ( 'NONE', *, *, #150, .T. ) ;
#33369 = CYLINDRICAL_SURFACE ( 'NONE', #28547, 1.154999999999999805 ) ;
#33370 = FACE_OUTER_BOUND ( 'NONE', #11396, .T. ) ;
#33371 = VECTOR ( 'NONE', #10244, 1000.000000000000000 ) ;
#33372 = ORIENTED_EDGE ( 'NONE', *, *, #273, .F. ) ;
#33373 = AXIS2_PLACEMENT_3D ( 'NONE', #11169, #27700, #13834 ) ;
#33374 = VECTOR ( 'NONE', #6068, 1000.000000000000000 ) ;
#33375 = VERTEX_POINT ( 'NONE', #32873 ) ;
#33376 = CARTESIAN_POINT ( 'NONE',  ( -410.0000000000000568, 137.0000000000000000, -175.0000000000000000 ) ) ;
#33377 = EDGE_LOOP ( 'NONE', ( #6356, #8876, #23440, #22812 ) ) ;
#33378 = VERTEX_POINT ( 'NONE', #27355 ) ;
#33379 = CARTESIAN_POINT ( 'NONE',  ( -19.99999999999998934, 134.9999999999998863, 162.9999999999999716 ) ) ;
#33380 = ADVANCED_FACE ( 'NONE', ( #5630 ), #12847, .F. ) ;
#33382 = CARTESIAN_POINT ( 'NONE',  ( 0.000000000000000000, 28.95078156989571738, -9.502838467757779739 ) ) ;
#33381 = AXIS2_PLACEMENT_3D ( 'NONE', #9880, #23586, #1695 ) ;
#33383 = EDGE_CURVE ( 'NONE', #15713, #26361, #18502, .T. ) ;
#33384 = DIRECTION ( 'NONE',  ( 1.000000000000000000, 0.000000000000000000, 0.000000000000000000 ) ) ;
#33385 = CARTESIAN_POINT ( 'NONE',  ( 0.000000000000000000, 0.000000000000000000, 0.000000000000000000 ) ) ;
#33386 = ORIENTED_EDGE ( 'NONE', *, *, #14026, .F. ) ;
#33387 = ORIENTED_EDGE ( 'NONE', *, *, #34373, .F. ) ;
#33388 = CARTESIAN_POINT ( 'NONE',  ( 0.02407890056655564992, -30.46391896562411716, 6.211548095912460710 ) ) ;
#33389 = DIRECTION ( 'NONE',  ( -0.000000000000000000, -1.836970198721029688E-16, 1.000000000000000000 ) ) ;
#33390 = EDGE_CURVE ( 'NONE', #7267, #2456, #34375, .T. ) ;
#33391 = CARTESIAN_POINT ( 'NONE',  ( -30.58418286738120884, -22.31615353445080174, 68.31122994652405112 ) ) ;
#33392 = LINE ( 'NONE', #19051, #3332 ) ;
#33393 = DIRECTION ( 'NONE',  ( -0.000000000000000000, -0.000000000000000000, -1.000000000000000000 ) ) ;
#33394 = DIRECTION ( 'NONE',  ( 0.000000000000000000, -1.000000000000000000, 3.374343856708137958E-53 ) ) ;
#33395 = AXIS2_PLACEMENT_3D ( 'NONE', #15068, #7022, #17575 ) ;
#33396 = CARTESIAN_POINT ( 'NONE',  ( 2.397606348813468014, 30.27116788627787614, 13.00174666746673324 ) ) ;
#33397 = VERTEX_POINT ( 'NONE', #13195 ) ;
#33398 = DIRECTION ( 'NONE',  ( 1.000000000000000000, 0.000000000000000000, 0.000000000000000000 ) ) ;
#33399 = FACE_OUTER_BOUND ( 'NONE', #5687, .T. ) ;
#33400 = CARTESIAN_POINT ( 'NONE',  ( -5.527271473480783293, -1.747512292859696226, 5.429999999999999716 ) ) ;
#33401 = VERTEX_POINT ( 'NONE', #10520 ) ;
#33402 = VECTOR ( 'NONE', #12991, 1000.000000000000000 ) ;
#33403 = VECTOR ( 'NONE', #5969, 1000.000000000000000 ) ;
#33404 = CARTESIAN_POINT ( 'NONE',  ( -363.0000000000000000, 124.9999999999999432, 168.9999999999999716 ) ) ;
#33405 = ORIENTED_EDGE ( 'NONE', *, *, #2955, .T. ) ;
#33406 = DIRECTION ( 'NONE',  ( 0.000000000000000000, 1.836970198721030181E-16, -1.000000000000000000 ) ) ;
#33407 = DIRECTION ( 'NONE',  ( 0.000000000000000000, -2.309213040847544338E-50, -1.000000000000000000 ) ) ;
#33408 = TOROIDAL_SURFACE ( 'NONE', #19779, 30.47050528711511674, 8.000000000000000000 ) ;
#33409 = VERTEX_POINT ( 'NONE', #19364 ) ;
#33410 = CARTESIAN_POINT ( 'NONE',  ( -5.469264258321805627, 1.713938105891546382, 0.000000000000000000 ) ) ;
#33411 = DIRECTION ( 'NONE',  ( 0.000000000000000000, -1.310824597558155437E-49, -1.000000000000000000 ) ) ;
#33412 = DIRECTION ( 'NONE',  ( -0.000000000000000000, -0.000000000000000000, -1.000000000000000000 ) ) ;
#33413 = ORIENTED_EDGE ( 'NONE', *, *, #17908, .F. ) ;
#33414 = VECTOR ( 'NONE', #11644, 1000.000000000000000 ) ;
#33415 = CARTESIAN_POINT ( 'NONE',  ( 840.8943870737551833, 1125.614262950047532, 1753.598338701303646 ) ) ;
#33416 = DIRECTION ( 'NONE',  ( 0.000000000000000000, 1.000000000000000000, 0.000000000000000000 ) ) ;
#33417 = ORIENTED_EDGE ( 'NONE', *, *, #23868, .T. ) ;
#33418 = DIRECTION ( 'NONE',  ( 1.000000000000000000, -1.270085550689488560E-30, -2.891205793294675368E-16 ) ) ;
#33419 = ADVANCED_FACE ( 'NONE', ( #34721 ), #10334, .T. ) ;
#33420 = CARTESIAN_POINT ( 'NONE',  ( -442.0000000000000000, -109.0000000000000142, -155.0000000000000000 ) ) ;
#33421 = CIRCLE ( 'NONE', #14625, 2.524999999999999467 ) ;
#33422 = VECTOR ( 'NONE', #21525, 1000.000000000000000 ) ;
#33423 = DIRECTION ( 'NONE',  ( -1.000000000000000000, -0.000000000000000000, -0.000000000000000000 ) ) ;
#33424 = DIRECTION ( 'NONE',  ( -1.000000000000000000, 0.000000000000000000, 0.000000000000000000 ) ) ;
#33425 = ITEM_DEFINED_TRANSFORMATION ( 'NONE', 'NONE', #15562,  #28566 ) ;
#33426 = ORIENTED_EDGE ( 'NONE', *, *, #9035, .T. ) ;
#33427 = EDGE_LOOP ( 'NONE', ( #244, #8040, #1880, #11966 ) ) ;
#33428 = EDGE_LOOP ( 'NONE', ( #25597, #19558, #7670, #34710 ) ) ;
#33429 = EDGE_CURVE ( 'NONE', #27638, #23842, #30205, .T. ) ;
#33430 = SURFACE_STYLE_FILL_AREA ( #30941 ) ;
#33431 = CARTESIAN_POINT ( 'NONE',  ( -10.84269519964070305, -36.27449394610879096, 68.31122994652405112 ) ) ;
#33432 = CARTESIAN_POINT ( 'NONE',  ( 2.783128911662848370, -23.57967537501747302, -19.92301408446885347 ) ) ;
#33433 = DIRECTION ( 'NONE',  ( 1.000000000000000000, 0.000000000000000000, 0.000000000000000000 ) ) ;
#33434 = ORIENTED_EDGE ( 'NONE', *, *, #16125, .T. ) ;
#33435 = EDGE_LOOP ( 'NONE', ( #31604, #2887, #9340, #28937 ) ) ;
#33436 = ADVANCED_FACE ( 'NONE', ( #11181 ), #20840, .T. ) ;
#33437 = CARTESIAN_POINT ( 'NONE',  ( -12.00000000000001066, 144.9999999999999716, -155.0000000000000000 ) ) ;
#33438 = CARTESIAN_POINT ( 'NONE',  ( -418.0000000000000000, 105.0000000000000142, -101.9999999999999858 ) ) ;
#33439 = ORIENTED_EDGE ( 'NONE', *, *, #13471, .F. ) ;
#33440 = CARTESIAN_POINT ( 'NONE',  ( 2.765921099433443331, 26.03801215795517621, 16.98986790278620873 ) ) ;
#33441 = EDGE_CURVE ( 'NONE', #18325, #18475, #21017, .T. ) ;
#33442 = CARTESIAN_POINT ( 'NONE',  ( 26.97014235612466493, -26.57093094961043889, 68.31122994652405112 ) ) ;
#33443 = AXIS2_PLACEMENT_3D ( 'NONE', #18538, #9798, #10325 ) ;
#33444 = ORIENTED_EDGE ( 'NONE', *, *, #21571, .F. ) ;
#33445 = ORIENTED_EDGE ( 'NONE', *, *, #34382, .T. ) ;
#33446 = DIRECTION ( 'NONE',  ( 0.000000000000000000, 0.000000000000000000, -1.000000000000000000 ) ) ;
#33447 = AXIS2_PLACEMENT_3D ( 'NONE', #32584, #24756, #22100 ) ;
#33448 = DIRECTION ( 'NONE',  ( 0.7621620551276360178, -0.6473862847818281363, 0.000000000000000000 ) ) ;
#33449 = ORIENTED_EDGE ( 'NONE', *, *, #2386, .T. ) ;
#33450 = DIRECTION ( 'NONE',  ( 0.000000000000000000, 0.000000000000000000, -1.000000000000000000 ) ) ;
#33451 = SURFACE_STYLE_FILL_AREA ( #16928 ) ;
#33452 = DIRECTION ( 'NONE',  ( 0.000000000000000000, 1.000000000000000000, 2.465190328815662439E-32 ) ) ;
#33453 = SURFACE_STYLE_USAGE ( .BOTH. , #8538 ) ;
#33454 = CARTESIAN_POINT ( 'NONE',  ( -109.4240349832319907, -2.572809509134357242, 12.23328267615805132 ) ) ;
#33455 = CYLINDRICAL_SURFACE ( 'NONE', #28686, 7.999999999999979572 ) ;
#33456 = DIRECTION ( 'NONE',  ( 0.000000000000000000, 0.000000000000000000, 1.000000000000000000 ) ) ;
#33457 = ORIENTED_EDGE ( 'NONE', *, *, #2567, .T. ) ;
#33458 = AXIS2_PLACEMENT_3D ( 'NONE', #7418, #10279, #28975 ) ;
#33459 = ORIENTED_EDGE ( 'NONE', *, *, #20323, .T. ) ;
#33460 = DIRECTION ( 'NONE',  ( 2.631201909438060269E-14, -5.396010391056495992E-16, 0.9999999999999998890 ) ) ;
#33461 = EDGE_LOOP ( 'NONE', ( #23431, #6394, #21867, #34779 ) ) ;
#33462 = ORIENTED_EDGE ( 'NONE', *, *, #18904, .F. ) ;
#33463 = CARTESIAN_POINT ( 'NONE',  ( 2.789999999999999147, -29.68817180695682723, 9.232883799364120847 ) ) ;
#33464 = CIRCLE ( 'NONE', #16442, 7.999999999999979572 ) ;
#33465 = CYLINDRICAL_SURFACE ( 'NONE', #28986, 34.41491905851385269 ) ;
#33466 = ITEM_DEFINED_TRANSFORMATION ( 'NONE', 'NONE', #12119,  #28566 ) ;
#33467 = ORIENTED_EDGE ( 'NONE', *, *, #9038, .F. ) ;
#33468 = DIRECTION ( 'NONE',  ( -0.000000000000000000, -0.000000000000000000, 1.000000000000000000 ) ) ;
#33469 = CARTESIAN_POINT ( 'NONE',  ( -104.6618752167676973, -5.114954807106460777, -11.40557921924218832 ) ) ;
#33470 = ADVANCED_FACE ( 'NONE', ( #31684 ), #15881, .F. ) ;
#33471 = B_SPLINE_CURVE_WITH_KNOTS ( 'NONE', 3,
 ( #19032, #29874, #30923, #3856 ),
 .UNSPECIFIED., .F., .F.,
 ( 4, 4 ),
 ( 2.038594426221743809E-07, 0.0006879396046783100693 ),
 .UNSPECIFIED. ) ;
#33473 = DIRECTION ( 'NONE',  ( 0.000000000000000000, 0.000000000000000000, 1.000000000000000000 ) ) ;
#33472 = DIRECTION ( 'NONE',  ( 0.000000000000000000, 0.000000000000000000, -1.000000000000000000 ) ) ;
#33474 = ORIENTED_EDGE ( 'NONE', *, *, #17723, .T. ) ;
#33475 = EDGE_LOOP ( 'NONE', ( #9746, #23960, #26546, #23597 ) ) ;
#33476 = ADVANCED_FACE ( 'NONE', ( #4614 ), #23578, .T. ) ;
#33477 = ADVANCED_FACE ( 'NONE', ( #30039 ), #29018, .F. ) ;
#33478 = CARTESIAN_POINT ( 'NONE',  ( 1.991296462759137853, -32.48444414290481319, -36.68877005347593467 ) ) ;
#33479 = FACE_OUTER_BOUND ( 'NONE', #12337, .T. ) ;
#33480 = DIRECTION ( 'NONE',  ( 0.000000000000000000, 0.000000000000000000, -1.000000000000000000 ) ) ;
#33481 = CARTESIAN_POINT ( 'NONE',  ( 3.235562306570555532E-30, 14.09580098603202458, -67.50000000000000000 ) ) ;
#33482 = ORIENTED_EDGE ( 'NONE', *, *, #19817, .F. ) ;
#33483 = VECTOR ( 'NONE', #17182, 1000.000000000000000 ) ;
#33484 = FACE_OUTER_BOUND ( 'NONE', #4012, .T. ) ;
#33485 = DIRECTION ( 'NONE',  ( -1.000000000000000000, 0.000000000000000000, 0.000000000000000000 ) ) ;
#33486 = ORIENTED_EDGE ( 'NONE', *, *, #22626, .T. ) ;
#33487 = PLANE ( 'NONE',  #12940 ) ;
#33488 = DIRECTION ( 'NONE',  ( 1.000000000000000000, 0.000000000000000000, -0.000000000000000000 ) ) ;
#33489 = EDGE_CURVE ( 'NONE', #23786, #16134, #17591, .T. ) ;
#33490 = LINE ( 'NONE', #27796, #2437 ) ;
#33492 = CYLINDRICAL_SURFACE ( 'NONE', #21933, 5.738084889453667792 ) ;
#33491 = DIRECTION ( 'NONE',  ( 0.000000000000000000, 1.836970198721029441E-16, -1.000000000000000000 ) ) ;
#33493 = AXIS2_PLACEMENT_3D ( 'NONE', #24930, #30466, #6059 ) ;
#33494 = PLANE ( 'NONE',  #9335 ) ;
#33495 = CARTESIAN_POINT ( 'NONE',  ( 2.789999999999999147, 30.93646776788796160, 7.943134866716423659 ) ) ;
#33496 = ORIENTED_EDGE ( 'NONE', *, *, #28341, .F. ) ;
#33497 = DIRECTION ( 'NONE',  ( -1.000000000000000000, -0.000000000000000000, -0.000000000000000000 ) ) ;
#33498 = CARTESIAN_POINT ( 'NONE',  ( -361.0000000000000000, -135.0000000000000000, 113.9999999999999858 ) ) ;
#33499 = EDGE_CURVE ( 'NONE', #23038, #5682, #3500, .T. ) ;
#33500 = VECTOR ( 'NONE', #19435, 1000.000000000000114 ) ;
#33501 = EDGE_CURVE ( 'NONE', #7081, #16235, #27712, .T. ) ;
#33502 = ORIENTED_EDGE ( 'NONE', *, *, #17772, .F. ) ;
#33503 = EDGE_CURVE ( 'NONE', #27359, #20509, #22912, .T. ) ;
#33504 = ORIENTED_EDGE ( 'NONE', *, *, #25868, .F. ) ;
#33505 = ORIENTED_EDGE ( 'NONE', *, *, #27606, .T. ) ;
#33506 = DIRECTION ( 'NONE',  ( -0.1617819965527614312, 0.9868265225415265851, 0.000000000000000000 ) ) ;
#33507 = ORIENTED_EDGE ( 'NONE', *, *, #13101, .F. ) ;
#33508 = ORIENTED_EDGE ( 'NONE', *, *, #19889, .T. ) ;
#33509 = CYLINDRICAL_SURFACE ( 'NONE', #17380, 2.000000000000001776 ) ;
#33510 = VECTOR ( 'NONE', #26694, 1000.000000000000000 ) ;
#33511 = VERTEX_POINT ( 'NONE', #28425 ) ;
#33512 = LINE ( 'NONE', #27997, #31165 ) ;
#33513 = LINE ( 'NONE', #11457, #2347 ) ;
#33514 = ORIENTED_EDGE ( 'NONE', *, *, #4683, .T. ) ;
#33515 = VERTEX_POINT ( 'NONE', #22202 ) ;
#33516 = EDGE_CURVE ( 'NONE', #19582, #6460, #9387, .T. ) ;
#33517 = EDGE_CURVE ( 'NONE', #769, #19238, #24156, .T. ) ;
#33518 = DIRECTION ( 'NONE',  ( 0.000000000000000000, -1.000000000000000000, -1.310824597558155437E-49 ) ) ;
#33519 = CARTESIAN_POINT ( 'NONE',  ( 0.000000000000000000, -31.68806325674609781, 4.003133335385473224 ) ) ;
#33520 = B_SPLINE_CURVE_WITH_KNOTS ( 'NONE', 3,
 ( #25538, #9534, #31240, #23236, #28575, #33911 ),
 .UNSPECIFIED., .F., .F.,
 ( 4, 2, 4 ),
 ( 4.404817032094653926E-07, 0.001874269626248360049, 0.003748098770793510670 ),
 .UNSPECIFIED. ) ;
#33521 = CARTESIAN_POINT ( 'NONE',  ( 15.99999999999997868, 136.9999999999999716, 155.0000000000000000 ) ) ;
#33522 = DIRECTION ( 'NONE',  ( 1.000000000000000000, 3.469446951953834515E-18, 0.000000000000000000 ) ) ;
#33523 = CARTESIAN_POINT ( 'NONE',  ( -21.41424479178918361, -24.50784553716277969, -36.68877005347593467 ) ) ;
#33524 = ORIENTED_EDGE ( 'NONE', *, *, #2196, .F. ) ;
#33525 = LINE ( 'NONE', #9507, #31028 ) ;
#33526 = CARTESIAN_POINT ( 'NONE',  ( 145.0000000000000568, 87.50000000000000000, 65.00000000000000000 ) ) ;
#33527 = VERTEX_POINT ( 'NONE', #33229 ) ;
#33528 = PRODUCT_DEFINITION_SHAPE ( 'NONE', 'NONE',  #35212 ) ;
#33529 = DIRECTION ( 'NONE',  ( -0.000000000000000000, -0.000000000000000000, -1.000000000000000000 ) ) ;
#33530 = DIRECTION ( 'NONE',  ( 0.000000000000000000, -0.000000000000000000, 1.000000000000000000 ) ) ;
#33531 = DIRECTION ( 'NONE',  ( 0.000000000000000000, 1.836970198721029934E-16, -1.000000000000000000 ) ) ;
#33532 = AXIS2_PLACEMENT_3D ( 'NONE', #908, #9087, #19953 ) ;
#33533 = CARTESIAN_POINT ( 'NONE',  ( 101.2248971821314569, 4.336304859840375059, -6.126759150192703451 ) ) ;
#33534 = DIRECTION ( 'NONE',  ( 0.000000000000000000, 1.000000000000000000, 0.000000000000000000 ) ) ;
#33535 = CARTESIAN_POINT ( 'NONE',  ( 11.99999999999999645, 144.9999999999999716, -190.9999999999999432 ) ) ;
#33536 = ORIENTED_EDGE ( 'NONE', *, *, #26906, .T. ) ;
#33537 = CARTESIAN_POINT ( 'NONE',  ( 2.789999999999999147, 6.312585643774966115, -29.77790610619679512 ) ) ;
#33539 = FACE_BOUND ( 'NONE', #7160, .T. ) ;
#33538 = CARTESIAN_POINT ( 'NONE',  ( -45.05956070192387841, -20.15143121711730245, 20.00000000000000000 ) ) ;
#33540 = EDGE_CURVE ( 'NONE', #27942, #2181, #8848, .T. ) ;
#33541 = EDGE_CURVE ( 'NONE', #2254, #30412, #11891, .T. ) ;
#33542 = EDGE_LOOP ( 'NONE', ( #11235, #28773, #20897, #32282 ) ) ;
#33543 =( REPRESENTATION_RELATIONSHIP ('NONE','NONE', #23037, #28231 ) REPRESENTATION_RELATIONSHIP_WITH_TRANSFORMATION ( #954 )SHAPE_REPRESENTATION_RELATIONSHIP( ) );
#33544 = CARTESIAN_POINT ( 'NONE',  ( 2.765921099433443775, -31.05158812718220673, -1.559667679918931738 ) ) ;
#33545 = VERTEX_POINT ( 'NONE', #25565 ) ;
#33546 = VERTEX_POINT ( 'NONE', #33042 ) ;
#33547 = EDGE_CURVE ( 'NONE', #30842, #19088, #27565, .T. ) ;
#33548 = ORIENTED_EDGE ( 'NONE', *, *, #4252, .T. ) ;
#33549 = CARTESIAN_POINT ( 'NONE',  ( 99.89373959579265261, -2.624171310066655938, -7.028111897042786715 ) ) ;
#33550 = ORIENTED_EDGE ( 'NONE', *, *, #8544, .F. ) ;
#33551 = ORIENTED_EDGE ( 'NONE', *, *, #1408, .T. ) ;
#33552 = FACE_OUTER_BOUND ( 'NONE', #32126, .T. ) ;
#33553 = AXIS2_PLACEMENT_3D ( 'NONE', #35017, #29496, #2948 ) ;
#33554 = CARTESIAN_POINT ( 'NONE',  ( -145.0000000000000568, -78.33668825982573480, -65.00000000000000000 ) ) ;
#33555 = DIRECTION ( 'NONE',  ( 0.000000000000000000, 0.000000000000000000, -1.000000000000000000 ) ) ;
#33556 = DIRECTION ( 'NONE',  ( -0.9985334138511239299, -0.05413890858541787338, -9.945156166269473284E-18 ) ) ;
#33557 = ORIENTED_EDGE ( 'NONE', *, *, #10687, .T. ) ;
#33558 = ORIENTED_EDGE ( 'NONE', *, *, #25662, .T. ) ;
#33559 = FACE_OUTER_BOUND ( 'NONE', #16471, .T. ) ;
#33560 = FACE_OUTER_BOUND ( 'NONE', #23460, .T. ) ;
#33561 = LINE ( 'NONE', #30900, #24274 ) ;
#33562 = CARTESIAN_POINT ( 'NONE',  ( 12.00000000000001066, 134.9999999999999432, -154.9999999999999716 ) ) ;
#33563 = DIRECTION ( 'NONE',  ( 1.000000000000000000, 0.000000000000000000, 0.000000000000000000 ) ) ;
#33564 = CARTESIAN_POINT ( 'NONE',  ( 1.155000000000000027, 1.414467053015192657E-16, 0.000000000000000000 ) ) ;
#33565 = AXIS2_PLACEMENT_3D ( 'NONE', #25592, #22763, #17787 ) ;
#33566 = CARTESIAN_POINT ( 'NONE',  ( 2.789999999999999147, 28.06759692514767934, 11.78059558880223712 ) ) ;
#33567 = ORIENTED_EDGE ( 'NONE', *, *, #5368, .T. ) ;
#33568 = EDGE_CURVE ( 'NONE', #20411, #13771, #19544, .T. ) ;
#33569 = LINE ( 'NONE', #488, #12313 ) ;
#33570 = CARTESIAN_POINT ( 'NONE',  ( 19.99999999999998934, -115.0000000000000000, 162.9999999999999716 ) ) ;
#33571 = PLANE ( 'NONE',  #21750 ) ;
#33572 = ORIENTED_EDGE ( 'NONE', *, *, #1405, .T. ) ;
#33573 = CARTESIAN_POINT ( 'NONE',  ( -365.0000000000000000, 118.9999999999999716, 126.0000000000000000 ) ) ;
#33574 = ORIENTED_EDGE ( 'NONE', *, *, #30444, .F. ) ;
#33575 = AXIS2_PLACEMENT_3D ( 'NONE', #4874, #20574, #15772 ) ;
#33576 =( NAMED_UNIT ( * ) PLANE_ANGLE_UNIT ( ) SI_UNIT ( $, .RADIAN. ) );
#33577 = LINE ( 'NONE', #14563, #1259 ) ;
#33578 = EDGE_CURVE ( 'NONE', #33515, #16809, #12249, .T. ) ;
#33579 = CIRCLE ( 'NONE', #32983, 7.999999999999986677 ) ;
#33580 = EDGE_CURVE ( 'NONE', #2324, #28031, #6162, .T. ) ;
#33581 = EDGE_CURVE ( 'NONE', #19630, #21502, #27886, .T. ) ;
#33582 = VERTEX_POINT ( 'NONE', #31099 ) ;
#33583 = DIRECTION ( 'NONE',  ( 1.000000000000000000, 0.000000000000000000, 0.000000000000000000 ) ) ;
#33584 = CARTESIAN_POINT ( 'NONE',  ( -363.0000000000000000, 134.9999999999999716, 114.0000000000000000 ) ) ;
#33585 = CARTESIAN_POINT ( 'NONE',  ( -110.1150203881707910, 0.000000000000000000, 60.00000000000000000 ) ) ;
#33586 = MANIFOLD_SOLID_BREP ( 'Keyway', #26452 ) ;
#33587 = ORIENTED_EDGE ( 'NONE', *, *, #23864, .T. ) ;
#33588 = VECTOR ( 'NONE', #29236, 1000.000000000000000 ) ;
#33589 = DIRECTION ( 'NONE',  ( -7.893605728314051750E-14, 1.618803117314786530E-15, 1.000000000000000000 ) ) ;
#33590 = VECTOR ( 'NONE', #20589, 1000.000000000000000 ) ;
#33591 = PRESENTATION_LAYER_ASSIGNMENT (  '', '', ( #5727 ) ) ;
#33592 = CYLINDRICAL_SURFACE ( 'NONE', #2250, 2.033421858999710619 ) ;
#33593 = ORIENTED_EDGE ( 'NONE', *, *, #26937, .T. ) ;
#33594 = CARTESIAN_POINT ( 'NONE',  ( -25.63124651156763179, 20.05601094782693394, 68.31122994652405112 ) ) ;
#33595 = CARTESIAN_POINT ( 'NONE',  ( -143.0000000000000568, -78.33668825982579165, -75.00000000000001421 ) ) ;
#33596 = CARTESIAN_POINT ( 'NONE',  ( 1.649999999999999911, 2.020667218593132262E-16, 3.180000000000000160 ) ) ;
#33597 = CARTESIAN_POINT ( 'NONE',  ( -110.1150203881707910, 0.000000000000000000, -57.49999999999999289 ) ) ;
#33598 = ITEM_DEFINED_TRANSFORMATION ( 'NONE', 'NONE', #6437,  #28566 ) ;
#33599 = ORIENTED_EDGE ( 'NONE', *, *, #3950, .T. ) ;
#33600 = ORIENTED_EDGE ( 'NONE', *, *, #20590, .T. ) ;
#33601 = VERTEX_POINT ( 'NONE', #844 ) ;
#33602 = CIRCLE ( 'NONE', #22254, 7.999999999999986677 ) ;
#33603 = CARTESIAN_POINT ( 'NONE',  ( 17.88561705399011714, -27.19023860642122514, 68.31122994652405112 ) ) ;
#33605 = VECTOR ( 'NONE', #1688, 1000.000000000000000 ) ;
#33604 = CARTESIAN_POINT ( 'NONE',  ( -499.9999999999999432, -113.0000000000000000, -162.9999999999999716 ) ) ;
#33606 = DIRECTION ( 'NONE',  ( 0.000000000000000000, 1.836970198721029441E-16, -1.000000000000000000 ) ) ;
#33607 = CARTESIAN_POINT ( 'NONE',  ( 2.789999999999999147, 11.30192140231231868, 28.29696565125074414 ) ) ;
#33608 = VERTEX_POINT ( 'NONE', #7213 ) ;
#33609 = DIRECTION ( 'NONE',  ( 1.000000000000000000, 0.000000000000000000, -1.848892746611746966E-32 ) ) ;
#33610 = LINE ( 'NONE', #395, #16995 ) ;
#33611 = ORIENTED_EDGE ( 'NONE', *, *, #12621, .F. ) ;
#33612 = PRODUCT_DEFINITION_SHAPE ( 'NONE', 'NONE',  #35134 ) ;
#33613 = CARTESIAN_POINT ( 'NONE',  ( -12.00000000000001066, 124.9999999999999716, 187.0000000000000000 ) ) ;
#33614 = LINE ( 'NONE', #33442, #8051 ) ;
#33615 = EDGE_LOOP ( 'NONE', ( #21621, #28146, #3394, #17808 ) ) ;
#33616 = ORIENTED_EDGE ( 'NONE', *, *, #31936, .T. ) ;
#33617 = DIRECTION ( 'NONE',  ( 1.000000000000000000, 0.000000000000000000, -1.848892746611746966E-32 ) ) ;
#33618 = AXIS2_PLACEMENT_3D ( 'NONE', #20843, #9987, #2152 ) ;
#33619 = EDGE_CURVE ( 'NONE', #8787, #22671, #11443, .T. ) ;
#33621 = CIRCLE ( 'NONE', #22830, 2.000000000000001776 ) ;
#33620 = DIRECTION ( 'NONE',  ( 0.000000000000000000, 1.000000000000000000, -3.374343856708137958E-53 ) ) ;
#33622 = ORIENTED_EDGE ( 'NONE', *, *, #34314, .F. ) ;
#33623=STYLED_ITEM('',(#35254),#22535);
#33624 = FACE_OUTER_BOUND ( 'NONE', #28490, .T. ) ;
#33625 = DIRECTION ( 'NONE',  ( 1.000000000000000000, -0.000000000000000000, 0.000000000000000000 ) ) ;
#33626 = EDGE_CURVE ( 'NONE', #5671, #5820, #25746, .T. ) ;
#33627 = LINE ( 'NONE', #17101, #17286 ) ;
#33628 = EDGE_CURVE ( 'NONE', #30776, #12415, #23426, .T. ) ;
#33629 = CARTESIAN_POINT ( 'NONE',  ( -109.3380992783527432, -2.715097909449874614, 12.20238416997438158 ) ) ;
#33630 = LINE ( 'NONE', #20120, #34978 ) ;
#33632 = EDGE_CURVE ( 'NONE', #22581, #27476, #18278, .T. ) ;
#33631 = DIRECTION ( 'NONE',  ( -0.000000000000000000, 1.836970198721029934E-16, -1.000000000000000000 ) ) ;
#33633 = EDGE_LOOP ( 'NONE', ( #1002, #20836, #7350, #4859 ) ) ;
#33634 = EDGE_LOOP ( 'NONE', ( #30625, #24570, #11005, #29373, #11605, #1442, #17458, #424 ) ) ;
#33635 = DIRECTION ( 'NONE',  ( -7.893605728314050488E-14, 1.618803117314786135E-15, 0.9999999999999998890 ) ) ;
#33636 = ORIENTED_EDGE ( 'NONE', *, *, #480, .F. ) ;
#33637 = ADVANCED_FACE ( 'NONE', ( #20419 ), #4577, .T. ) ;
#33638 = VECTOR ( 'NONE', #14956, 1000.000000000000000 ) ;
#33639 = CARTESIAN_POINT ( 'NONE',  ( -10.00000000000000000, 0.000000000000000000, 0.000000000000000000 ) ) ;
#33640 = DIRECTION ( 'NONE',  ( -1.000000000000000000, -0.000000000000000000, -0.000000000000000000 ) ) ;
#33641 = AXIS2_PLACEMENT_3D ( 'NONE', #20079, #3156, #9394 ) ;
#33642 = ORIENTED_EDGE ( 'NONE', *, *, #4000, .F. ) ;
#33643 = AXIS2_PLACEMENT_3D ( 'NONE', #20964, #31465, #28972 ) ;
#33644 = AXIS2_PLACEMENT_3D ( 'NONE', #5503, #21890, #16401 ) ;
#33646 = MANIFOLD_SOLID_BREP ( 'BearingFace', #24161 ) ;
#33645 = DIRECTION ( 'NONE',  ( 0.000000000000000000, 0.000000000000000000, -1.000000000000000000 ) ) ;
#33647 = CARTESIAN_POINT ( 'NONE',  ( -103.6592623599142087, -4.947629808455840994, -11.47938275244241169 ) ) ;
#33648 = ITEM_DEFINED_TRANSFORMATION ( 'NONE', 'NONE', #25787,  #28566 ) ;
#33650 = DIRECTION ( 'NONE',  ( 1.000000000000000000, 0.000000000000000000, 0.000000000000000000 ) ) ;
#33649 = DIRECTION ( 'NONE',  ( 0.000000000000000000, -1.000000000000000000, 6.123233995736766036E-17 ) ) ;
#33651 = ORIENTED_EDGE ( 'NONE', *, *, #435, .F. ) ;
#33652 = EDGE_LOOP ( 'NONE', ( #15813, #23872, #4702, #33616, #5144 ) ) ;
#33653 = CARTESIAN_POINT ( 'NONE',  ( -27.76765758629847980, -16.97532223688790864, -36.68877005347593467 ) ) ;
#33654 = DIRECTION ( 'NONE',  ( -1.000000000000000000, -0.000000000000000000, -0.000000000000000000 ) ) ;
#33655 = DIRECTION ( 'NONE',  ( 0.000000000000000000, 1.374038396813311798E-15, -1.000000000000000000 ) ) ;
#33656 = ORIENTED_EDGE ( 'NONE', *, *, #19293, .T. ) ;
#33657 = CARTESIAN_POINT ( 'NONE',  ( 0.1859802790892826907, -22.69026646801045999, -22.96218055026821858 ) ) ;
#33658 = CARTESIAN_POINT ( 'NONE',  ( 1.749999999999999778, -10.89151784028311809, 32.64600270996213283 ) ) ;
#33659 = PRODUCT_DEFINITION_SHAPE ( 'NONE', 'NONE',  #16007 ) ;
#33660 = VERTEX_POINT ( 'NONE', #17940 ) ;
#33661 = DIRECTION ( 'NONE',  ( 0.000000000000000000, -1.000000000000000000, 0.000000000000000000 ) ) ;
#33662 = DIRECTION ( 'NONE',  ( -1.000000000000000000, 0.000000000000000000, 1.848892746611746966E-32 ) ) ;
#33663 = DIRECTION ( 'NONE',  ( -1.000000000000000000, 0.000000000000000000, -5.546364386991661285E-52 ) ) ;
#33666 = CARTESIAN_POINT ( 'NONE',  ( -15.99999999999998579, -56.99999999999997868, -175.0000000000000000 ) ) ;
#33665 = DIRECTION ( 'NONE',  ( -1.000000000000000000, 0.000000000000000000, -0.000000000000000000 ) ) ;
#33664 = VECTOR ( 'NONE', #4671, 1000.000000000000000 ) ;
#33667 = CIRCLE ( 'NONE', #11495, 22.50000000000000355 ) ;
#33668 = AXIS2_PLACEMENT_3D ( 'NONE', #30708, #8993, #22526 ) ;
#33669 = CARTESIAN_POINT ( 'NONE',  ( 5.021133111224162171, -21.54630831098063481, -87.50000000000000000 ) ) ;
#33670 = CARTESIAN_POINT ( 'NONE',  ( -34.66645501699844090, -15.21971901163153440, -36.68877005347593467 ) ) ;
#33671 = EDGE_LOOP ( 'NONE', ( #16382, #3478, #15693, #28002 ) ) ;
#33672 = DIRECTION ( 'NONE',  ( 0.000000000000000000, -1.000000000000000000, 0.000000000000000000 ) ) ;
#33673 = EDGE_CURVE ( 'NONE', #7946, #6878, #34639, .T. ) ;
#33674 = EDGE_CURVE ( 'NONE', #14836, #5864, #21093, .T. ) ;
#33675 = ORIENTED_EDGE ( 'NONE', *, *, #2472, .F. ) ;
#33676 = ADVANCED_FACE ( 'NONE', ( #20935 ), #23095, .F. ) ;
#33677 = EDGE_CURVE ( 'NONE', #181, #4287, #16570, .T. ) ;
#33678 = ORIENTED_EDGE ( 'NONE', *, *, #6124, .T. ) ;
#33679 = VERTEX_POINT ( 'NONE', #21105 ) ;
#33680 = CARTESIAN_POINT ( 'NONE',  ( 10.96230482721425403, -16.64466345897533017, -77.50000000000000000 ) ) ;
#33681 = ORIENTED_EDGE ( 'NONE', *, *, #11972, .F. ) ;
#33682 = ORIENTED_EDGE ( 'NONE', *, *, #6264, .T. ) ;
#33683 = B_SPLINE_CURVE_WITH_KNOTS ( 'NONE', 3,
 ( #28189, #3791, #28878, #16073 ),
 .UNSPECIFIED., .F., .F.,
 ( 4, 4 ),
 ( 1.976296719774577317E-07, 0.0006879333227023364796 ),
 .UNSPECIFIED. ) ;
#33684 = CARTESIAN_POINT ( 'NONE',  ( 22.10765473302597073, -12.47301499840863848, -87.50000000000000000 ) ) ;
#33685 = ADVANCED_FACE ( 'NONE', ( #15084 ), #4368, .F. ) ;
#33686 = AXIS2_PLACEMENT_3D ( 'NONE', #16940, #3381, #11233 ) ;
#33687 = EDGE_LOOP ( 'NONE', ( #23591, #34445, #1552, #26329 ) ) ;
#33688 = LINE ( 'NONE', #23196, #10120 ) ;
#33689 = AXIS2_PLACEMENT_3D ( 'NONE', #8889, #6201, #3367 ) ;
#33690 = DIRECTION ( 'NONE',  ( -0.000000000000000000, -1.000000000000000000, -0.000000000000000000 ) ) ;
#33691 = VERTEX_POINT ( 'NONE', #1713 ) ;
#33692 = AXIS2_PLACEMENT_3D ( 'NONE', #32266, #34775, #10570 ) ;
#33693 = VERTEX_POINT ( 'NONE', #2065 ) ;
#33694 = DIRECTION ( 'NONE',  ( 0.000000000000000000, 1.000000000000000000, -3.374343856708137958E-53 ) ) ;
#33695 = PLANE ( 'NONE',  #20939 ) ;
#33696 = PLANE ( 'NONE',  #1658 ) ;
#33697 = CARTESIAN_POINT ( 'NONE',  ( -20.63749999999999574, 0.000000000000000000, -14.77500000000000036 ) ) ;
#33698 = DIRECTION ( 'NONE',  ( -1.000000000000000000, 0.000000000000000000, 0.000000000000000000 ) ) ;
#33699 = ORIENTED_EDGE ( 'NONE', *, *, #30868, .T. ) ;
#33700 = ADVANCED_FACE ( 'NONE', ( #12580 ), #7565, .F. ) ;
#33701 = FACE_BOUND ( 'NONE', #34732, .T. ) ;
#33702 = DIRECTION ( 'NONE',  ( -0.000000000000000000, -1.836970198721029688E-16, 1.000000000000000000 ) ) ;
#33703 = EDGE_CURVE ( 'NONE', #21709, #10179, #32305, .T. ) ;
#33704 = DIRECTION ( 'NONE',  ( 0.000000000000000000, 1.000000000000000000, 5.053935297177146739E-49 ) ) ;
#33705 = ORIENTED_EDGE ( 'NONE', *, *, #34025, .T. ) ;
#33706 = MANIFOLD_SOLID_BREP ( 'OuterRace', #30423 ) ;
#33707 = DIRECTION ( 'NONE',  ( 0.000000000000000000, 1.836970198721029441E-16, -1.000000000000000000 ) ) ;
#33708 = DIRECTION ( 'NONE',  ( 0.000000000000000000, 0.000000000000000000, 1.000000000000000000 ) ) ;
#33709 = FACE_OUTER_BOUND ( 'NONE', #21787, .T. ) ;
#33710 = CARTESIAN_POINT ( 'NONE',  ( 0.7561992196122224730, 22.02446183774635102, 25.79073883748091589 ) ) ;
#33712 = CYLINDRICAL_SURFACE ( 'NONE', #27572, 12.50000000000000000 ) ;
#33711 = LINE ( 'NONE', #10027, #19027 ) ;
#33713 = VECTOR ( 'NONE', #13619, 1000.000000000000000 ) ;
#33714 = DIRECTION ( 'NONE',  ( 0.000000000000000000, 1.836970198721029441E-16, -1.000000000000000000 ) ) ;
#33715 = ORIENTED_EDGE ( 'NONE', *, *, #761, .T. ) ;
#33716 = CARTESIAN_POINT ( 'NONE',  ( 0.000000000000000000, 0.000000000000000000, 3.930000000000000160 ) ) ;
#33718 = DIRECTION ( 'NONE',  ( 1.000000000000000000, 0.000000000000000000, 0.000000000000000000 ) ) ;
#33717 = CARTESIAN_POINT ( 'NONE',  ( 2.765921099433442443, 28.29688452313417812, -12.88099432405573630 ) ) ;
#33719 = AXIS2_PLACEMENT_3D ( 'NONE', #18519, #4950, #20988 ) ;
#33721 = EDGE_LOOP ( 'NONE', ( #18780, #25380, #34491, #30419, #30514, #573, #10842, #30766, #19587, #31055, #5865 ) ) ;
#33720 = VECTOR ( 'NONE', #11178, 1000.000000000000000 ) ;
#33722 = EDGE_CURVE ( 'NONE', #24969, #8699, #15792, .T. ) ;
#33723 = EDGE_CURVE ( 'NONE', #28881, #17261, #16485, .T. ) ;
#33724 = AXIS2_PLACEMENT_3D ( 'NONE', #16130, #32469, #5415 ) ;
#33725 = CARTESIAN_POINT ( 'NONE',  ( 2.783128933130080362, 30.78681169157792041, 2.258271426746184751 ) ) ;
#33726 = ORIENTED_EDGE ( 'NONE', *, *, #33758, .F. ) ;
#33727 = EDGE_CURVE ( 'NONE', #9979, #9877, #27141, .T. ) ;
#33728 = ORIENTED_EDGE ( 'NONE', *, *, #5639, .F. ) ;
#33729 = CARTESIAN_POINT ( 'NONE',  ( 99.80968765692681188, -2.454113965193227997, -7.089506392665936296 ) ) ;
#33730 = ORIENTED_EDGE ( 'NONE', *, *, #19986, .F. ) ;
#33731 = ORIENTED_EDGE ( 'NONE', *, *, #15174, .F. ) ;
#33732 = DIRECTION ( 'NONE',  ( 1.000000000000000000, 0.000000000000000000, 0.000000000000000000 ) ) ;
#33733 = DIRECTION ( 'NONE',  ( 0.000000000000000000, -2.465190328815661892E-32, -1.000000000000000000 ) ) ;
#33734 = VECTOR ( 'NONE', #14403, 1000.000000000000000 ) ;
#33735 = CYLINDRICAL_SURFACE ( 'NONE', #34417, 12.00000000000001066 ) ;
#33736 = LINE ( 'NONE', #30720, #21076 ) ;
#33737 = ORIENTED_EDGE ( 'NONE', *, *, #22834, .T. ) ;
#33738 = ORIENTED_EDGE ( 'NONE', *, *, #26354, .T. ) ;
#33739 = CARTESIAN_POINT ( 'NONE',  ( -20.00000000000004619, -137.0000000000000000, -159.0000000000000000 ) ) ;
#33740 = DIRECTION ( 'NONE',  ( 1.232595164407830946E-32, 0.000000000000000000, 1.000000000000000000 ) ) ;
#33741 = LINE ( 'NONE', #31421, #25449 ) ;
#33742 = EDGE_CURVE ( 'NONE', #31908, #17794, #9711, .T. ) ;
#33743 = CARTESIAN_POINT ( 'NONE',  ( -20.00000000000001776, -109.0000000000000142, 187.0000000000000000 ) ) ;
#33744 = DIRECTION ( 'NONE',  ( 0.000000000000000000, -1.131431318426415506E-52, -1.000000000000000000 ) ) ;
#33745 = EDGE_CURVE ( 'NONE', #5785, #939, #1341, .T. ) ;
#33746 = AXIS2_PLACEMENT_3D ( 'NONE', #20772, #34292, #20598 ) ;
#33747 = EDGE_CURVE ( 'NONE', #14902, #13888, #29641, .T. ) ;
#33748 = FACE_OUTER_BOUND ( 'NONE', #4022, .T. ) ;
#33749 = AXIS2_PLACEMENT_3D ( 'NONE', #29473, #5066, #18454 ) ;
#33750 = AXIS2_PLACEMENT_3D ( 'NONE', #14650, #25650, #5895 ) ;
#33751 = DIRECTION ( 'NONE',  ( 1.000000000000000000, 0.000000000000000000, 0.000000000000000000 ) ) ;
#33752 = ORIENTED_EDGE ( 'NONE', *, *, #20387, .F. ) ;
#33753 = CARTESIAN_POINT ( 'NONE',  ( 0.02407890056655651728, -15.32140196853772984, 27.05343472112986092 ) ) ;
#33754 = EDGE_CURVE ( 'NONE', #7236, #4465, #26618, .T. ) ;
#33755 = CARTESIAN_POINT ( 'NONE',  ( -27.27957549904816048, -33.75938860598994040, 33.83906026525051658 ) ) ;
#33756 = LINE ( 'NONE', #33933, #31406 ) ;
#33757 = VERTEX_POINT ( 'NONE', #5238 ) ;
#33758 = EDGE_CURVE ( 'NONE', #5512, #6878, #34881, .T. ) ;
#33759 =( REPRESENTATION_RELATIONSHIP ('NONE','NONE', #23037, #28231 ) REPRESENTATION_RELATIONSHIP_WITH_TRANSFORMATION ( #32970 )SHAPE_REPRESENTATION_RELATIONSHIP( ) );
#33760 = ADVANCED_FACE ( 'NONE', ( #29995 ), #5069, .F. ) ;
#33761 = CARTESIAN_POINT ( 'NONE',  ( -442.0000000000000000, -125.0000000000000000, -101.9999999999999858 ) ) ;
#33762 = ORIENTED_EDGE ( 'NONE', *, *, #13717, .T. ) ;
#33763 = CARTESIAN_POINT ( 'NONE',  ( -365.0000000000000000, -133.0000000000000000, 126.0000000000000000 ) ) ;
#33764 = FACE_OUTER_BOUND ( 'NONE', #29397, .T. ) ;
#33765 = CIRCLE ( 'NONE', #17326, 7.500000000000000000 ) ;
#33766 = EDGE_CURVE ( 'NONE', #10045, #30850, #34149, .T. ) ;
#33767 = ORIENTED_EDGE ( 'NONE', *, *, #27189, .T. ) ;
#33768 = DIRECTION ( 'NONE',  ( -1.000000000000000000, -0.000000000000000000, -0.000000000000000000 ) ) ;
#33769 = CARTESIAN_POINT ( 'NONE',  ( -445.9999999999999432, -112.9999999999999858, -155.0000000000000000 ) ) ;
#33770 = DIRECTION ( 'NONE',  ( 1.000000000000000000, 0.000000000000000000, 0.000000000000000000 ) ) ;
#33771 = ORIENTED_EDGE ( 'NONE', *, *, #21472, .F. ) ;
#33772 = FACE_OUTER_BOUND ( 'NONE', #2714, .T. ) ;
#33773 = AXIS2_PLACEMENT_3D ( 'NONE', #15701, #34193, #31521 ) ;
#33774 = CARTESIAN_POINT ( 'NONE',  ( 794.0359714656788128, 990.7481904691475165, 1753.598338701303419 ) ) ;
#33775 = VECTOR ( 'NONE', #6654, 1000.000000000000000 ) ;
#33776 = DIRECTION ( 'NONE',  ( -0.000000000000000000, -0.000000000000000000, -1.000000000000000000 ) ) ;
#33777 = ORIENTED_EDGE ( 'NONE', *, *, #14777, .F. ) ;
#33778 = CARTESIAN_POINT ( 'NONE',  ( -145.0000000000000568, 87.50000000000000000, 65.00000000000000000 ) ) ;
#33779 = AXIS2_PLACEMENT_3D ( 'NONE', #15850, #24350, #34518 ) ;
#33780 = LINE ( 'NONE', #23280, #20952 ) ;
#33781 = DIRECTION ( 'NONE',  ( 0.9868265225415260300, -0.1617819965527648174, 0.000000000000000000 ) ) ;
#33782 = CARTESIAN_POINT ( 'NONE',  ( 8.000000000000000000, 0.000000000000000000, 0.000000000000000000 ) ) ;
#33783 = ITEM_DEFINED_TRANSFORMATION ( 'NONE', 'NONE', #28612,  #28566 ) ;
#33784 = VERTEX_POINT ( 'NONE', #21801 ) ;
#33785 = ORIENTED_EDGE ( 'NONE', *, *, #17597, .T. ) ;
#33786 = ORIENTED_EDGE ( 'NONE', *, *, #7135, .T. ) ;
#33787 =( NAMED_UNIT ( * ) SI_UNIT ( $, .STERADIAN. ) SOLID_ANGLE_UNIT ( ) );
#33788 = FACE_OUTER_BOUND ( 'NONE', #32182, .T. ) ;
#33789 = EDGE_CURVE ( 'NONE', #18455, #12566, #2891, .T. ) ;
#33790 = EDGE_CURVE ( 'NONE', #26426, #34682, #11140, .T. ) ;
#33791 = AXIS2_PLACEMENT_3D ( 'NONE', #27816, #24608, #32802 ) ;
#33792 = CARTESIAN_POINT ( 'NONE',  ( 22.89764159710613001, 6.310691531022071921, -87.50000000000000000 ) ) ;
#33793 = CARTESIAN_POINT ( 'NONE',  ( -12.00000000000001066, -137.0000000000000000, 155.0000000000000000 ) ) ;
#33794 = CARTESIAN_POINT ( 'NONE',  ( -18.45373714011839539, 26.80790850550482673, -36.68877005347593467 ) ) ;
#33795 = DIRECTION ( 'NONE',  ( 0.1617819965527614312, -0.9868265225415265851, -0.000000000000000000 ) ) ;
#33796 = EDGE_LOOP ( 'NONE', ( #27641, #31539, #30317, #21388 ) ) ;
#33797 = VECTOR ( 'NONE', #6226, 1000.000000000000000 ) ;
#33798 = FACE_OUTER_BOUND ( 'NONE', #8330, .T. ) ;
#33799 = VERTEX_POINT ( 'NONE', #6530 ) ;
#33800 = ORIENTED_EDGE ( 'NONE', *, *, #15080, .F. ) ;
#33801 = DIRECTION ( 'NONE',  ( 0.000000000000000000, -1.310824597558155437E-49, -1.000000000000000000 ) ) ;
#33802 = VECTOR ( 'NONE', #28553, 1000.000000000000000 ) ;
#33803 = CIRCLE ( 'NONE', #20719, 1.649999999999999911 ) ;
#33804 = DIRECTION ( 'NONE',  ( -1.000000000000000000, -0.000000000000000000, -0.000000000000000000 ) ) ;
#33805 = ORIENTED_EDGE ( 'NONE', *, *, #27755, .F. ) ;
#33806 = CARTESIAN_POINT ( 'NONE',  ( -105.0000000000000000, 0.000000000000000000, 60.00000000000000000 ) ) ;
#33807 = CARTESIAN_POINT ( 'NONE',  ( -99.88497961182919482, 9.184690493976639608E-16, -7.500000000000000000 ) ) ;
#33808 = CARTESIAN_POINT ( 'NONE',  ( 15.99999999999998579, -137.0000000000000000, 174.9999999999999432 ) ) ;
#33809 = UNCERTAINTY_MEASURE_WITH_UNIT (LENGTH_MEASURE( 1.000000000000000082E-05 ), #16805, 'distance_accuracy_value', 'NONE');
#33810 = FACE_OUTER_BOUND ( 'NONE', #29409, .T. ) ;
#33811 = LINE ( 'NONE', #20635, #21142 ) ;
#33812 = ORIENTED_EDGE ( 'NONE', *, *, #10904, .T. ) ;
#33813 = AXIS2_PLACEMENT_3D ( 'NONE', #34080, #31071, #12388 ) ;
#33815 = ORIENTED_EDGE ( 'NONE', *, *, #27633, .F. ) ;
#33814 = B_SPLINE_CURVE_WITH_KNOTS ( 'NONE', 3,
 ( #16698, #14018, #27010, #8490, #2963, #131 ),
 .UNSPECIFIED., .F., .F.,
 ( 4, 2, 4 ),
 ( 2.699892344249078029E-07, 0.001873468359919019379, 0.003746666730603614125 ),
 .UNSPECIFIED. ) ;
#33816 = DIRECTION ( 'NONE',  ( -0.6673905642130606441, -0.7447078855493423077, -2.383035295615920728E-14 ) ) ;
#33817 = ORIENTED_EDGE ( 'NONE', *, *, #24368, .T. ) ;
#33818 = AXIS2_PLACEMENT_3D ( 'NONE', #26823, #26469, #2786 ) ;
#33819 = VECTOR ( 'NONE', #25407, 1000.000000000000000 ) ;
#33820 = CARTESIAN_POINT ( 'NONE',  ( 11.99999999999999645, -115.0000000000000000, 162.9999999999999716 ) ) ;
#33821 = AXIS2_PLACEMENT_3D ( 'NONE', #6427, #23171, #9471 ) ;
#33822 = PLANE ( 'NONE',  #7965 ) ;
#33823 = AXIS2_PLACEMENT_3D ( 'NONE', #18331, #23140, #4762 ) ;
#33824 = ORIENTED_EDGE ( 'NONE', *, *, #21412, .T. ) ;
#33825 = PLANE ( 'NONE',  #20779 ) ;
#33826 = CARTESIAN_POINT ( 'NONE',  ( -110.0804867582412214, -0.6815953102692046128, -12.48576125250277968 ) ) ;
#33827 = CLOSED_SHELL ( 'NONE', ( #16246, #7814, #24487, #14687, #7838, #21295, #30240, #6219, #24212, #1541 ) ) ;
#33828 = EDGE_CURVE ( 'NONE', #34039, #8710, #1710, .T. ) ;
#33829 = EDGE_CURVE ( 'NONE', #18536, #7560, #624, .T. ) ;
#33831 = CARTESIAN_POINT ( 'NONE',  ( 212.5000000000000000, 0.000000000000000000, 7.500000000000000000 ) ) ;
#33830 = CARTESIAN_POINT ( 'NONE',  ( 1.749999999999999778, 14.89726405156217126, 31.02351007835983054 ) ) ;
#33832 = EDGE_LOOP ( 'NONE', ( #4007, #27857, #27402, #4545 ) ) ;
#33833 = ORIENTED_EDGE ( 'NONE', *, *, #29162, .T. ) ;
#33834 = DIRECTION ( 'NONE',  ( 0.000000000000000000, 0.000000000000000000, 1.000000000000000000 ) ) ;
#33835 = ADVANCED_FACE ( 'NONE', ( #11485 ), #3810, .F. ) ;
#33836 = DIRECTION ( 'NONE',  ( 0.000000000000000000, 1.000000000000000000, -3.421138828918010427E-49 ) ) ;
#33837 = FACE_OUTER_BOUND ( 'NONE', #9525, .T. ) ;
#33838 = VERTEX_POINT ( 'NONE', #22873 ) ;
#33839 = VECTOR ( 'NONE', #25495, 1000.000000000000000 ) ;
#33840 = CARTESIAN_POINT ( 'NONE',  ( 0.1149164202474769469, 10.37169118567825699, 9.035703905990970952 ) ) ;
#33841 = FACE_OUTER_BOUND ( 'NONE', #30150, .T. ) ;
#33842 = AXIS2_PLACEMENT_3D ( 'NONE', #10068, #20923, #31770 ) ;
#33843 = EDGE_LOOP ( 'NONE', ( #8767, #8570 ) ) ;
#33844 = B_SPLINE_CURVE_WITH_KNOTS ( 'NONE', 3,
 ( #6036, #8896, #30966, #19770, #30617, #17105 ),
 .UNSPECIFIED., .F., .F.,
 ( 4, 2, 4 ),
 ( 2.446897702433135647E-07, 0.001873443032870421906, 0.003746641375970600780 ),
 .UNSPECIFIED. ) ;
#33845 = VECTOR ( 'NONE', #31252, 1000.000000000000000 ) ;
#33846 = DIRECTION ( 'NONE',  ( 1.000000000000000000, 0.000000000000000000, 0.000000000000000000 ) ) ;
#33847 = FACE_OUTER_BOUND ( 'NONE', #33155, .T. ) ;
#33848 = DIRECTION ( 'NONE',  ( 0.1063910735369155841, -0.9943243633099125844, -3.335902418025060287E-15 ) ) ;
#33849 = CARTESIAN_POINT ( 'NONE',  ( -355.0000000000000000, -131.0000000000000000, 128.0000000000000000 ) ) ;
#33851 = LINE ( 'NONE', #26353, #13407 ) ;
#33850 = CARTESIAN_POINT ( 'NONE',  ( -499.9999999999999432, -105.0000000000000142, -162.9999999999999716 ) ) ;
#33852 = VECTOR ( 'NONE', #20943, 1000.000000000000000 ) ;
#33853 = DIRECTION ( 'NONE',  ( 0.000000000000000000, 1.000000000000000000, 0.000000000000000000 ) ) ;
#33854 = CARTESIAN_POINT ( 'NONE',  ( -0.6763010051031078662, -1.505030548027689319, 3.180000000000000160 ) ) ;
#33855 = VERTEX_POINT ( 'NONE', #33188 ) ;
#33856 = CARTESIAN_POINT ( 'NONE',  ( 2.789999999999999147, -20.35927063852824048, 24.61013060777164796 ) ) ;
#33857 = CARTESIAN_POINT ( 'NONE',  ( -3.062871137271549632E-15, -12.35529564071043040, 5.600000207755297055 ) ) ;
#33858 = VECTOR ( 'NONE', #23689, 1000.000000000000000 ) ;
#33859 = ORIENTED_EDGE ( 'NONE', *, *, #26797, .T. ) ;
#33860 = VERTEX_POINT ( 'NONE', #9342 ) ;
#33861 = VECTOR ( 'NONE', #28748, 1000.000000000000000 ) ;
#33862 = FACE_OUTER_BOUND ( 'NONE', #16792, .T. ) ;
#33863 = ORIENTED_EDGE ( 'NONE', *, *, #1518, .T. ) ;
#33864 = VERTEX_POINT ( 'NONE', #30704 ) ;
#33865 = ORIENTED_EDGE ( 'NONE', *, *, #17296, .T. ) ;
#33866 = DIRECTION ( 'NONE',  ( 0.000000000000000000, 0.000000000000000000, 1.000000000000000000 ) ) ;
#33867 = VECTOR ( 'NONE', #20016, 1000.000000000000000 ) ;
#33868 = ADVANCED_FACE ( 'NONE', ( #25168 ), #17198, .F. ) ;
#33869 = CONTEXT_DEPENDENT_SHAPE_REPRESENTATION ( #125, #26346 ) ;
#33870 = ORIENTED_EDGE ( 'NONE', *, *, #10313, .F. ) ;
#33871 = CARTESIAN_POINT ( 'NONE',  ( -12.00000000000001066, -105.0000000000000142, 174.9999999999999432 ) ) ;
#33872 = CARTESIAN_POINT ( 'NONE',  ( 0.5288002543229157748, 26.55216317045622532, 20.24504431679649485 ) ) ;
#33873 = EDGE_LOOP ( 'NONE', ( #31511, #6980, #16249, #11734 ) ) ;
#33874 = VERTEX_POINT ( 'NONE', #33717 ) ;
#33875 = CARTESIAN_POINT ( 'NONE',  ( 0.5328044427876279521, -5.227541351193698560, 13.50000000000000178 ) ) ;
#33876 = DIRECTION ( 'NONE',  ( -1.000000000000000000, 0.000000000000000000, 0.000000000000000000 ) ) ;
#33877 = EDGE_CURVE ( 'NONE', #18216, #9649, #14703, .T. ) ;
#33878 = AXIS2_PLACEMENT_3D ( 'NONE', #542, #8716, #19413 ) ;
#33879 = EDGE_CURVE ( 'NONE', #24651, #6202, #12020, .T. ) ;
#33880 = PLANE ( 'NONE',  #27238 ) ;
#33881 = DIRECTION ( 'NONE',  ( 0.000000000000000000, 0.000000000000000000, -1.000000000000000000 ) ) ;
#33882 = FACE_OUTER_BOUND ( 'NONE', #8811, .T. ) ;
#33883 = ORIENTED_EDGE ( 'NONE', *, *, #14142, .T. ) ;
#33884 = LINE ( 'NONE', #18919, #10648 ) ;
#33885 = DIRECTION ( 'NONE',  ( -0.000000000000000000, -0.000000000000000000, 1.000000000000000000 ) ) ;
#33886 = ADVANCED_FACE ( 'NONE', ( #799 ), #19503, .F. ) ;
#33887 = ADVANCED_FACE ( 'NONE', ( #30529 ), #16661, .T. ) ;
#33888 = FACE_BOUND ( 'NONE', #2904, .T. ) ;
#33889 = VERTEX_POINT ( 'NONE', #22522 ) ;
#33890 = CARTESIAN_POINT ( 'NONE',  ( 1.749999999999999778, 28.00026196654299326, -20.00929742917092469 ) ) ;
#33891 = DIRECTION ( 'NONE',  ( -1.000000000000000000, 0.000000000000000000, 0.000000000000000000 ) ) ;
#33892 = CARTESIAN_POINT ( 'NONE',  ( 0.000000000000000000, -20.92506858792743785, -22.14933852381697932 ) ) ;
#33893 = EDGE_CURVE ( 'NONE', #1226, #28359, #27668, .T. ) ;
#33894 = CARTESIAN_POINT ( 'NONE',  ( 1.040000000000000702, 22.14447232807505728, 26.34405054495564968 ) ) ;
#33895 = DIRECTION ( 'NONE',  ( -1.000000000000000000, 0.000000000000000000, 0.000000000000000000 ) ) ;
#33896 = AXIS2_PLACEMENT_3D ( 'NONE', #5403, #10936, #15580 ) ;
#33897 = CARTESIAN_POINT ( 'NONE',  ( -410.0000000000000568, -137.0000000000000000, -155.0000000000000000 ) ) ;
#33898 = VERTEX_POINT ( 'NONE', #27495 ) ;
#33899 = CARTESIAN_POINT ( 'NONE',  ( 0.02407890056655695096, 20.99477179376858871, -22.93149026599722617 ) ) ;
#33901 = DIRECTION ( 'NONE',  ( -0.000000000000000000, 1.836970198721029934E-16, -1.000000000000000000 ) ) ;
#33900 = CARTESIAN_POINT ( 'NONE',  ( 10.17231796313407344, -3.615060903476079890, -77.50000000000000000 ) ) ;
#33902 = AXIS2_PLACEMENT_3D ( 'NONE', #22643, #9103, #20149 ) ;
#33903 = EDGE_LOOP ( 'NONE', ( #22664, #8517, #13456, #34380 ) ) ;
#33904 = DIRECTION ( 'NONE',  ( -1.000000000000000000, -0.000000000000000000, -0.000000000000000000 ) ) ;
#33905 = VECTOR ( 'NONE', #15926, 1000.000000000000000 ) ;
#33906 = EDGE_LOOP ( 'NONE', ( #26606, #18510, #16131, #24736, #11108, #15201, #8460, #27571, #10656 ) ) ;
#33907 = ORIENTED_EDGE ( 'NONE', *, *, #30540, .F. ) ;
#33908 = DIRECTION ( 'NONE',  ( 3.697785493223492838E-32, 1.934419779023891545E-16, -1.000000000000000000 ) ) ;
#33909 = ORIENTED_EDGE ( 'NONE', *, *, #27108, .F. ) ;
#33910 = ORIENTED_EDGE ( 'NONE', *, *, #29136, .F. ) ;
#33911 = CARTESIAN_POINT ( 'NONE',  ( 0.02407890056655825201, -17.95514392185434360, 25.38201125280350468 ) ) ;
#33912 = PRODUCT_DEFINITION_SHAPE ( 'NONE', 'NONE',  #35142 ) ;
#33913 = DIRECTION ( 'NONE',  ( 0.000000000000000000, -0.000000000000000000, -1.000000000000000000 ) ) ;
#33914 = AXIS2_PLACEMENT_3D ( 'NONE', #32636, #21221, #10360 ) ;
#33915 = CARTESIAN_POINT ( 'NONE',  ( 37.86520737902618805, 0.5181781365365152325, 49.43553178847298568 ) ) ;
#33916 = DIRECTION ( 'NONE',  ( 1.000000000000000000, -0.000000000000000000, 0.000000000000000000 ) ) ;
#33917 = VERTEX_POINT ( 'NONE', #27846 ) ;
#33918 = ORIENTED_EDGE ( 'NONE', *, *, #11590, .F. ) ;
#33919 = DIRECTION ( 'NONE',  ( -0.05413890858541785950, 0.9985334138511238189, -0.000000000000000000 ) ) ;
#33920 = PLANE ( 'NONE',  #451 ) ;
#33921 = CARTESIAN_POINT ( 'NONE',  ( -20.00000000000007461, -113.0000000000000000, -187.0000000000000000 ) ) ;
#33922 = EDGE_CURVE ( 'NONE', #7091, #35062, #33366, .T. ) ;
#33923 = DIRECTION ( 'NONE',  ( 0.000000000000000000, 1.000000000000000000, 1.224646799147353207E-16 ) ) ;
#33924 = DIRECTION ( 'NONE',  ( -0.000000000000000000, -1.836970198721029688E-16, 1.000000000000000000 ) ) ;
#33925 = ADVANCED_BREP_SHAPE_REPRESENTATION ( '', ( #33706, #28566 ), #17234 ) ;
#33926 = LINE ( 'NONE', #6507, #33845 ) ;
#33927 = EDGE_CURVE ( 'NONE', #26960, #20418, #28027, .T. ) ;
#33928 = EDGE_CURVE ( 'NONE', #32701, #20439, #19480, .T. ) ;
#33929 = FACE_OUTER_BOUND ( 'NONE', #29833, .T. ) ;
#33930 = EDGE_LOOP ( 'NONE', ( #24792, #34933, #18680, #2426 ) ) ;
#33931 = DIRECTION ( 'NONE',  ( 0.000000000000000000, 1.836970198721029934E-16, -1.000000000000000000 ) ) ;
#33932 = LINE ( 'NONE', #33755, #21696 ) ;
#33933 = CARTESIAN_POINT ( 'NONE',  ( -18.38714294329533416, -33.09555747561021377, 68.31122994652405112 ) ) ;
#33934 = VERTEX_POINT ( 'NONE', #11853 ) ;
#33935 = CARTESIAN_POINT ( 'NONE',  ( -414.0000000000000568, -137.0000000000000000, -155.0000000000000000 ) ) ;
#33936 = VERTEX_POINT ( 'NONE', #22702 ) ;
#33937 = CARTESIAN_POINT ( 'NONE',  ( -442.0000000000000000, 113.0000000000000000, -175.0000000000000000 ) ) ;
#33938 = CARTESIAN_POINT ( 'NONE',  ( -108.3843351873371574, 3.849558703864948583, 11.89498339909459723 ) ) ;
#33939 = EDGE_CURVE ( 'NONE', #23404, #32668, #6479, .T. ) ;
#33940 = VECTOR ( 'NONE', #16212, 1000.000000000000000 ) ;
#33941 = AXIS2_PLACEMENT_3D ( 'NONE', #22933, #6010, #1045 ) ;
#33942 = ORIENTED_EDGE ( 'NONE', *, *, #15224, .F. ) ;
#33943 = CARTESIAN_POINT ( 'NONE',  ( 19.99999999999996092, -145.0000000000000000, 162.9999999999999716 ) ) ;
#33944 = CARTESIAN_POINT ( 'NONE',  ( 0.000000000000000000, -30.41598411195412055, 1.821977758773545952 ) ) ;
#33945 = ADVANCED_FACE ( 'NONE', ( #24820 ), #454, .F. ) ;
#33946 = ORIENTED_EDGE ( 'NONE', *, *, #4536, .F. ) ;
#33947 = EDGE_CURVE ( 'NONE', #9326, #23878, #11527, .T. ) ;
#33948 = ADVANCED_FACE ( 'NONE', ( #23051 ), #23737, .F. ) ;
#33949 = DIRECTION ( 'NONE',  ( -0.08939666085780163807, -0.9959961029178152625, -8.486570951434709999E-15 ) ) ;
#33950 = CARTESIAN_POINT ( 'NONE',  ( 107.5556592954127666, -5.151199242560473124, 11.39037137834242586 ) ) ;
#33951 = ORIENTED_EDGE ( 'NONE', *, *, #6555, .T. ) ;
#33952 = DIRECTION ( 'NONE',  ( 0.000000000000000000, 0.000000000000000000, 1.000000000000000000 ) ) ;
#33953 = ADVANCED_FACE ( 'NONE', ( #17898 ), #34243, .F. ) ;
#33954 = PLANE ( 'NONE',  #31737 ) ;
#33955 = AXIS2_PLACEMENT_3D ( 'NONE', #8290, #30008, #19515 ) ;
#33956 = CARTESIAN_POINT ( 'NONE',  ( 0.5248942554772805247, -28.86920449294106916, 16.75648442687110773 ) ) ;
#33957 = CARTESIAN_POINT ( 'NONE',  ( -29.34345171400087793, 14.07715221144536777, -36.68877005347593467 ) ) ;
#33958 = ORIENTED_EDGE ( 'NONE', *, *, #29244, .T. ) ;
#33959 = ORIENTED_EDGE ( 'NONE', *, *, #15554, .F. ) ;
#33960 = ORIENTED_EDGE ( 'NONE', *, *, #30783, .T. ) ;
#33961 = CARTESIAN_POINT ( 'NONE',  ( 1.040000000000001146, 34.10861917999622506, -4.581348211831715034 ) ) ;
#33962 = LINE ( 'NONE', #31288, #4612 ) ;
#33963 = VECTOR ( 'NONE', #23885, 1000.000000000000000 ) ;
#33964 = CIRCLE ( 'NONE', #10649, 32.54542015209057126 ) ;
#33965 = CARTESIAN_POINT ( 'NONE',  ( -12.00000000000001066, 136.9999999999999716, -155.0000000000000000 ) ) ;
#33966 = CARTESIAN_POINT ( 'NONE',  ( -17.07420202168509604, 33.79163469797341435, 68.31122994652405112 ) ) ;
#33967 = ADVANCED_FACE ( 'NONE', ( #23560 ), #2022, .F. ) ;
#33969 = CARTESIAN_POINT ( 'NONE',  ( -414.0000000000000568, 124.9999999999999574, -187.0000000000000000 ) ) ;
#33968 = APPLICATION_CONTEXT ( 'automotive_design' ) ;
#33970 = CARTESIAN_POINT ( 'NONE',  ( 2.789940898827340199, -25.81863125502495038, -16.24881338200996694 ) ) ;
#33971 = ORIENTED_EDGE ( 'NONE', *, *, #34187, .T. ) ;
#33972 = CARTESIAN_POINT ( 'NONE',  ( 107.0424307436086337, 5.365524250098477665, 11.29014866489560376 ) ) ;
#33973 = ORIENTED_EDGE ( 'NONE', *, *, #1510, .F. ) ;
#33974 = DIRECTION ( 'NONE',  ( 0.000000000000000000, 0.000000000000000000, 1.000000000000000000 ) ) ;
#33975 = CARTESIAN_POINT ( 'NONE',  ( 0.000000000000000000, 0.000000000000000000, 0.000000000000000000 ) ) ;
#33976 = ORIENTED_EDGE ( 'NONE', *, *, #30508, .T. ) ;
#33977 = CARTESIAN_POINT ( 'NONE',  ( 2.604019725809434860, -24.34160354263056547, -21.20368514569445750 ) ) ;
#33978 = DIRECTION ( 'NONE',  ( 0.000000000000000000, 0.000000000000000000, -1.000000000000000000 ) ) ;
#33979 = AXIS2_PLACEMENT_3D ( 'NONE', #429, #29970, #14136 ) ;
#33980 = DIRECTION ( 'NONE',  ( 0.000000000000000000, 0.000000000000000000, 1.000000000000000000 ) ) ;
#33981 = B_SPLINE_CURVE_WITH_KNOTS ( 'NONE', 3,
 ( #17146, #755, #3239, #27798, #14114, #3411, #22473, #934 ),
 .UNSPECIFIED., .F., .F.,
 ( 4, 2, 2, 4 ),
 ( 0.02224295563652558400, 0.02421672923683100900, 0.02619050283713643401, 0.03013805003774728056 ),
 .UNSPECIFIED. ) ;
#33982 = CARTESIAN_POINT ( 'NONE',  ( -130.6469666100234406, 6.000000000000000000, -57.49999999999999289 ) ) ;
#33983 = CARTESIAN_POINT ( 'NONE',  ( -12.00000000000001066, 144.9999999999999716, -162.9999999999999432 ) ) ;
#33984 = EDGE_LOOP ( 'NONE', ( #1776, #23644, #28964, #20608 ) ) ;
#33985 = EDGE_CURVE ( 'NONE', #11239, #5234, #6828, .T. ) ;
#33986 = CIRCLE ( 'NONE', #16375, 3.999999999999976019 ) ;
#33987 = VECTOR ( 'NONE', #14066, 1000.000000000000000 ) ;
#33988 = EDGE_CURVE ( 'NONE', #7073, #10974, #33104, .T. ) ;
#33989 = EDGE_LOOP ( 'NONE', ( #27618, #3807, #23286, #6020 ) ) ;
#33990 = DIRECTION ( 'NONE',  ( -7.838314785662891421E-14, -7.144904269828988189E-15, 0.9999999999999998890 ) ) ;
#33991 = ORIENTED_EDGE ( 'NONE', *, *, #9581, .F. ) ;
#33992 = DIRECTION ( 'NONE',  ( 0.9476531711828025673, 0.3193015301359796165, 5.865473952658193889E-17 ) ) ;
#33993 = DIRECTION ( 'NONE',  ( -0.000000000000000000, -0.000000000000000000, -1.000000000000000000 ) ) ;
#33994 = CONTEXT_DEPENDENT_SHAPE_REPRESENTATION ( #21906, #14352 ) ;
#33995 = ORIENTED_EDGE ( 'NONE', *, *, #23625, .F. ) ;
#33996 = CARTESIAN_POINT ( 'NONE',  ( 2.789999999999999147, -13.59935610937951900, -26.37510281771846365 ) ) ;
#33997 = CARTESIAN_POINT ( 'NONE',  ( -1.030735741678193484, 1.713938105891546826, -0.7500000000000000000 ) ) ;
#33999 = CYLINDRICAL_SURFACE ( 'NONE', #30608, 2.525000000000001243 ) ;
#33998 = DIRECTION ( 'NONE',  ( -0.000000000000000000, -1.000000000000000000, -0.000000000000000000 ) ) ;
#34000 = VECTOR ( 'NONE', #16424, 1000.000000000000000 ) ;
#34001 = EDGE_LOOP ( 'NONE', ( #2062, #7601 ) ) ;
#34002 = ORIENTED_EDGE ( 'NONE', *, *, #4051, .F. ) ;
#34003 = DIRECTION ( 'NONE',  ( -0.000000000000000000, -1.000000000000000000, -0.000000000000000000 ) ) ;
#34004 = CARTESIAN_POINT ( 'NONE',  ( 19.99999999999998934, 75.55999999999990280, 172.9900000000000091 ) ) ;
#34005 = CARTESIAN_POINT ( 'NONE',  ( 32.54460952423469422, 0.2297037030477265540, 68.31122994652405112 ) ) ;
#34006 = EDGE_LOOP ( 'NONE', ( #8825, #31239, #14906, #12796 ) ) ;
#34007 = CIRCLE ( 'NONE', #18685, 2.000000000000001776 ) ;
#34008 = FACE_OUTER_BOUND ( 'NONE', #13007, .T. ) ;
#34009 =( REPRESENTATION_RELATIONSHIP ('NONE','NONE', #23037, #28231 ) REPRESENTATION_RELATIONSHIP_WITH_TRANSFORMATION ( #24226 )SHAPE_REPRESENTATION_RELATIONSHIP( ) );
#34010 = CIRCLE ( 'NONE', #10725, 34.41491905851385269 ) ;
#34011 = EDGE_LOOP ( 'NONE', ( #6436, #21460, #3712, #7920 ) ) ;
#34012 = EDGE_CURVE ( 'NONE', #23038, #26019, #15045, .T. ) ;
#34013 = FACE_OUTER_BOUND ( 'NONE', #20047, .T. ) ;
#34014 = LINE ( 'NONE', #34363, #13158 ) ;
#34015 = CARTESIAN_POINT ( 'NONE',  ( -20.00000000000001776, -141.0000000000000000, -162.9999999999999432 ) ) ;
#34016 = CIRCLE ( 'NONE', #19810, 1.999999999999999112 ) ;
#34018 = DIRECTION ( 'NONE',  ( 0.000000000000000000, 1.000000000000000000, 5.053935297177146739E-49 ) ) ;
#34017 = CARTESIAN_POINT ( 'NONE',  ( -12.00000000000001066, 104.9999999999999858, 154.9999999999999432 ) ) ;
#34019 = CARTESIAN_POINT ( 'NONE',  ( -449.9999999999999432, -137.0000000000000000, -175.0000000000000000 ) ) ;
#34020 = DIRECTION ( 'NONE',  ( 0.3193015301359796165, -0.9476531711828025673, 0.000000000000000000 ) ) ;
#34021 = CARTESIAN_POINT ( 'NONE',  ( 0.02407890056655695096, -8.112136323389137260, 30.01377904834206589 ) ) ;
#34022 = CARTESIAN_POINT ( 'NONE',  ( -19.99999999999998934, -137.0000000000000000, -155.0000000000000284 ) ) ;
#34023 = ADVANCED_FACE ( 'NONE', ( #6655 ), #3978, .F. ) ;
#34024 = AXIS2_PLACEMENT_3D ( 'NONE', #33613, #28103, #6379 ) ;
#34025 = EDGE_CURVE ( 'NONE', #31497, #6008, #28001, .T. ) ;
#34026 = EDGE_CURVE ( 'NONE', #750, #20418, #6952, .T. ) ;
#34027 = VECTOR ( 'NONE', #1531, 1000.000000000000000 ) ;
#34028 = ORIENTED_EDGE ( 'NONE', *, *, #28330, .F. ) ;
#34029 = ADVANCED_FACE ( 'NONE', ( #23222 ), #9684, .F. ) ;
#34030 = VERTEX_POINT ( 'NONE', #4497 ) ;
#34031 = ORIENTED_EDGE ( 'NONE', *, *, #14480, .T. ) ;
#34032 = AXIS2_PLACEMENT_3D ( 'NONE', #15849, #2813, #2987 ) ;
#34033 = DIRECTION ( 'NONE',  ( -1.000000000000000000, 0.000000000000000000, 0.000000000000000000 ) ) ;
#34034 = VERTEX_POINT ( 'NONE', #18238 ) ;
#34035 = ORIENTED_EDGE ( 'NONE', *, *, #34470, .T. ) ;
#34036 = EDGE_LOOP ( 'NONE', ( #1345, #30536, #16356, #26363, #6577, #1549, #16816, #672 ) ) ;
#34037 = DIRECTION ( 'NONE',  ( 1.000000000000000000, 3.040835319149746528E-31, 1.232595164407830946E-32 ) ) ;
#34038 = CIRCLE ( 'NONE', #27789, 32.54542015209056416 ) ;
#34039 = VERTEX_POINT ( 'NONE', #1671 ) ;
#34040 = CARTESIAN_POINT ( 'NONE',  ( -70.00000000000000000, 75.55999999999990280, -168.2400000000000091 ) ) ;
#34041 = CARTESIAN_POINT ( 'NONE',  ( -418.0000000000000000, 105.0000000000000142, -175.0000000000000000 ) ) ;
#34042 = VERTEX_POINT ( 'NONE', #23386 ) ;
#34043 = VERTEX_POINT ( 'NONE', #20723 ) ;
#34044 = CARTESIAN_POINT ( 'NONE',  ( 0.000000000000000000, 3.004629197474321612E-15, 13.50000000000000000 ) ) ;
#34045 = DIRECTION ( 'NONE',  ( 1.000000000000000000, 0.000000000000000000, 0.000000000000000000 ) ) ;
#34046 = DIRECTION ( 'NONE',  ( 1.000000000000000000, -0.000000000000000000, -0.000000000000000000 ) ) ;
#34047 = CARTESIAN_POINT ( 'NONE',  ( 5.021133111224473033, 8.235406450278430768, -87.50000000000000000 ) ) ;
#34048 = CARTESIAN_POINT ( 'NONE',  ( 2.765921099433442443, 20.99477179376858871, -22.93149026599722617 ) ) ;
#34049 = ORIENTED_EDGE ( 'NONE', *, *, #4793, .T. ) ;
#34050 = CARTESIAN_POINT ( 'NONE',  ( 119.9999999999998295, 0.000000000000000000, 10.00000000000000000 ) ) ;
#34051 = LINE ( 'NONE', #19845, #33284 ) ;
#34052 = TOROIDAL_SURFACE ( 'NONE', #1628, 30.47050528711512030, 8.000000000000000000 ) ;
#34053 = CARTESIAN_POINT ( 'NONE',  ( -19.99999999999998934, -112.9999999999999858, -155.0000000000000284 ) ) ;
#34054 = ORIENTED_EDGE ( 'NONE', *, *, #29605, .F. ) ;
#34055 = MANIFOLD_SOLID_BREP ( 'Boss-Extrude5', #10361 ) ;
#34056 = CARTESIAN_POINT ( 'NONE',  ( 0.02407890056655781832, -29.68817180695682723, 9.232883799364120847 ) ) ;
#34057 = DIRECTION ( 'NONE',  ( 1.000000000000000000, 0.000000000000000000, 0.000000000000000000 ) ) ;
#34058 = CARTESIAN_POINT ( 'NONE',  ( 10.17231796313409298, 4.274639749586561344, -77.50000000000000000 ) ) ;
#34059 = CARTESIAN_POINT ( 'NONE',  ( -5.210000000000000853, 0.000000000000000000, 0.000000000000000000 ) ) ;
#34061 = DIRECTION ( 'NONE',  ( 1.000000000000000000, 0.000000000000000000, 0.000000000000000000 ) ) ;
#34060 = DIRECTION ( 'NONE',  ( 0.000000000000000000, 0.000000000000000000, 1.000000000000000000 ) ) ;
#34062 = VECTOR ( 'NONE', #13999, 1000.000000000000000 ) ;
#34063 = ADVANCED_FACE ( 'NONE', ( #7706 ), #9855, .T. ) ;
#34064 = DIRECTION ( 'NONE',  ( 0.000000000000000000, -1.000000000000000000, 6.123233995736766036E-17 ) ) ;
#34065 = ORIENTED_EDGE ( 'NONE', *, *, #29687, .T. ) ;
#34066 = DIRECTION ( 'NONE',  ( 0.000000000000000000, 1.000000000000000000, 0.000000000000000000 ) ) ;
#34068 = DIRECTION ( 'NONE',  ( -1.000000000000000000, -0.000000000000000000, -0.000000000000000000 ) ) ;
#34067 = DIRECTION ( 'NONE',  ( 0.000000000000000000, 0.000000000000000000, -1.000000000000000000 ) ) ;
#34069 = EDGE_CURVE ( 'NONE', #1594, #17242, #15925, .T. ) ;
#34070 = AXIS2_PLACEMENT_3D ( 'NONE', #30517, #6282, #25158 ) ;
#34071 = VERTEX_POINT ( 'NONE', #19119 ) ;
#34072 = CARTESIAN_POINT ( 'NONE',  ( 0.000000000000000000, 2.281310696040539424E-14, -36.68877005347592757 ) ) ;
#34073 = ADVANCED_FACE ( 'NONE', ( #15745 ), #34954, .F. ) ;
#34074 = EDGE_LOOP ( 'NONE', ( #25972, #34143, #14489, #148 ) ) ;
#34075 = CIRCLE ( 'NONE', #1108, 4.306175033202026547 ) ;
#34076 = EDGE_LOOP ( 'NONE', ( #12028, #32996, #16971, #9594, #18076, #20798, #18351, #19870 ) ) ;
#34077 = FACE_OUTER_BOUND ( 'NONE', #21007, .T. ) ;
#34078 = EDGE_LOOP ( 'NONE', ( #1555, #19910, #19402, #14618 ) ) ;
#34079 = ORIENTED_EDGE ( 'NONE', *, *, #18613, .T. ) ;
#34080 = CARTESIAN_POINT ( 'NONE',  ( -12.00000000000001066, -32.99999999999997158, -154.9999999999999716 ) ) ;
#34081 = ADVANCED_FACE ( 'NONE', ( #26575 ), #10746, .T. ) ;
#34082 = ADVANCED_FACE ( 'NONE', ( #21424 ), #27447, .T. ) ;
#34083 = DIRECTION ( 'NONE',  ( 0.000000000000000000, -1.000000000000000000, 3.374343856708137958E-53 ) ) ;
#34084 = CARTESIAN_POINT ( 'NONE',  ( 11.99999999999999645, 136.9999999999999716, -155.0000000000000000 ) ) ;
#34085 = ORIENTED_EDGE ( 'NONE', *, *, #32845, .T. ) ;
#34086 = ORIENTED_EDGE ( 'NONE', *, *, #17795, .F. ) ;
#34087 = CARTESIAN_POINT ( 'NONE',  ( -30.91434716440808117, 10.17386417614053684, 68.31122994652405112 ) ) ;
#34088 = LINE ( 'NONE', #31083, #4385 ) ;
#34089 = CARTESIAN_POINT ( 'NONE',  ( -35.00000000000000000, 28.28427124746186649, 87.50000000000000000 ) ) ;
#34090 = DIRECTION ( 'NONE',  ( -1.000000000000000000, -0.000000000000000000, -0.000000000000000000 ) ) ;
#34091 = CARTESIAN_POINT ( 'NONE',  ( 2.789999999999999147, 0.000000000000000000, 0.000000000000000000 ) ) ;
#34092 = ORIENTED_EDGE ( 'NONE', *, *, #33723, .F. ) ;
#34093 = AXIS2_PLACEMENT_3D ( 'NONE', #31214, #28545, #26208 ) ;
#34094 = CARTESIAN_POINT ( 'NONE',  ( 36.86854689046325717, 8.645963718612076576, 49.43553178847298568 ) ) ;
#34095 = CARTESIAN_POINT ( 'NONE',  ( 0.5248942443853367168, -18.53613167721941579, -27.76008932203601276 ) ) ;
#34096 = ORIENTED_EDGE ( 'NONE', *, *, #15863, .T. ) ;
#34097 = CARTESIAN_POINT ( 'NONE',  ( 2.604019705202075041, -11.11575656128824185, -30.30758796111462772 ) ) ;
#34098 = LINE ( 'NONE', #29107, #1828 ) ;
#34099 = CYLINDRICAL_SURFACE ( 'NONE', #34252, 4.750000000000004441 ) ;
#34100 = ORIENTED_EDGE ( 'NONE', *, *, #29932, .F. ) ;
#34101 = CARTESIAN_POINT ( 'NONE',  ( -12.00000000000001243, 134.9999999999998863, 194.9999999999999716 ) ) ;
#34102 = EDGE_LOOP ( 'NONE', ( #8807, #14275, #23534, #27788 ) ) ;
#34104 = FILL_AREA_STYLE ('',( #6034 ) ) ;
#34103 = CARTESIAN_POINT ( 'NONE',  ( 0.000000000000000000, 15.58845726811990673, -2.400813222210650817E-15 ) ) ;
#34105 = CARTESIAN_POINT ( 'NONE',  ( -110.1150203881707910, 3.166944581793445397E-20, 12.50000000000000000 ) ) ;
#34106 = ORIENTED_EDGE ( 'NONE', *, *, #23745, .F. ) ;
#34107 = DIRECTION ( 'NONE',  ( 1.000000000000000000, 0.000000000000000000, -0.000000000000000000 ) ) ;
#34108 = LINE ( 'NONE', #33769, #13966 ) ;
#34109 = EDGE_CURVE ( 'NONE', #10000, #10965, #32087, .T. ) ;
#34110 = ORIENTED_EDGE ( 'NONE', *, *, #8060, .T. ) ;
#34111 = VECTOR ( 'NONE', #4997, 1000.000000000000227 ) ;
#34112 = EDGE_CURVE ( 'NONE', #7548, #22615, #12672, .T. ) ;
#34113 = EDGE_CURVE ( 'NONE', #16065, #22434, #5200, .T. ) ;
#34114 = CARTESIAN_POINT ( 'NONE',  ( 778.8220548561183705, 1132.936509181189194, 1753.598338701303192 ) ) ;
#34115 = ORIENTED_EDGE ( 'NONE', *, *, #19256, .T. ) ;
#34116 = DIRECTION ( 'NONE',  ( 1.000000000000000000, 0.000000000000000000, 0.000000000000000000 ) ) ;
#34117 = VERTEX_POINT ( 'NONE', #13068 ) ;
#34118 = CARTESIAN_POINT ( 'NONE',  ( -5.021133111224886036, 4.168562732279004202, -67.50000000000000000 ) ) ;
#34119 = CARTESIAN_POINT ( 'NONE',  ( -418.0000000000000000, -124.9999999999999716, 132.0000000000000000 ) ) ;
#34120 = CARTESIAN_POINT ( 'NONE',  ( -12.00000000000001066, -145.0000000000000000, 174.9999999999999432 ) ) ;
#34121 = DIRECTION ( 'NONE',  ( 0.000000000000000000, 1.131431318426415506E-52, 1.000000000000000000 ) ) ;
#34122 = ITEM_DEFINED_TRANSFORMATION ( 'NONE', 'NONE', #12723,  #28566 ) ;
#34123 = EDGE_LOOP ( 'NONE', ( #25674, #3602, #21581, #25107 ) ) ;
#34124 = VERTEX_POINT ( 'NONE', #29432 ) ;
#34125 = ORIENTED_EDGE ( 'NONE', *, *, #31936, .F. ) ;
#34126 = CARTESIAN_POINT ( 'NONE',  ( -349.0000000000000000, -135.0000000000000000, 128.0000000000000000 ) ) ;
#34127 = EDGE_CURVE ( 'NONE', #23603, #11199, #8104, .T. ) ;
#34128 = CARTESIAN_POINT ( 'NONE',  ( 28.23027531293552528, -10.15143121711728469, 20.00000000000000000 ) ) ;
#34129 = DIRECTION ( 'NONE',  ( 0.000000000000000000, 0.000000000000000000, -1.000000000000000000 ) ) ;
#34130 = LINE ( 'NONE', #1910, #30805 ) ;
#34131 = LINE ( 'NONE', #34669, #16912 ) ;
#34132 = CARTESIAN_POINT ( 'NONE',  ( -349.0000000000000000, -135.0000000000000000, 130.0000000000000000 ) ) ;
#34133 = ORIENTED_EDGE ( 'NONE', *, *, #26715, .F. ) ;
#34134 = CIRCLE ( 'NONE', #30221, 11.99999999999999645 ) ;
#34135 = EDGE_CURVE ( 'NONE', #26209, #1742, #7886, .T. ) ;
#34136 = CARTESIAN_POINT ( 'NONE',  ( 1.749999999999999778, -34.41385771548413430, 0.2702793785568976537 ) ) ;
#34137 = CIRCLE ( 'NONE', #32428, 30.47050528711512030 ) ;
#34139 = EDGE_CURVE ( 'NONE', #30924, #14545, #24593, .T. ) ;
#34138 = ORIENTED_EDGE ( 'NONE', *, *, #25635, .F. ) ;
#34140 = EDGE_CURVE ( 'NONE', #26810, #2032, #14384, .T. ) ;
#34141 = SHAPE_REPRESENTATION ( 'top shell', ( #28566 ), #5242 ) ;
#34142 = CARTESIAN_POINT ( 'NONE',  ( 2.606461937191911105, -24.33633102984369856, 21.19365992153269573 ) ) ;
#34143 = ORIENTED_EDGE ( 'NONE', *, *, #16383, .T. ) ;
#34144 = CARTESIAN_POINT ( 'NONE',  ( -500.0000000000000000, -109.0000000000000142, 187.0000000000000000 ) ) ;
#34145 = CARTESIAN_POINT ( 'NONE',  ( 0.07094831696795600440, -15.78353653323357619, -27.48438217453501409 ) ) ;
#34146 = CIRCLE ( 'NONE', #18819, 7.999999999999979572 ) ;
#34147 = AXIS2_PLACEMENT_3D ( 'NONE', #17943, #4370, #28944 ) ;
#34148 = PLANE ( 'NONE',  #1204 ) ;
#34149 = CIRCLE ( 'NONE', #8003, 14.77499999999999858 ) ;
#34150 = CARTESIAN_POINT ( 'NONE',  ( 0.000000000000000000, 6.992329373473909019E-15, 49.43553178847298568 ) ) ;
#34151 = DIRECTION ( 'NONE',  ( 1.232595164407830946E-32, 0.000000000000000000, 1.000000000000000000 ) ) ;
#34152 = VERTEX_POINT ( 'NONE', #16446 ) ;
#34153 = ORIENTED_EDGE ( 'NONE', *, *, #8706, .T. ) ;
#34154 = EDGE_CURVE ( 'NONE', #23829, #18049, #29774, .T. ) ;
#34155 = ADVANCED_FACE ( 'NONE', ( #13766 ), #2716, .F. ) ;
#34156 = CARTESIAN_POINT ( 'NONE',  ( 785.0459292684514594, 1074.768565606336551, 1753.598338701303419 ) ) ;
#34157 = CIRCLE ( 'NONE', #12579, 30.47050528711511674 ) ;
#34158 = ORIENTED_EDGE ( 'NONE', *, *, #25214, .F. ) ;
#34159 = EDGE_CURVE ( 'NONE', #26602, #25989, #2885, .T. ) ;
#34160 = CIRCLE ( 'NONE', #23911, 3.999999999999976019 ) ;
#34161 = CARTESIAN_POINT ( 'NONE',  ( -361.0000000000000000, -135.0000000000000000, 112.0000000000000000 ) ) ;
#34162 = DIRECTION ( 'NONE',  ( 0.000000000000000000, -1.000000000000000000, 0.000000000000000000 ) ) ;
#34163 = CONTEXT_DEPENDENT_SHAPE_REPRESENTATION ( #15113, #30821 ) ;
#34164 = ORIENTED_EDGE ( 'NONE', *, *, #4973, .F. ) ;
#34166 = MANIFOLD_SOLID_BREP ( 'Cut-Extrude3', #2404 ) ;
#34165 = LINE ( 'NONE', #5446, #21918 ) ;
#34167 = DIRECTION ( 'NONE',  ( -1.000000000000000000, 0.000000000000000000, 0.000000000000000000 ) ) ;
#34169 = DIRECTION ( 'NONE',  ( 0.000000000000000000, 0.000000000000000000, 1.000000000000000000 ) ) ;
#34168 = CARTESIAN_POINT ( 'NONE',  ( -13.53398258527560749, -35.36769364574539765, 68.31122994652405112 ) ) ;
#34171 = ORIENTED_EDGE ( 'NONE', *, *, #6897, .T. ) ;
#34170 = VECTOR ( 'NONE', #29376, 1000.000000000000000 ) ;
#34172 = ORIENTED_EDGE ( 'NONE', *, *, #22543, .T. ) ;
#34173 = FACE_OUTER_BOUND ( 'NONE', #7376, .T. ) ;
#34174 = AXIS2_PLACEMENT_3D ( 'NONE', #24206, #27586, #5859 ) ;
#34175 = CIRCLE ( 'NONE', #18848, 0.3000000000000016542 ) ;
#34176 = CIRCLE ( 'NONE', #18851, 2.000000000000001776 ) ;
#34177 = LINE ( 'NONE', #4440, #1129 ) ;
#34178 = PLANE ( 'NONE',  #29062 ) ;
#34179 = ORIENTED_EDGE ( 'NONE', *, *, #16410, .F. ) ;
#34180 = EDGE_CURVE ( 'NONE', #25584, #20352, #24583, .T. ) ;
#34181 = EDGE_CURVE ( 'NONE', #27122, #9925, #16641, .T. ) ;
#34182 = CARTESIAN_POINT ( 'NONE',  ( -442.0000000000000000, 113.0000000000000000, 154.9999999999999716 ) ) ;
#34183 = B_SPLINE_CURVE_WITH_KNOTS ( 'NONE', 3,
 ( #9145, #20370, #31217, #20202 ),
 .UNSPECIFIED., .F., .F.,
 ( 4, 4 ),
 ( 0.005298366463358190892, 0.005985234859393911803 ),
 .UNSPECIFIED. ) ;
#34184 = ORIENTED_EDGE ( 'NONE', *, *, #8237, .T. ) ;
#34185 = FACE_OUTER_BOUND ( 'NONE', #24644, .T. ) ;
#34186 = CARTESIAN_POINT ( 'NONE',  ( -10.00000000000000000, 3.520859547548641820E-15, 47.49999999999999289 ) ) ;
#34187 = EDGE_CURVE ( 'NONE', #8764, #21448, #10391, .T. ) ;
#34188 = VECTOR ( 'NONE', #30230, 1000.000000000000000 ) ;
#34189 = LINE ( 'NONE', #26526, #22958 ) ;
#34191 = DIRECTION ( 'NONE',  ( 0.000000000000000000, 1.000000000000000000, 0.000000000000000000 ) ) ;
#34190 = DIRECTION ( 'NONE',  ( 0.000000000000000000, -1.000000000000000000, 0.000000000000000000 ) ) ;
#34192 = EDGE_CURVE ( 'NONE', #2863, #10173, #24782, .T. ) ;
#34194 = ADVANCED_FACE ( 'NONE', ( #414 ), #33327, .T. ) ;
#34193 = DIRECTION ( 'NONE',  ( 0.000000000000000000, 1.000000000000000000, 5.053935297177146739E-49 ) ) ;
#34195 = DIRECTION ( 'NONE',  ( -0.000000000000000000, -0.000000000000000000, 1.000000000000000000 ) ) ;
#34196 = CARTESIAN_POINT ( 'NONE',  ( -15.99999999999998579, -32.99999999999997158, 154.9999999999999716 ) ) ;
#34197 = PRODUCT_DEFINITION_SHAPE ( 'NONE', 'NONE',  #35139 ) ;
#34198 = VECTOR ( 'NONE', #12852, 1000.000000000000000 ) ;
#34199 = ORIENTED_EDGE ( 'NONE', *, *, #29581, .F. ) ;
#34200 = AXIS2_PLACEMENT_3D ( 'NONE', #28420, #3667, #25739 ) ;
#34201 = AXIS2_PLACEMENT_3D ( 'NONE', #29872, #11186, #32520 ) ;
#34202 = VECTOR ( 'NONE', #23452, 1000.000000000000000 ) ;
#34203 = VECTOR ( 'NONE', #24203, 1000.000000000000000 ) ;
#34204 = ORIENTED_EDGE ( 'NONE', *, *, #4110, .F. ) ;
#34205 = ORIENTED_EDGE ( 'NONE', *, *, #26079, .F. ) ;
#34206 = CYLINDRICAL_SURFACE ( 'NONE', #18187, 4.750000000000004441 ) ;
#34207 = ORIENTED_EDGE ( 'NONE', *, *, #16575, .F. ) ;
#34208 = ORIENTED_EDGE ( 'NONE', *, *, #30493, .T. ) ;
#34209 = ORIENTED_EDGE ( 'NONE', *, *, #34600, .T. ) ;
#34210 = EDGE_CURVE ( 'NONE', #22709, #24130, #8944, .T. ) ;
#34211 = DIRECTION ( 'NONE',  ( -1.000000000000000000, -0.000000000000000000, -0.000000000000000000 ) ) ;
#34212 = CIRCLE ( 'NONE', #17753, 1.999999999999999556 ) ;
#34213 = ORIENTED_EDGE ( 'NONE', *, *, #31103, .T. ) ;
#34214 = CARTESIAN_POINT ( 'NONE',  ( 0.000000000000000000, -33.69708579775584667, 49.43553178847298568 ) ) ;
#34215 = DIRECTION ( 'NONE',  ( 0.000000000000000000, 0.000000000000000000, 1.000000000000000000 ) ) ;
#34216 = ORIENTED_EDGE ( 'NONE', *, *, #26801, .T. ) ;
#34217 = ORIENTED_EDGE ( 'NONE', *, *, #4683, .F. ) ;
#34218 =( REPRESENTATION_RELATIONSHIP ('NONE','NONE', #23037, #15767 ) REPRESENTATION_RELATIONSHIP_WITH_TRANSFORMATION ( #12086 )SHAPE_REPRESENTATION_RELATIONSHIP( ) );
#34219 = DIRECTION ( 'NONE',  ( -1.000000000000000000, 0.000000000000000000, 0.000000000000000000 ) ) ;
#34220 = CYLINDRICAL_SURFACE ( 'NONE', #8998, 16.19999999999999929 ) ;
#34221 = EDGE_CURVE ( 'NONE', #3001, #10822, #32563, .T. ) ;
#34222 = DIRECTION ( 'NONE',  ( 0.000000000000000000, 0.000000000000000000, -1.000000000000000000 ) ) ;
#34223 = DIRECTION ( 'NONE',  ( 0.000000000000000000, 2.309213040847544338E-50, 1.000000000000000000 ) ) ;
#34224 = CARTESIAN_POINT ( 'NONE',  ( -499.9999999999999432, 104.9999999999999858, -187.0000000000000000 ) ) ;
#34225 = ORIENTED_EDGE ( 'NONE', *, *, #29342, .F. ) ;
#34226 = ADVANCED_FACE ( 'NONE', ( #32958, #25312 ), #33145, .T. ) ;
#34227 = VECTOR ( 'NONE', #30212, 1000.000000000000000 ) ;
#34228 = CARTESIAN_POINT ( 'NONE',  ( 6.857172176539690689, 37.23415287044795718, -36.68877005347593467 ) ) ;
#34229 = CARTESIAN_POINT ( 'NONE',  ( -5.021133111224679091, 26.05646109878476580, -87.50000000000000000 ) ) ;
#34230 = ADVANCED_FACE ( 'NONE', ( #30663 ), #16982, .F. ) ;
#34231 = AXIS2_PLACEMENT_3D ( 'NONE', #18111, #34453, #15954 ) ;
#34232 = LINE ( 'NONE', #34053, #29552 ) ;
#34233 = ORIENTED_EDGE ( 'NONE', *, *, #12842, .F. ) ;
#34234 = VECTOR ( 'NONE', #13145, 1000.000000000000000 ) ;
#34235 = DIRECTION ( 'NONE',  ( 0.9941379571543593752, -0.1081190184239433083, -0.000000000000000000 ) ) ;
#34236 = CARTESIAN_POINT ( 'NONE',  ( 2.789999999999999147, -5.984944020945660803, -31.37417528048448645 ) ) ;
#34237 = DIRECTION ( 'NONE',  ( 1.232595164407830946E-32, 0.000000000000000000, 1.000000000000000000 ) ) ;
#34239 = CARTESIAN_POINT ( 'NONE',  ( 0.000000000000000000, 3.524919873834583163E-15, 68.31122994652405112 ) ) ;
#34238 = DIRECTION ( 'NONE',  ( 0.000000000000000000, 1.000000000000000000, 5.145227585319922065E-49 ) ) ;
#34240 = CARTESIAN_POINT ( 'NONE',  ( -70.00000000000000000, 4.559999999999908127, 172.9900000000000091 ) ) ;
#34241 = ORIENTED_EDGE ( 'NONE', *, *, #5875, .T. ) ;
#34242 = DIRECTION ( 'NONE',  ( 0.000000000000000000, 1.836970198721029441E-16, -1.000000000000000000 ) ) ;
#34244 = CARTESIAN_POINT ( 'NONE',  ( 0.000000000000000000, 0.000000000000000000, 3.180000000000000160 ) ) ;
#34243 = CYLINDRICAL_SURFACE ( 'NONE', #28569, 2.036051781435517682 ) ;
#34245 = VERTEX_POINT ( 'NONE', #11628 ) ;
#34246 = PRODUCT_DEFINITION_SHAPE ( 'NONE', 'NONE',  #35123 ) ;
#34247 = CARTESIAN_POINT ( 'NONE',  ( 28.23027531293552528, -17.65143121711728469, 20.00000000000000000 ) ) ;
#34248 = ORIENTED_EDGE ( 'NONE', *, *, #8485, .F. ) ;
#34249 = VECTOR ( 'NONE', #26227, 1000.000000000000227 ) ;
#34250 = VECTOR ( 'NONE', #12455, 1000.000000000000000 ) ;
#34251 = COLOUR_RGB ( '',0.7921568627450980005, 0.8196078431372548767, 0.9333333333333333481 ) ;
#34252 = AXIS2_PLACEMENT_3D ( 'NONE', #28592, #3494, #6691 ) ;
#34253 = ORIENTED_EDGE ( 'NONE', *, *, #10275, .F. ) ;
#34254 = DIRECTION ( 'NONE',  ( 0.4198891015602644883, 0.9075754196709571175, 0.000000000000000000 ) ) ;
#34255 = ORIENTED_EDGE ( 'NONE', *, *, #32090, .T. ) ;
#34256 = ORIENTED_EDGE ( 'NONE', *, *, #13585, .F. ) ;
#34257 = DIRECTION ( 'NONE',  ( 1.000000000000000000, 3.469446951953834515E-18, 0.000000000000000000 ) ) ;
#34258 = LINE ( 'NONE', #21078, #10668 ) ;
#34259 = PLANE ( 'NONE',  #33004 ) ;
#34260 = VERTEX_POINT ( 'NONE', #22480 ) ;
#34261 = ORIENTED_EDGE ( 'NONE', *, *, #17723, .F. ) ;
#34262 = CARTESIAN_POINT ( 'NONE',  ( 50.00050000000000239, 9.539392014169456147, -3.000000000000000000 ) ) ;
#34263 = CARTESIAN_POINT ( 'NONE',  ( -6.246745248748235768E-16, -30.07665394020986227, -5.960573492977661481 ) ) ;
#34264 = FACE_OUTER_BOUND ( 'NONE', #25919, .T. ) ;
#34265 = EDGE_CURVE ( 'NONE', #14153, #33515, #15718, .T. ) ;
#34266 = LINE ( 'NONE', #33562, #15298 ) ;
#34267 = CARTESIAN_POINT ( 'NONE',  ( 0.000000000000000000, 0.000000000000000000, 20.00000000000000000 ) ) ;
#34268 = ORIENTED_EDGE ( 'NONE', *, *, #11998, .F. ) ;
#34269 = ORIENTED_EDGE ( 'NONE', *, *, #10878, .F. ) ;
#34270 = CARTESIAN_POINT ( 'NONE',  ( 2.783128947185056656, 30.38119646769590787, -5.469045072944661356 ) ) ;
#34271 = EDGE_CURVE ( 'NONE', #1639, #2071, #11813, .T. ) ;
#34272 = DIRECTION ( 'NONE',  ( -0.000000000000000000, -0.000000000000000000, -1.000000000000000000 ) ) ;
#34273 = ORIENTED_EDGE ( 'NONE', *, *, #16898, .F. ) ;
#34274 = EDGE_CURVE ( 'NONE', #25337, #1716, #32791, .T. ) ;
#34275 = DIRECTION ( 'NONE',  ( -1.000000000000000000, -3.040835319149746528E-31, -1.232595164407830946E-32 ) ) ;
#34276 = CARTESIAN_POINT ( 'NONE',  ( 1.040000000000000924, 0.000000000000000000, 0.000000000000000000 ) ) ;
#34277 = LINE ( 'NONE', #9893, #12673 ) ;
#34278 = VERTEX_POINT ( 'NONE', #25485 ) ;
#34279 = VECTOR ( 'NONE', #20586, 1000.000000000000000 ) ;
#34280 = AXIS2_PLACEMENT_3D ( 'NONE', #14254, #3022, #19597 ) ;
#34281 = CIRCLE ( 'NONE', #23476, 2.525000000000003020 ) ;
#34282 = DIRECTION ( 'NONE',  ( 0.000000000000000000, 0.000000000000000000, 1.000000000000000000 ) ) ;
#34283 = ORIENTED_EDGE ( 'NONE', *, *, #33988, .F. ) ;
#34284 = DIRECTION ( 'NONE',  ( 0.000000000000000000, 0.000000000000000000, 1.000000000000000000 ) ) ;
#34285 = CARTESIAN_POINT ( 'NONE',  ( -108.1244492803746766, 4.063381404898920302, 11.82275161328742286 ) ) ;
#34286 = ADVANCED_FACE ( 'NONE', ( #17848 ), #28513, .F. ) ;
#34287 = ORIENTED_EDGE ( 'NONE', *, *, #16602, .T. ) ;
#34288 = DIRECTION ( 'NONE',  ( 0.000000000000000000, -1.000000000000000000, 6.842277657836020854E-49 ) ) ;
#34289 = CARTESIAN_POINT ( 'NONE',  ( -20.82057426567703473, -31.63141042832691952, -36.68877005347593467 ) ) ;
#34290 = VERTEX_POINT ( 'NONE', #31188 ) ;
#34291=STYLED_ITEM('',(#35268),#22481);
#34292 = DIRECTION ( 'NONE',  ( -2.253518519522067372E-14, -5.195982370170459947E-14, 0.9999999999999998890 ) ) ;
#34293 = ORIENTED_EDGE ( 'NONE', *, *, #23967, .F. ) ;
#34294 = CARTESIAN_POINT ( 'NONE',  ( 99.77990078431651000, -2.389942209051219901, 12.27067588826158762 ) ) ;
#34295 = ORIENTED_EDGE ( 'NONE', *, *, #28565, .F. ) ;
#34296 = CARTESIAN_POINT ( 'NONE',  ( 1.395000000000002238, -34.41385771548413430, 0.2702793785568976537 ) ) ;
#34297 = AXIS2_PLACEMENT_3D ( 'NONE', #33244, #13855, #27369 ) ;
#34298 = DIRECTION ( 'NONE',  ( 0.000000000000000000, 1.000000000000000000, 1.224646799147353207E-16 ) ) ;
#34299 = CARTESIAN_POINT ( 'NONE',  ( 22.10765473302597073, -16.64466345897532662, -77.50000000000000000 ) ) ;
#34300 = CARTESIAN_POINT ( 'NONE',  ( 0.07094833575216234756, 31.58891575048174971, -2.579090161526253588 ) ) ;
#34301 = ITEM_DEFINED_TRANSFORMATION ( 'NONE', 'NONE', #33150,  #28566 ) ;
#34302 = ORIENTED_EDGE ( 'NONE', *, *, #19419, .F. ) ;
#34303 = VERTEX_POINT ( 'NONE', #4108 ) ;
#34304 = PRODUCT_DEFINITION_SHAPE ( 'NONE', 'NONE',  #35200 ) ;
#34305 = ORIENTED_EDGE ( 'NONE', *, *, #10871, .T. ) ;
#34306 = FACE_OUTER_BOUND ( 'NONE', #3329, .T. ) ;
#34307 = EDGE_CURVE ( 'NONE', #30129, #20922, #20641, .T. ) ;
#34308 = CARTESIAN_POINT ( 'NONE',  ( -442.0000000000000000, 104.9999999999999858, -155.0000000000000000 ) ) ;
#34309 = DIRECTION ( 'NONE',  ( 0.000000000000000000, -1.310824597558155437E-49, -1.000000000000000000 ) ) ;
#34310 = CARTESIAN_POINT ( 'NONE',  ( 2.033589658306851344, 5.833445725193281639, -33.41010632092317678 ) ) ;
#34311 = CARTESIAN_POINT ( 'NONE',  ( 2.789999999999999147, 17.11426446101236820, -26.96776559937708129 ) ) ;
#34312 = CARTESIAN_POINT ( 'NONE',  ( 2.789999999999999147, -25.79731400673761144, -16.24908301080859374 ) ) ;
#34313 = VERTEX_POINT ( 'NONE', #34022 ) ;
#34314 = EDGE_CURVE ( 'NONE', #32798, #7621, #12157, .T. ) ;
#34315 = PLANE ( 'NONE',  #28208 ) ;
#34316 = EDGE_CURVE ( 'NONE', #16011, #20178, #5828, .T. ) ;
#34317 = CARTESIAN_POINT ( 'NONE',  ( 100.0353719831124977, 2.883232572601701627, 12.16410353805738964 ) ) ;
#34318 = ORIENTED_EDGE ( 'NONE', *, *, #28945, .T. ) ;
#34319 = AXIS2_PLACEMENT_3D ( 'NONE', #21520, #7973, #29698 ) ;
#34320 = EDGE_CURVE ( 'NONE', #15570, #17480, #7620, .T. ) ;
#34321 = EDGE_CURVE ( 'NONE', #20282, #26849, #15276, .T. ) ;
#34322 = DIRECTION ( 'NONE',  ( 0.000000000000000000, 1.836970198721029441E-16, -1.000000000000000000 ) ) ;
#34323 = VERTEX_POINT ( 'NONE', #1627 ) ;
#34324 = DIRECTION ( 'NONE',  ( 0.000000000000000000, -0.8660254037844382635, -0.5000000000000008882 ) ) ;
#34325 = ADVANCED_FACE ( 'NONE', ( #9646 ), #6788, .T. ) ;
#34326 = DIRECTION ( 'NONE',  ( 1.000000000000000000, 0.000000000000000000, -1.300283923313630633E-47 ) ) ;
#34327 = AXIS2_PLACEMENT_3D ( 'NONE', #10624, #7396, #34924 ) ;
#34328 = AXIS2_PLACEMENT_3D ( 'NONE', #18932, #16088, #16621 ) ;
#34329 = AXIS2_PLACEMENT_3D ( 'NONE', #29161, #20632, #4756 ) ;
#34330 = DIRECTION ( 'NONE',  ( 0.000000000000000000, 0.000000000000000000, 1.000000000000000000 ) ) ;
#34331 = DIRECTION ( 'NONE',  ( -0.000000000000000000, -0.000000000000000000, 1.000000000000000000 ) ) ;
#34332 = LINE ( 'NONE', #1073, #21721 ) ;
#34334 = EDGE_CURVE ( 'NONE', #23007, #6336, #26012, .T. ) ;
#34333 = VERTEX_POINT ( 'NONE', #23179 ) ;
#34335 = EDGE_LOOP ( 'NONE', ( #19661, #241, #17367, #20486, #9867, #1814, #20302, #26901 ) ) ;
#34336 = DIRECTION ( 'NONE',  ( -0.1063910735369017202, 0.9943243633099136947, -1.000770725407181676E-14 ) ) ;
#34337 = ORIENTED_EDGE ( 'NONE', *, *, #901, .F. ) ;
#34338 = CARTESIAN_POINT ( 'NONE',  ( 2.789999999999999591, -29.22790002295970524, -9.266248432308945127 ) ) ;
#34339 = VECTOR ( 'NONE', #3863, 1000.000000000000114 ) ;
#34340 = LINE ( 'NONE', #6090, #1386 ) ;
#34341 = CARTESIAN_POINT ( 'NONE',  ( 99.34337556290111593, -0.9828571727418841109, 7.437816238889399578 ) ) ;
#34342 = ORIENTED_EDGE ( 'NONE', *, *, #13691, .F. ) ;
#34343 = MANIFOLD_SOLID_BREP ( 'Boss-Extrude6[2]', #20200 ) ;
#34344 = CARTESIAN_POINT ( 'NONE',  ( 0.000000000000000000, 6.992329373473909019E-15, 49.43553178847298568 ) ) ;
#34345 = CIRCLE ( 'NONE', #6492, 4.000000000000003553 ) ;
#34346 = CARTESIAN_POINT ( 'NONE',  ( 0.000000000000000000, -5.984944020945660803, -31.37417528048448645 ) ) ;
#34348 = DIRECTION ( 'NONE',  ( 0.000000000000000000, 1.000000000000000000, 0.000000000000000000 ) ) ;
#34347 = CARTESIAN_POINT ( 'NONE',  ( 17.88561705399010293, -27.19023860642120383, 49.43553178847298568 ) ) ;
#34349 = CIRCLE ( 'NONE', #15061, 3.999999999999976019 ) ;
#34350 = VERTEX_POINT ( 'NONE', #6610 ) ;
#34351 = ORIENTED_EDGE ( 'NONE', *, *, #26085, .F. ) ;
#34352 = CIRCLE ( 'NONE', #263, 34.41491905851385269 ) ;
#34353 = CARTESIAN_POINT ( 'NONE',  ( 1.040000000000000480, 6.183021911001836735, 33.85493898757064812 ) ) ;
#34354 = EDGE_LOOP ( 'NONE', ( #15244, #17072, #13851, #31734, #15272, #10261, #24674, #5995, #22554, #17418, #28263, #17819, #30070 ) ) ;
#34355 = CARTESIAN_POINT ( 'NONE',  ( 2.789999999999999147, -26.36977540155018218, 15.20550475489928388 ) ) ;
#34356 = LINE ( 'NONE', #23678, #8585 ) ;
#34357 = ORIENTED_EDGE ( 'NONE', *, *, #33985, .F. ) ;
#34358 = CARTESIAN_POINT ( 'NONE',  ( 0.02407890056655695096, -23.70329957282599764, 20.11932597908820242 ) ) ;
#34359 = EDGE_CURVE ( 'NONE', #7716, #2811, #7130, .T. ) ;
#34360 = ADVANCED_FACE ( 'NONE', ( #17514 ), #28345, .F. ) ;
#34361 = ORIENTED_EDGE ( 'NONE', *, *, #361, .F. ) ;
#34362 = DIRECTION ( 'NONE',  ( 0.000000000000000000, 0.000000000000000000, 1.000000000000000000 ) ) ;
#34363 = CARTESIAN_POINT ( 'NONE',  ( -500.0000000000000000, 144.9999999999999716, -155.0000000000000000 ) ) ;
#34364 = CARTESIAN_POINT ( 'NONE',  ( -361.0000000000000000, 124.9999999999999432, 181.0000000000000000 ) ) ;
#34366 = CARTESIAN_POINT ( 'NONE',  ( -145.0000000000000568, -177.8172209610550851, -45.87893859614474223 ) ) ;
#34365 = CARTESIAN_POINT ( 'NONE',  ( 0.02407890056655825201, -31.05158812718220673, -1.559667679918931738 ) ) ;
#34367 = CIRCLE ( 'NONE', #19598, 2.000000000000001776 ) ;
#34368 = DIRECTION ( 'NONE',  ( 0.000000000000000000, 0.000000000000000000, 1.000000000000000000 ) ) ;
#34369 = FACE_OUTER_BOUND ( 'NONE', #19211, .T. ) ;
#34370 = CARTESIAN_POINT ( 'NONE',  ( 0.000000000000000000, 32.54542015209057126, 76.74945698428001606 ) ) ;
#34371 = DIRECTION ( 'NONE',  ( -1.000000000000000000, 0.000000000000000000, -0.000000000000000000 ) ) ;
#34372 = CIRCLE ( 'NONE', #33818, 30.47050528711512030 ) ;
#34373 = EDGE_CURVE ( 'NONE', #18350, #19066, #22340, .T. ) ;
#34374 = VECTOR ( 'NONE', #14548, 1000.000000000000000 ) ;
#34376 = VERTEX_POINT ( 'NONE', #4985 ) ;
#34375 = CIRCLE ( 'NONE', #10532, 34.41491905851385269 ) ;
#34377 = AXIS2_PLACEMENT_3D ( 'NONE', #11187, #4945, #13156 ) ;
#34378 = ORIENTED_EDGE ( 'NONE', *, *, #7737, .F. ) ;
#34380 = ORIENTED_EDGE ( 'NONE', *, *, #31549, .F. ) ;
#34379 = ADVANCED_FACE ( 'NONE', ( #34548 ), #24384, .T. ) ;
#34381 = EDGE_CURVE ( 'NONE', #33934, #30641, #12317, .T. ) ;
#34382 = EDGE_CURVE ( 'NONE', #26602, #6257, #18686, .T. ) ;
#34383 = DIRECTION ( 'NONE',  ( -1.000000000000000000, -0.000000000000000000, -0.000000000000000000 ) ) ;
#34384 = CARTESIAN_POINT ( 'NONE',  ( 818.3260927326359706, 1336.536139717604328, 1753.598338701303419 ) ) ;
#34385 = ORIENTED_EDGE ( 'NONE', *, *, #10272, .T. ) ;
#34386 = ORIENTED_EDGE ( 'NONE', *, *, #30025, .F. ) ;
#34387 = ORIENTED_EDGE ( 'NONE', *, *, #14292, .T. ) ;
#34388 = CARTESIAN_POINT ( 'NONE',  ( -430.0000000000000000, 134.9999999999999716, 126.0000000000000000 ) ) ;
#34389 = ADVANCED_FACE ( 'NONE', ( #15885 ), #17260, .T. ) ;
#34390 = CONTEXT_DEPENDENT_SHAPE_REPRESENTATION ( #1936, #19001 ) ;
#34391 = VECTOR ( 'NONE', #9265, 1000.000000000000000 ) ;
#34392 = ORIENTED_EDGE ( 'NONE', *, *, #32176, .T. ) ;
#34393 = DIRECTION ( 'NONE',  ( 0.000000000000000000, -1.000000000000000000, -5.145227585319922065E-49 ) ) ;
#34394 = DIRECTION ( 'NONE',  ( 0.000000000000000000, 1.000000000000000000, 1.836970198721029688E-16 ) ) ;
#34395 = VERTEX_POINT ( 'NONE', #11 ) ;
#34396 = ORIENTED_EDGE ( 'NONE', *, *, #1394, .F. ) ;
#34397 = CYLINDRICAL_SURFACE ( 'NONE', #16887, 3.999999999999976019 ) ;
#34398 = CIRCLE ( 'NONE', #7174, 2.036051781435517682 ) ;
#34399 = DIRECTION ( 'NONE',  ( 1.000000000000000000, 0.000000000000000000, 0.000000000000000000 ) ) ;
#34400 = CONICAL_SURFACE ( 'NONE', #16819, 32.54542015209057126, 1.110254297872109275 ) ;
#34401 = CARTESIAN_POINT ( 'NONE',  ( 1.040000000000000036, 14.40815186467775533, 31.25366880301323746 ) ) ;
#34402 = DIRECTION ( 'NONE',  ( -1.000000000000000000, 0.000000000000000000, -0.000000000000000000 ) ) ;
#34403 = CARTESIAN_POINT ( 'NONE',  ( -12.00000000000001066, 140.9999999999999716, 155.0000000000000000 ) ) ;
#34404 = ORIENTED_EDGE ( 'NONE', *, *, #10768, .T. ) ;
#34405 = DIRECTION ( 'NONE',  ( -0.000000000000000000, 0.000000000000000000, -1.000000000000000000 ) ) ;
#34406 = LINE ( 'NONE', #4653, #7119 ) ;
#34407 = EDGE_CURVE ( 'NONE', #28097, #22681, #24029, .T. ) ;
#34408 = AXIS2_PLACEMENT_3D ( 'NONE', #18286, #28603, #12769 ) ;
#34409 = DIRECTION ( 'NONE',  ( 1.000000000000000000, 0.000000000000000000, -5.546364386991661285E-52 ) ) ;
#34410 = EDGE_LOOP ( 'NONE', ( #20427, #24428, #2346, #3940, #13810, #10454 ) ) ;
#34411 = TOROIDAL_SURFACE ( 'NONE', #9397, 30.47050528711511674, 8.000000000000000000 ) ;
#34412 = CYLINDRICAL_SURFACE ( 'NONE', #28278, 7.999999999999979572 ) ;
#34413 = CARTESIAN_POINT ( 'NONE',  ( -499.9999999999999432, 144.9999999999999716, -162.9999999999999716 ) ) ;
#34414 = FACE_OUTER_BOUND ( 'NONE', #27744, .T. ) ;
#34416 = DIRECTION ( 'NONE',  ( 1.000000000000000000, 0.000000000000000000, 0.000000000000000000 ) ) ;
#34415 = CARTESIAN_POINT ( 'NONE',  ( 11.99999999999999645, -124.9999999999999432, -194.9999999999999432 ) ) ;
#34417 = AXIS2_PLACEMENT_3D ( 'NONE', #30719, #11871, #25186 ) ;
#34418 = CARTESIAN_POINT ( 'NONE',  ( 22.89764159710615132, -3.615060903476079890, -77.50000000000000000 ) ) ;
#34419 = VERTEX_POINT ( 'NONE', #26885 ) ;
#34420 = FACE_OUTER_BOUND ( 'NONE', #10792, .T. ) ;
#34422 = FACE_OUTER_BOUND ( 'NONE', #27500, .T. ) ;
#34421 = DIRECTION ( 'NONE',  ( 0.000000000000000000, 1.000000000000000000, 0.000000000000000000 ) ) ;
#34423 = AXIS2_PLACEMENT_3D ( 'NONE', #5787, #16684, #27519 ) ;
#34424 = ORIENTED_EDGE ( 'NONE', *, *, #2074, .T. ) ;
#34425 = FACE_OUTER_BOUND ( 'NONE', #31438, .T. ) ;
#34426 = AXIS2_PLACEMENT_3D ( 'NONE', #14857, #33702, #22689 ) ;
#34427 = EDGE_LOOP ( 'NONE', ( #20995, #33572, #10764, #16324 ) ) ;
#34428 = EDGE_CURVE ( 'NONE', #25965, #9066, #6979, .T. ) ;
#34429 = ADVANCED_FACE ( 'NONE', ( #32042 ), #188, .T. ) ;
#34430 =( REPRESENTATION_RELATIONSHIP ('NONE','NONE', #23037, #15767 ) REPRESENTATION_RELATIONSHIP_WITH_TRANSFORMATION ( #32894 )SHAPE_REPRESENTATION_RELATIONSHIP( ) );
#34431 = EDGE_LOOP ( 'NONE', ( #12072, #30422, #420, #25670 ) ) ;
#34432 = FACE_OUTER_BOUND ( 'NONE', #13718, .T. ) ;
#34433 = ORIENTED_EDGE ( 'NONE', *, *, #34470, .F. ) ;
#34434 = EDGE_LOOP ( 'NONE', ( #12902, #28556, #33482, #27390 ) ) ;
#34435 = DIRECTION ( 'NONE',  ( -1.000000000000000000, 0.000000000000000000, 0.000000000000000000 ) ) ;
#34436 = CIRCLE ( 'NONE', #905, 4.750000000000004441 ) ;
#34437 = CARTESIAN_POINT ( 'NONE',  ( 5.021133111224369117, -3.725253662474300231, -87.50000000000000000 ) ) ;
#34438 = CARTESIAN_POINT ( 'NONE',  ( 143.0000000000000568, -99.56883598056833762, -180.0000000000000000 ) ) ;
#34439 = ORIENTED_EDGE ( 'NONE', *, *, #27071, .T. ) ;
#34440 = EDGE_LOOP ( 'NONE', ( #18001, #10863, #3064, #18987 ) ) ;
#34441 = LINE ( 'NONE', #1861, #33861 ) ;
#34442 = CARTESIAN_POINT ( 'NONE',  ( 11.99999999999999645, 134.9999999999998863, 194.9999999999999716 ) ) ;
#34443 = CARTESIAN_POINT ( 'NONE',  ( 0.02407890056655651728, 11.80989368511502846, -28.76039115933972923 ) ) ;
#34444 = DIRECTION ( 'NONE',  ( -1.000000000000000000, 0.000000000000000000, 1.848892746611746966E-32 ) ) ;
#34445 = ORIENTED_EDGE ( 'NONE', *, *, #2562, .T. ) ;
#34446 = ORIENTED_EDGE ( 'NONE', *, *, #418, .F. ) ;
#34447 = AXIS2_PLACEMENT_3D ( 'NONE', #17172, #27825, #19138 ) ;
#34448 = DIRECTION ( 'NONE',  ( -1.000000000000000000, -3.040835319149746528E-31, -1.232595164407830946E-32 ) ) ;
#34449 = CARTESIAN_POINT ( 'NONE',  ( -12.00000000000003908, -145.0000000000000000, -154.9999999999999716 ) ) ;
#34450 = ORIENTED_EDGE ( 'NONE', *, *, #22152, .F. ) ;
#34451 = CIRCLE ( 'NONE', #22524, 5.738084889453667792 ) ;
#34452 = CARTESIAN_POINT ( 'NONE',  ( 3.235562306570555532E-30, 18.16264470403145026, -67.50000000000000000 ) ) ;
#34453 = DIRECTION ( 'NONE',  ( 0.000000000000000000, 0.000000000000000000, 1.000000000000000000 ) ) ;
#34454 = ORIENTED_EDGE ( 'NONE', *, *, #34274, .F. ) ;
#34455 = CARTESIAN_POINT ( 'NONE',  ( 212.5000000000000000, 0.000000000000000000, 7.500000000000000000 ) ) ;
#34456 = ORIENTED_EDGE ( 'NONE', *, *, #22597, .F. ) ;
#34457 = DIRECTION ( 'NONE',  ( 1.000000000000000000, -0.000000000000000000, 0.000000000000000000 ) ) ;
#34458 = ORIENTED_EDGE ( 'NONE', *, *, #22798, .T. ) ;
#34459 = CYLINDRICAL_SURFACE ( 'NONE', #21960, 2.525000000000003020 ) ;
#34461 = MECHANICAL_DESIGN_GEOMETRIC_PRESENTATION_REPRESENTATION (  '', ( #23097 ), #17446 ) ;
#34460 = DIRECTION ( 'NONE',  ( 0.000000000000000000, 0.000000000000000000, -1.000000000000000000 ) ) ;
#34462 = CIRCLE ( 'NONE', #28772, 7.999999999999979572 ) ;
#34463 = ORIENTED_EDGE ( 'NONE', *, *, #15727, .T. ) ;
#34464 = VECTOR ( 'NONE', #4684, 999.9999999999998863 ) ;
#34465 = DIRECTION ( 'NONE',  ( -0.000000000000000000, -1.836970198721029688E-16, 1.000000000000000000 ) ) ;
#34466 = DIRECTION ( 'NONE',  ( 1.000000000000000000, 0.000000000000000000, 0.000000000000000000 ) ) ;
#34467 = ADVANCED_FACE ( 'NONE', ( #18372 ), #32228, .T. ) ;
#34468 = EDGE_LOOP ( 'NONE', ( #29710, #27951, #10919, #33715 ) ) ;
#34469 = VECTOR ( 'NONE', #5008, 1000.000000000000000 ) ;
#34470 = EDGE_CURVE ( 'NONE', #5322, #26512, #28032, .T. ) ;
#34471 = DIRECTION ( 'NONE',  ( -7.893605728314051750E-14, 1.618803117314786530E-15, 1.000000000000000000 ) ) ;
#34472 = ORIENTED_EDGE ( 'NONE', *, *, #2592, .F. ) ;
#34473 = CARTESIAN_POINT ( 'NONE',  ( 100.4534127715137544, -3.505526250977490488, 11.99932421786962244 ) ) ;
#34474 = EDGE_CURVE ( 'NONE', #31695, #5771, #5157, .T. ) ;
#34475 = ORIENTED_EDGE ( 'NONE', *, *, #22711, .F. ) ;
#34476 = AXIS2_PLACEMENT_3D ( 'NONE', #13838, #24671, #311 ) ;
#34477 = DIRECTION ( 'NONE',  ( 1.000000000000000000, 0.000000000000000000, -0.000000000000000000 ) ) ;
#34478 = DIRECTION ( 'NONE',  ( 0.000000000000000000, -3.017235169886638201E-16, 1.000000000000000000 ) ) ;
#34479 = CARTESIAN_POINT ( 'NONE',  ( 35.44043929807611448, -17.65143121711728469, 10.00000000000000000 ) ) ;
#34480 = CARTESIAN_POINT ( 'NONE',  ( 1.040000000000002922, 34.17636915695680244, -4.045051921974834208 ) ) ;
#34481 = ORIENTED_EDGE ( 'NONE', *, *, #2968, .T. ) ;
#34482 = VERTEX_POINT ( 'NONE', #16229 ) ;
#34483 = ORIENTED_EDGE ( 'NONE', *, *, #9447, .F. ) ;
#34484 = DIRECTION ( 'NONE',  ( 0.000000000000000000, -0.08715574274766170471, -0.9961946980917453232 ) ) ;
#34485 = AXIS2_PLACEMENT_3D ( 'NONE', #25887, #4154, #30530 ) ;
#34486 = CARTESIAN_POINT ( 'NONE',  ( -8.242531583266565685E-14, -3.624739946994197215, 30.44774159452261486 ) ) ;
#34487 = DIRECTION ( 'NONE',  ( 0.000000000000000000, 1.836970198721029441E-16, -1.000000000000000000 ) ) ;
#34488 = CARTESIAN_POINT ( 'NONE',  ( -418.0000000000000000, 105.0000000000000142, -109.9999999999999574 ) ) ;
#34489 = LINE ( 'NONE', #17974, #23697 ) ;
#34490 = DIRECTION ( 'NONE',  ( 0.000000000000000000, 1.000000000000000000, 5.053935297177146739E-49 ) ) ;
#34491 = ORIENTED_EDGE ( 'NONE', *, *, #31891, .F. ) ;
#34492 = PRODUCT_DEFINITION_SHAPE ( 'NONE', 'NONE',  #35183 ) ;
#34493 = CIRCLE ( 'NONE', #1037, 32.54542015209055705 ) ;
#34494 = DIRECTION ( 'NONE',  ( -1.000000000000000000, 0.000000000000000000, 0.000000000000000000 ) ) ;
#34495 = CARTESIAN_POINT ( 'NONE',  ( 143.0000000000000568, 85.49999999999998579, -63.00000000000000000 ) ) ;
#34496 = CARTESIAN_POINT ( 'NONE',  ( -499.9999999999998863, -109.0000000000000142, -162.9999999999999716 ) ) ;
#34497 = ORIENTED_EDGE ( 'NONE', *, *, #6612, .F. ) ;
#34498 = CIRCLE ( 'NONE', #28251, 30.47050528711512030 ) ;
#34499 = CARTESIAN_POINT ( 'NONE',  ( 145.0000000000000568, -87.50000000000000000, 65.00000000000000000 ) ) ;
#34500 = ORIENTED_EDGE ( 'NONE', *, *, #21079, .F. ) ;
#34501 = CARTESIAN_POINT ( 'NONE',  ( 10.00000000000000000, 15.58845726811990495, 0.000000000000000000 ) ) ;
#34502 = DIRECTION ( 'NONE',  ( -0.4198891015602644883, -0.9075754196709571175, 0.000000000000000000 ) ) ;
#34503 = ORIENTED_EDGE ( 'NONE', *, *, #4110, .T. ) ;
#34504 = EDGE_CURVE ( 'NONE', #28875, #31191, #10707, .T. ) ;
#34505 = CARTESIAN_POINT ( 'NONE',  ( 0.02407890056655651728, 7.350529080603541487, 30.20932655202940254 ) ) ;
#34506 = CYLINDRICAL_SURFACE ( 'NONE', #16801, 3.999999999999976019 ) ;
#34507 = FACE_OUTER_BOUND ( 'NONE', #2547, .T. ) ;
#34508 = EDGE_CURVE ( 'NONE', #30531, #9222, #10525, .T. ) ;
#34509 = ORIENTED_EDGE ( 'NONE', *, *, #3289, .F. ) ;
#34510 = ORIENTED_EDGE ( 'NONE', *, *, #21700, .F. ) ;
#34511 = DIRECTION ( 'NONE',  ( -7.893605728314050488E-14, 1.618803117314786135E-15, 0.9999999999999998890 ) ) ;
#34512 = ADVANCED_FACE ( 'NONE', ( #21556 ), #8014, .F. ) ;
#34513 = EDGE_LOOP ( 'NONE', ( #23727, #24117, #30094, #1435 ) ) ;
#34514 = AXIS2_PLACEMENT_3D ( 'NONE', #23933, #11304, #19150 ) ;
#34515 = CARTESIAN_POINT ( 'NONE',  ( 0.5248941893598875197, -32.51534716424833960, -7.547378828040798737 ) ) ;
#34516 = VECTOR ( 'NONE', #27006, 1000.000000000000000 ) ;
#34517 = AXIS2_PLACEMENT_3D ( 'NONE', #28333, #4274, #33846 ) ;
#34518 = DIRECTION ( 'NONE',  ( 0.000000000000000000, 2.309213040847544338E-50, 1.000000000000000000 ) ) ;
#34519 = CARTESIAN_POINT ( 'NONE',  ( 0.006892386851572370257, -27.79373726981368620, -13.43326644626254662 ) ) ;
#34520 = ADVANCED_FACE ( 'NONE', ( #23693 ), #32749, .F. ) ;
#34521 = VERTEX_POINT ( 'NONE', #11047 ) ;
#34522 = CARTESIAN_POINT ( 'NONE',  ( 1.394999999999999574, -10.37741591188917134, 32.81304455236865181 ) ) ;
#34523 = EDGE_CURVE ( 'NONE', #17865, #32956, #22433, .T. ) ;
#34524 = EDGE_CURVE ( 'NONE', #10781, #27819, #14437, .T. ) ;
#34525 = VECTOR ( 'NONE', #16513, 1000.000000000000114 ) ;
#34527 = DIRECTION ( 'NONE',  ( -0.000000000000000000, 1.000000000000000000, -0.000000000000000000 ) ) ;
#34526 = CARTESIAN_POINT ( 'NONE',  ( 1.749999999999999778, 27.68252950111338251, 20.44661865013498669 ) ) ;
#34528 = ORIENTED_EDGE ( 'NONE', *, *, #8948, .F. ) ;
#34529 = ORIENTED_EDGE ( 'NONE', *, *, #27872, .T. ) ;
#34530 = CARTESIAN_POINT ( 'NONE',  ( 0.07094833381203961842, 4.557485336350485028, 31.36463980626633941 ) ) ;
#34531 = ORIENTED_EDGE ( 'NONE', *, *, #17651, .T. ) ;
#34532 = CARTESIAN_POINT ( 'NONE',  ( -12.00000000000001066, -145.0000000000000000, -194.9999999999999432 ) ) ;
#34533 = CARTESIAN_POINT ( 'NONE',  ( 11.99999999999999645, -105.0000000000000142, 155.0000000000000000 ) ) ;
#34534 = EDGE_LOOP ( 'NONE', ( #18540, #32714, #20433, #30804 ) ) ;
#34535 = CARTESIAN_POINT ( 'NONE',  ( -430.0000000000000000, 116.9999999999999858, 126.0000000000000000 ) ) ;
#34536 = VECTOR ( 'NONE', #4350, 1000.000000000000000 ) ;
#34537 = ORIENTED_EDGE ( 'NONE', *, *, #30540, .T. ) ;
#34538 = FACE_OUTER_BOUND ( 'NONE', #18288, .T. ) ;
#34539 = CARTESIAN_POINT ( 'NONE',  ( -6.500000000000000000, 0.000000000000000000, 3.930000000000000160 ) ) ;
#34540 = CARTESIAN_POINT ( 'NONE',  ( -8.000000000000000000, 0.000000000000000000, 0.000000000000000000 ) ) ;
#34542 = LINE ( 'NONE', #31854, #33290 ) ;
#34541 = DIRECTION ( 'NONE',  ( 0.000000000000000000, -0.000000000000000000, -1.000000000000000000 ) ) ;
#34543 = AXIS2_PLACEMENT_3D ( 'NONE', #19447, #11613, #3228 ) ;
#34544 = VECTOR ( 'NONE', #22186, 1000.000000000000114 ) ;
#34545 = CARTESIAN_POINT ( 'NONE',  ( 1.040000000000001812, -34.41385771548413430, -0.2702793785573777696 ) ) ;
#34546 = CARTESIAN_POINT ( 'NONE',  ( 0.000000000000000000, 49.99999999999999289, 0.000000000000000000 ) ) ;
#34547 = DIRECTION ( 'NONE',  ( -0.000000000000000000, 1.836970198721029934E-16, -1.000000000000000000 ) ) ;
#34548 = FACE_OUTER_BOUND ( 'NONE', #22128, .T. ) ;
#34549 = VECTOR ( 'NONE', #19139, 1000.000000000000000 ) ;
#34550 = VERTEX_POINT ( 'NONE', #21897 ) ;
#34551 = SHAPE_REPRESENTATION_RELATIONSHIP ( 'NONE' , 'NONE' ,  #1195, #17803 ) ;
#34552 = B_SPLINE_CURVE_WITH_KNOTS ( 'NONE', 3,
 ( #29291, #2228, #24107, #32123, #14776, #14947 ),
 .UNSPECIFIED., .F., .F.,
 ( 4, 2, 4 ),
 ( 4.404817104804532277E-07, 0.001874269682437030085, 0.003748098883163587889 ),
 .UNSPECIFIED. ) ;
#34553 = ORIENTED_EDGE ( 'NONE', *, *, #24368, .F. ) ;
#34554 = ORIENTED_EDGE ( 'NONE', *, *, #29486, .T. ) ;
#34555 = ADVANCED_FACE ( 'NONE', ( #22614, #32922, #33099 ), #372, .T. ) ;
#34556 = VECTOR ( 'NONE', #9128, 1000.000000000000000 ) ;
#34557 = EDGE_CURVE ( 'NONE', #15156, #17702, #10982, .T. ) ;
#34558 = CARTESIAN_POINT ( 'NONE',  ( 110.7380848894536598, -4.118294838564020743E-16, 7.500000000000000000 ) ) ;
#34559 = EDGE_CURVE ( 'NONE', #31620, #15103, #2847, .T. ) ;
#34560 = PRODUCT_CONTEXT ( 'NONE', #22376, 'mechanical' ) ;
#34561 = VERTEX_POINT ( 'NONE', #25081 ) ;
#34562 = EDGE_LOOP ( 'NONE', ( #12605, #25051, #4187, #33020 ) ) ;
#34563 = EDGE_LOOP ( 'NONE', ( #7642, #31657, #15723, #22802, #24108, #3189, #1638, #11823 ) ) ;
#34564 = LINE ( 'NONE', #20861, #24730 ) ;
#34565 = CARTESIAN_POINT ( 'NONE',  ( 2.765921099433442443, 20.99477179376825120, 22.93149026599753526 ) ) ;
#34566 = ITEM_DEFINED_TRANSFORMATION ( 'NONE', 'NONE', #8172,  #28566 ) ;
#34567 = VECTOR ( 'NONE', #12298, 1000.000000000000000 ) ;
#34568 = ORIENTED_EDGE ( 'NONE', *, *, #13776, .F. ) ;
#34569 = CARTESIAN_POINT ( 'NONE',  ( -0.9727285265192152641, -1.747512292859696670, -0.7500000000000000000 ) ) ;
#34570 = DIRECTION ( 'NONE',  ( 0.000000000000000000, -3.374343856708137958E-53, 1.000000000000000000 ) ) ;
#34571 = ORIENTED_EDGE ( 'NONE', *, *, #855, .T. ) ;
#34572 = ORIENTED_EDGE ( 'NONE', *, *, #9390, .T. ) ;
#34573 = COLOUR_RGB ( '',0.7921568627450980005, 0.8196078431372548767, 0.9333333333333333481 ) ;
#34574 = DIRECTION ( 'NONE',  ( 1.000000000000000000, 0.000000000000000000, 0.000000000000000000 ) ) ;
#34575 = DIRECTION ( 'NONE',  ( -1.000000000000000000, 0.000000000000000000, 0.000000000000000000 ) ) ;
#34576 = DIRECTION ( 'NONE',  ( -1.000000000000000000, 0.000000000000000000, 0.000000000000000000 ) ) ;
#34578 = ADVANCED_FACE ( 'NONE', ( #24548 ), #30256, .F. ) ;
#34577 = CARTESIAN_POINT ( 'NONE',  ( 15.99999999999998579, -124.9999999999999432, -162.9999999999999432 ) ) ;
#34579 = FACE_OUTER_BOUND ( 'NONE', #13815, .T. ) ;
#34580 = ORIENTED_EDGE ( 'NONE', *, *, #6730, .T. ) ;
#34581 = AXIS2_PLACEMENT_3D ( 'NONE', #26199, #9662, #31206 ) ;
#34582 = DIRECTION ( 'NONE',  ( -1.000000000000000000, 0.000000000000000000, 0.000000000000000000 ) ) ;
#34583 = CYLINDRICAL_SURFACE ( 'NONE', #28735, 8.000000000000007105 ) ;
#34584 = MANIFOLD_SOLID_BREP ( 'Trim/Extend6[2]', #4816 ) ;
#34585 = CARTESIAN_POINT ( 'NONE',  ( 23.31255882915076683, -22.70966696615087699, 49.43553178847298568 ) ) ;
#34586 = EDGE_CURVE ( 'NONE', #24110, #31132, #5861, .T. ) ;
#34587 = CYLINDRICAL_SURFACE ( 'NONE', #5847, 2.524999999999999467 ) ;
#34588 = VECTOR ( 'NONE', #25639, 1000.000000000000000 ) ;
#34589 = DIRECTION ( 'NONE',  ( 1.000000000000000000, 0.000000000000000000, -1.848892746611746966E-32 ) ) ;
#34591 = DIRECTION ( 'NONE',  ( -0.000000000000000000, -0.000000000000000000, -1.000000000000000000 ) ) ;
#34590 = CARTESIAN_POINT ( 'NONE',  ( -27.13361903382165963, -26.41607761506757868, 68.31122994652405112 ) ) ;
#34592 = EDGE_CURVE ( 'NONE', #10121, #28865, #30442, .T. ) ;
#34593 = AXIS2_PLACEMENT_3D ( 'NONE', #32764, #8557, #8389 ) ;
#34594 = ADVANCED_FACE ( 'NONE', ( #11584 ), #33283, .T. ) ;
#34595 = LINE ( 'NONE', #15556, #4758 ) ;
#34596 = VERTEX_POINT ( 'NONE', #11765 ) ;
#34597 = CARTESIAN_POINT ( 'NONE',  ( 30.69344702212033127, -10.82204614554912681, 68.31122994652405112 ) ) ;
#34599 = CARTESIAN_POINT ( 'NONE',  ( 0.000000000000000000, 11.69134295108991140, -6.750000000000015987 ) ) ;
#34598 = CARTESIAN_POINT ( 'NONE',  ( 2.789999999999999147, -5.984944020946091570, 31.37417528048439763 ) ) ;
#34600 = EDGE_CURVE ( 'NONE', #34561, #25561, #14355, .T. ) ;
#34601 = VERTEX_POINT ( 'NONE', #31308 ) ;
#34602 = CARTESIAN_POINT ( 'NONE',  ( -442.0000000000000000, -109.0000000000000142, -174.9999999999999716 ) ) ;
#34603 = PRODUCT_DEFINITION_SHAPE ( 'NONE', 'NONE',  #35224 ) ;
#34604 = ORIENTED_EDGE ( 'NONE', *, *, #23079, .T. ) ;
#34605 = AXIS2_PLACEMENT_3D ( 'NONE', #32335, #19188, #26826 ) ;
#34606 = EDGE_CURVE ( 'NONE', #5515, #31150, #33811, .T. ) ;
#34607 = EDGE_CURVE ( 'NONE', #18155, #5682, #26238, .T. ) ;
#34608 = ORIENTED_EDGE ( 'NONE', *, *, #30823, .T. ) ;
#34609 = DIRECTION ( 'NONE',  ( -0.9947866662129278836, 0.05393576583119111950, -0.08654722346309884351 ) ) ;
#34610 = ORIENTED_EDGE ( 'NONE', *, *, #209, .F. ) ;
#34611 = EDGE_LOOP ( 'NONE', ( #6700, #15536, #19995, #21573 ) ) ;
#34612 = LINE ( 'NONE', #21075, #12213 ) ;
#34613 = VECTOR ( 'NONE', #21361, 1000.000000000000000 ) ;
#34614 = DIRECTION ( 'NONE',  ( 0.000000000000000000, 0.000000000000000000, -1.000000000000000000 ) ) ;
#34615 = FACE_OUTER_BOUND ( 'NONE', #34440, .T. ) ;
#34616 = ORIENTED_EDGE ( 'NONE', *, *, #381, .F. ) ;
#34617 = ORIENTED_EDGE ( 'NONE', *, *, #13869, .T. ) ;
#34618 = CARTESIAN_POINT ( 'NONE',  ( -500.0000000000000000, -137.0000000000000000, 159.0000000000000000 ) ) ;
#34619 = DIRECTION ( 'NONE',  ( 1.000000000000000000, 0.000000000000000000, 0.000000000000000000 ) ) ;
#34620 = SURFACE_STYLE_USAGE ( .BOTH. , #23005 ) ;
#34621 = FACE_OUTER_BOUND ( 'NONE', #12984, .T. ) ;
#34622 = CARTESIAN_POINT ( 'NONE',  ( 2.123179190381538906, -33.69708579775584667, -36.68877005347592757 ) ) ;
#34623 = ORIENTED_EDGE ( 'NONE', *, *, #968, .T. ) ;
#34624 = AXIS2_PLACEMENT_3D ( 'NONE', #31969, #7940, #7578 ) ;
#34625 = CARTESIAN_POINT ( 'NONE',  ( 8.485274312747499437, 31.41981051364775013, 49.43553178847298568 ) ) ;
#34626 = CARTESIAN_POINT ( 'NONE',  ( 0.07098932002541190334, -18.14847849655012624, -25.98417794693637362 ) ) ;
#34627 = ORIENTED_EDGE ( 'NONE', *, *, #19174, .F. ) ;
#34628 = CARTESIAN_POINT ( 'NONE',  ( -355.0000000000000000, -133.0000000000000000, 126.0000000000000000 ) ) ;
#34629 = DIRECTION ( 'NONE',  ( -1.000000000000000000, 0.000000000000000000, -0.000000000000000000 ) ) ;
#34630 = CARTESIAN_POINT ( 'NONE',  ( 36.10877985260814427, 11.38239727801116352, 68.31122994652405112 ) ) ;
#34631 = ORIENTED_EDGE ( 'NONE', *, *, #19184, .F. ) ;
#34632 = AXIS2_PLACEMENT_3D ( 'NONE', #2393, #24444, #21274 ) ;
#34633 = EDGE_CURVE ( 'NONE', #30712, #22911, #9950, .T. ) ;
#34634 = LINE ( 'NONE', #2400, #25148 ) ;
#34635 = EDGE_LOOP ( 'NONE', ( #5042, #10592, #1458, #29076 ) ) ;
#34636 = EDGE_CURVE ( 'NONE', #19987, #13518, #7087, .T. ) ;
#34637 = PLANE ( 'NONE',  #32006 ) ;
#34638 = ORIENTED_EDGE ( 'NONE', *, *, #8484, .T. ) ;
#34640 = LINE ( 'NONE', #35000, #18558 ) ;
#34639 = LINE ( 'NONE', #12416, #29035 ) ;
#34641 = EDGE_CURVE ( 'NONE', #18838, #11597, #28470, .T. ) ;
#34642 = VECTOR ( 'NONE', #9501, 1000.000000000000000 ) ;
#34643 = ORIENTED_EDGE ( 'NONE', *, *, #8995, .F. ) ;
#34644 =( REPRESENTATION_RELATIONSHIP ('NONE','NONE', #23037, #15767 ) REPRESENTATION_RELATIONSHIP_WITH_TRANSFORMATION ( #28314 )SHAPE_REPRESENTATION_RELATIONSHIP( ) );
#34645 = LINE ( 'NONE', #10254, #27950 ) ;
#34646 = EDGE_CURVE ( 'NONE', #22648, #8601, #34332, .T. ) ;
#34647 = CARTESIAN_POINT ( 'NONE',  ( -26.18205399241665177, -19.33143609808336549, 68.31122994652405112 ) ) ;
#34648 = ORIENTED_EDGE ( 'NONE', *, *, #30583, .T. ) ;
#34649 = VECTOR ( 'NONE', #31321, 1000.000000000000000 ) ;
#34650 = CARTESIAN_POINT ( 'NONE',  ( 760.8419732204888533, 1300.977235064100341, 1753.598338701303419 ) ) ;
#34651 = VERTEX_POINT ( 'NONE', #6391 ) ;
#34652 = CARTESIAN_POINT ( 'NONE',  ( -361.0000000000000000, -135.0000000000000000, 112.0000000000000000 ) ) ;
#34653 = ORIENTED_EDGE ( 'NONE', *, *, #31366, .T. ) ;
#34654 = DIRECTION ( 'NONE',  ( -1.000000000000000000, 0.000000000000000000, 0.000000000000000000 ) ) ;
#34655 = VECTOR ( 'NONE', #8816, 1000.000000000000000 ) ;
#34656 = DIRECTION ( 'NONE',  ( -1.000000000000000000, -0.000000000000000000, -0.000000000000000000 ) ) ;
#34657 = CARTESIAN_POINT ( 'NONE',  ( -105.3523586389574831, -5.105803102660850357, -5.493756281618515480 ) ) ;
#34658 = CARTESIAN_POINT ( 'NONE',  ( 0.02407890056655781832, 31.00221527374952046, -2.344426712874310148 ) ) ;
#34659 = ITEM_DEFINED_TRANSFORMATION ( 'NONE', 'NONE', #766,  #28566 ) ;
#34660 = VERTEX_POINT ( 'NONE', #17472 ) ;
#34661 = VERTEX_POINT ( 'NONE', #22961 ) ;
#34662 = ORIENTED_EDGE ( 'NONE', *, *, #21415, .F. ) ;
#34663 = ADVANCED_FACE ( 'NONE', ( #25793 ), #1242, .T. ) ;
#34664 = DIRECTION ( 'NONE',  ( -0.000000000000000000, -0.000000000000000000, -1.000000000000000000 ) ) ;
#34665 = DIRECTION ( 'NONE',  ( -1.000000000000000000, 0.000000000000000000, 0.000000000000000000 ) ) ;
#34666 = CARTESIAN_POINT ( 'NONE',  ( -20.00000000000004619, 136.9999999999999432, 155.0000000000000000 ) ) ;
#34667 = AXIS2_PLACEMENT_3D ( 'NONE', #25288, #8921, #14280 ) ;
#34668 = DIRECTION ( 'NONE',  ( -1.000000000000000000, 0.000000000000000000, -1.300283923313630633E-47 ) ) ;
#34669 = CARTESIAN_POINT ( 'NONE',  ( 19.99999999999996092, -134.9999999999999716, -162.9999999999999432 ) ) ;
#34670 = ORIENTED_EDGE ( 'NONE', *, *, #9826, .F. ) ;
#34671 = EDGE_CURVE ( 'NONE', #17023, #17068, #20121, .T. ) ;
#34672 = DIRECTION ( 'NONE',  ( 1.000000000000000000, -0.000000000000000000, 0.000000000000000000 ) ) ;
#34673 = LINE ( 'NONE', #12800, #30233 ) ;
#34674 = ADVANCED_FACE ( 'NONE', ( #1760, #12116 ), #31148, .T. ) ;
#34675 = CARTESIAN_POINT ( 'NONE',  ( -418.0000000000000000, 144.9999999999999716, 154.9999999999999716 ) ) ;
#34676 = ORIENTED_EDGE ( 'NONE', *, *, #17822, .T. ) ;
#34677 = EDGE_CURVE ( 'NONE', #19207, #18227, #19456, .T. ) ;
#34678 = CARTESIAN_POINT ( 'NONE',  ( -8.455559046012042135E-14, 30.58763704338517897, -2.144802104989565361 ) ) ;
#34679 = EDGE_LOOP ( 'NONE', ( #29380, #29487, #5958, #31820 ) ) ;
#34680 = LINE ( 'NONE', #17631, #110 ) ;
#34681 = AXIS2_PLACEMENT_3D ( 'NONE', #10347, #26893, #2506 ) ;
#34682 = VERTEX_POINT ( 'NONE', #9610 ) ;
#34683 = DIRECTION ( 'NONE',  ( 0.000000000000000000, 0.000000000000000000, 1.000000000000000000 ) ) ;
#34684 = DIRECTION ( 'NONE',  ( 1.000000000000000000, 0.000000000000000000, 0.000000000000000000 ) ) ;
#34685 = CARTESIAN_POINT ( 'NONE',  ( 9.199999999999999289, 7.794228634059932048, -13.49999999999999822 ) ) ;
#34686 = ORIENTED_EDGE ( 'NONE', *, *, #11551, .T. ) ;
#34687 = VERTEX_POINT ( 'NONE', #6913 ) ;
#34688 = CARTESIAN_POINT ( 'NONE',  ( 761.5335148218593986, 1294.514130222450149, 1753.598338701303646 ) ) ;
#34689 =( REPRESENTATION_RELATIONSHIP ('NONE','NONE', #23037, #28231 ) REPRESENTATION_RELATIONSHIP_WITH_TRANSFORMATION ( #30459 )SHAPE_REPRESENTATION_RELATIONSHIP( ) );
#34690 = VERTEX_POINT ( 'NONE', #1590 ) ;
#34691 = DIRECTION ( 'NONE',  ( 0.000000000000000000, 0.000000000000000000, 1.000000000000000000 ) ) ;
#34692 = SURFACE_SIDE_STYLE ('',( #16544 ) ) ;
#34693 = DIRECTION ( 'NONE',  ( 1.000000000000000000, 0.000000000000000000, 5.546364386991661285E-52 ) ) ;
#34694 = CARTESIAN_POINT ( 'NONE',  ( 101.2263342230664591, -4.337494364694277849, 6.125882734748267389 ) ) ;
#34695 = ITEM_DEFINED_TRANSFORMATION ( 'NONE', 'NONE', #24578,  #28566 ) ;
#34696 = VERTEX_POINT ( 'NONE', #12291 ) ;
#34697 = MANIFOLD_SOLID_BREP ( 'Square tube 40 X 40 X 4(1)[10]', #2561 ) ;
#34698 = DIRECTION ( 'NONE',  ( 1.000000000000000000, 0.000000000000000000, -0.000000000000000000 ) ) ;
#34699 = CIRCLE ( 'NONE', #9140, 1.999999999999999112 ) ;
#34701 = DIRECTION ( 'NONE',  ( -0.9075754196709572286, 0.4198891015602640997, 7.713237663339529843E-17 ) ) ;
#34700 = CARTESIAN_POINT ( 'NONE',  ( -145.0000000000000568, -177.8172209610550851, -45.87893859614474223 ) ) ;
#34702 = VERTEX_POINT ( 'NONE', #14787 ) ;
#34703 = EDGE_LOOP ( 'NONE', ( #33330, #13092, #11721, #9543 ) ) ;
#34704 = LINE ( 'NONE', #2297, #2072 ) ;
#34705 = EDGE_CURVE ( 'NONE', #15586, #24825, #25615, .T. ) ;
#34706 = EDGE_LOOP ( 'NONE', ( #7291, #34994, #30354, #31081, #11832, #34096 ) ) ;
#34707 = EDGE_CURVE ( 'NONE', #22622, #8559, #2936, .T. ) ;
#34708 = CARTESIAN_POINT ( 'NONE',  ( -20.00000000000007461, -113.0000000000000000, -155.0000000000000000 ) ) ;
#34709 = DIRECTION ( 'NONE',  ( 0.000000000000000000, 1.000000000000000000, 5.053935297177146739E-49 ) ) ;
#34710 = ORIENTED_EDGE ( 'NONE', *, *, #19817, .T. ) ;
#34711 = CARTESIAN_POINT ( 'NONE',  ( -361.0000000000000000, -125.0000000000000284, 113.9999999999999858 ) ) ;
#34712 = EDGE_CURVE ( 'NONE', #28310, #2702, #26669, .T. ) ;
#34713 = VECTOR ( 'NONE', #11610, 1000.000000000000000 ) ;
#34714 = AXIS2_PLACEMENT_3D ( 'NONE', #20499, #276, #18370 ) ;
#34715 = DIRECTION ( 'NONE',  ( -1.000000000000000000, -0.000000000000000000, -0.000000000000000000 ) ) ;
#34716 = EDGE_LOOP ( 'NONE', ( #2552, #4759, #31993, #24899 ) ) ;
#34717 = EDGE_CURVE ( 'NONE', #14536, #19390, #33075, .T. ) ;
#34718 = DIRECTION ( 'NONE',  ( 0.000000000000000000, -1.000000000000000000, -1.836970198721029688E-16 ) ) ;
#34719 =( LENGTH_UNIT ( ) NAMED_UNIT ( * ) SI_UNIT ( .MILLI., .METRE. ) );
#34720 = DIRECTION ( 'NONE',  ( 1.000000000000000000, 0.000000000000000000, 0.000000000000000000 ) ) ;
#34722 = DIRECTION ( 'NONE',  ( 0.000000000000000000, -0.9822872507286879440, -0.1873813145857282925 ) ) ;
#34721 = FACE_OUTER_BOUND ( 'NONE', #28788, .T. ) ;
#34723 = DIRECTION ( 'NONE',  ( -0.000000000000000000, 1.000000000000000000, 0.000000000000000000 ) ) ;
#34724 = CARTESIAN_POINT ( 'NONE',  ( 0.02407890056441847060, -0.3931553186915530129, 31.08824725498900321 ) ) ;
#34725 = VECTOR ( 'NONE', #2564, 1000.000000000000000 ) ;
#34726 = CARTESIAN_POINT ( 'NONE',  ( 2.789999999999999147, 17.98401995359667893, -24.59729088254936613 ) ) ;
#34727 = EDGE_CURVE ( 'NONE', #25708, #3173, #21514, .T. ) ;
#34728 = AXIS2_PLACEMENT_3D ( 'NONE', #33207, #25187, #9010 ) ;
#34729 = ORIENTED_EDGE ( 'NONE', *, *, #17932, .F. ) ;
#34730 = CARTESIAN_POINT ( 'NONE',  ( 787.0592847629981179, 1342.348721680649078, 1668.876119909290992 ) ) ;
#34731 = ORIENTED_EDGE ( 'NONE', *, *, #28014, .T. ) ;
#34732 = EDGE_LOOP ( 'NONE', ( #19751, #26671 ) ) ;
#34733 = ADVANCED_BREP_SHAPE_REPRESENTATION ( '', ( #21945, #34697, #22717, #100, #10767, #11835, #12482, #24685, #11234, #22940, #10172, #22535, #34343, #23516, #10344, #34584, #11180, #1117, #28566 ), #4098 ) ;
#34734 = VECTOR ( 'NONE', #26160, 1000.000000000000000 ) ;
#34735 = CARTESIAN_POINT ( 'NONE',  ( -9.978866888775527855, 4.168562732279008642, -87.50000000000000000 ) ) ;
#34736 = DIRECTION ( 'NONE',  ( 0.000000000000000000, 0.000000000000000000, 1.000000000000000000 ) ) ;
#34737 = VECTOR ( 'NONE', #26492, 1000.000000000000000 ) ;
#34738 = ORIENTED_EDGE ( 'NONE', *, *, #28166, .T. ) ;
#34739 = AXIS2_PLACEMENT_3D ( 'NONE', #34103, #15259, #9721 ) ;
#34740 = VERTEX_POINT ( 'NONE', #2633 ) ;
#34741 = CARTESIAN_POINT ( 'NONE',  ( -17.07420202168509604, 33.79163469797343566, -36.68877005347593467 ) ) ;
#34742 = CARTESIAN_POINT ( 'NONE',  ( 0.000000000000000000, 3.524919873834583163E-15, 68.31122994652405112 ) ) ;
#34743 = ITEM_DEFINED_TRANSFORMATION ( 'NONE', 'NONE', #20684,  #28566 ) ;
#34744 = CARTESIAN_POINT ( 'NONE',  ( -11.83261234297099662, -30.31820670846268229, 68.31122994652405112 ) ) ;
#34745 = DIRECTION ( 'NONE',  ( -1.000000000000000000, -0.000000000000000000, -0.000000000000000000 ) ) ;
#34746 = ORIENTED_EDGE ( 'NONE', *, *, #25574, .T. ) ;
#34747 = ORIENTED_EDGE ( 'NONE', *, *, #951, .F. ) ;
#34748 = CARTESIAN_POINT ( 'NONE',  ( 0.000000000000000000, 7.489092610871481703, -29.53582882395380693 ) ) ;
#34750 = DIRECTION ( 'NONE',  ( 1.000000000000000000, 0.000000000000000000, 0.000000000000000000 ) ) ;
#34749 = VECTOR ( 'NONE', #13052, 1000.000000000000000 ) ;
#34751 = EDGE_CURVE ( 'NONE', #10828, #8531, #17760, .T. ) ;
#34752 = CARTESIAN_POINT ( 'NONE',  ( 0.000000000000000000, -23.41952779159748843, -19.49300927180572529 ) ) ;
#34753 = LINE ( 'NONE', #32248, #14833 ) ;
#34754 = PLANE ( 'NONE',  #25645 ) ;
#34755 = ORIENTED_EDGE ( 'NONE', *, *, #19511, .F. ) ;
#34756 = VECTOR ( 'NONE', #21133, 1000.000000000000000 ) ;
#34757 = CARTESIAN_POINT ( 'NONE',  ( 22.89764159710615132, -5.651112684911597128, -77.50000000000000000 ) ) ;
#34758 = LINE ( 'NONE', #7330, #21925 ) ;
#34759 = EDGE_CURVE ( 'NONE', #11327, #20784, #26494, .T. ) ;
#34760 = DIRECTION ( 'NONE',  ( -0.8276889981568906762, 0.5611870653623823868, 1.030883914978406668E-16 ) ) ;
#34761 = DIRECTION ( 'NONE',  ( 0.000000000000000000, 0.000000000000000000, 1.000000000000000000 ) ) ;
#34762 = ADVANCED_FACE ( 'NONE', ( #34507 ), #2279, .F. ) ;
#34763 = CARTESIAN_POINT ( 'NONE',  ( 105.7844661172050991, 5.687621871124707518, -4.888959764314519063 ) ) ;
#34765 = CARTESIAN_POINT ( 'NONE',  ( -106.6936943766627053, 4.837773223901915998, -5.733537676439134145 ) ) ;
#34764 = DIRECTION ( 'NONE',  ( 0.000000000000000000, 0.000000000000000000, -1.000000000000000000 ) ) ;
#34766 = AXIS2_PLACEMENT_3D ( 'NONE', #30280, #14460, #567 ) ;
#34767 = EDGE_CURVE ( 'NONE', #10186, #5671, #2453, .T. ) ;
#34768 = EDGE_CURVE ( 'NONE', #29934, #19057, #27976, .T. ) ;
#34769 = CIRCLE ( 'NONE', #1803, 7.999999999999986677 ) ;
#34770 = DIRECTION ( 'NONE',  ( 0.000000000000000000, 0.000000000000000000, -1.000000000000000000 ) ) ;
#34772 = VERTEX_POINT ( 'NONE', #10124 ) ;
#34771 = CIRCLE ( 'NONE', #31356, 7.999999999999979572 ) ;
#34774 = CIRCLE ( 'NONE', #13181, 1.999999999999999112 ) ;
#34773 = CARTESIAN_POINT ( 'NONE',  ( -15.99999999999998579, -145.0000000000000000, -186.9999999999999716 ) ) ;
#34776 = CARTESIAN_POINT ( 'NONE',  ( 1.039999999999999147, -33.39989884085096605, 8.296590337300141726 ) ) ;
#34775 = DIRECTION ( 'NONE',  ( 3.697785493223492838E-32, 1.934419779023891545E-16, -1.000000000000000000 ) ) ;
#34777 = ORIENTED_EDGE ( 'NONE', *, *, #19098, .T. ) ;
#34778 = SHAPE_REPRESENTATION_RELATIONSHIP ( 'NONE' , 'NONE' ,  #47, #34733 ) ;
#34779 = ORIENTED_EDGE ( 'NONE', *, *, #9542, .T. ) ;
#34780 = ADVANCED_FACE ( 'NONE', ( #18683 ), #31652, .T. ) ;
#34781 = CIRCLE ( 'NONE', #4067, 44.99999999999998579 ) ;
#34782 = ORIENTED_EDGE ( 'NONE', *, *, #7152, .T. ) ;
#34783 = FACE_BOUND ( 'NONE', #34078, .T. ) ;
#34784 = EDGE_LOOP ( 'NONE', ( #26128, #29223, #30652, #10346 ) ) ;
#34785 = ORIENTED_EDGE ( 'NONE', *, *, #25045, .F. ) ;
#34786 = LINE ( 'NONE', #18602, #24700 ) ;
#34787 = VECTOR ( 'NONE', #17639, 1000.000000000000000 ) ;
#34788 = EDGE_CURVE ( 'NONE', #19079, #26414, #21156, .T. ) ;
#34790 = EDGE_CURVE ( 'NONE', #2780, #13396, #5117, .T. ) ;
#34789 = DIRECTION ( 'NONE',  ( -1.000000000000000000, 0.000000000000000000, 1.848892746611746966E-32 ) ) ;
#34791 = AXIS2_PLACEMENT_3D ( 'NONE', #10645, #18498, #7249 ) ;
#34792 = DIRECTION ( 'NONE',  ( -0.000000000000000000, -0.000000000000000000, -1.000000000000000000 ) ) ;
#34793 = ORIENTED_EDGE ( 'NONE', *, *, #5518, .T. ) ;
#34794 = ORIENTED_EDGE ( 'NONE', *, *, #13867, .T. ) ;
#34795 = AXIS2_PLACEMENT_3D ( 'NONE', #16668, #27674, #3112 ) ;
#34796 = DIRECTION ( 'NONE',  ( -0.000000000000000000, 0.08715574274766170471, 0.9961946980917453232 ) ) ;
#34797 = CARTESIAN_POINT ( 'NONE',  ( 24.90835164106607280, -28.52396285516520891, 68.31122994652405112 ) ) ;
#34798 = AXIS2_PLACEMENT_3D ( 'NONE', #34501, #34324, #28463 ) ;
#34799 = LINE ( 'NONE', #13089, #12419 ) ;
#34800 = LINE ( 'NONE', #10406, #31235 ) ;
#34801 = CARTESIAN_POINT ( 'NONE',  ( -445.9999999999999432, -105.0000000000000142, 107.9999999999999858 ) ) ;
#34802 = ORIENTED_EDGE ( 'NONE', *, *, #4112, .F. ) ;
#34803 = CARTESIAN_POINT ( 'NONE',  ( -345.0000000000000000, 134.9999999999999716, 126.0000000000000000 ) ) ;
#34804 = DIRECTION ( 'NONE',  ( 0.000000000000000000, 0.000000000000000000, -1.000000000000000000 ) ) ;
#34805 = VERTEX_POINT ( 'NONE', #7616 ) ;
#34806 = FACE_OUTER_BOUND ( 'NONE', #12767, .T. ) ;
#34807 = DIRECTION ( 'NONE',  ( 0.000000000000000000, -0.7705132427757861446, -0.6374239897486932982 ) ) ;
#34808 = LINE ( 'NONE', #12282, #19744 ) ;
#34809 = VERTEX_POINT ( 'NONE', #29350 ) ;
#34810 = CARTESIAN_POINT ( 'NONE',  ( 12.00000000000001066, -60.99999999999997158, 154.9999999999999716 ) ) ;
#34811 = ORIENTED_EDGE ( 'NONE', *, *, #3324, .T. ) ;
#34812 = ADVANCED_FACE ( 'NONE', ( #13336 ), #4946, .T. ) ;
#34813 = ADVANCED_FACE ( 'NONE', ( #13157 ), #10483, .F. ) ;
#34814 = LINE ( 'NONE', #20759, #21216 ) ;
#34815 = CLOSED_SHELL ( 'NONE', ( #31937, #13035, #7493, #23229, #14079, #31575, #2318, #32571, #7996, #10860, #33760, #35082, #12948, #23944, #2080, #1746, #35043, #7991 ) ) ;
#34816 = ORIENTED_EDGE ( 'NONE', *, *, #31983, .F. ) ;
#34818 = LINE ( 'NONE', #10076, #8313 ) ;
#34817 = FILL_AREA_STYLE ('',( #21630 ) ) ;
#34819 = DIRECTION ( 'NONE',  ( 1.000000000000000000, -0.000000000000000000, -0.000000000000000000 ) ) ;
#34820 = CIRCLE ( 'NONE', #31952, 2.033421858999711507 ) ;
#34821 = B_SPLINE_CURVE_WITH_KNOTS ( 'NONE', 3,
 ( #25921, #1871, #15422, #34097, #6857, #22902 ),
 .UNSPECIFIED., .F., .F.,
 ( 4, 2, 4 ),
 ( 4.404817002564676105E-07, 0.001874269606309968183, 0.003748098730919679870 ),
 .UNSPECIFIED. ) ;
#34823 = EDGE_LOOP ( 'NONE', ( #24017, #526, #6499, #17716 ) ) ;
#34822 = VECTOR ( 'NONE', #33891, 1000.000000000000000 ) ;
#34824 = AXIS2_PLACEMENT_3D ( 'NONE', #29069, #26402, #34067 ) ;
#34825 = VECTOR ( 'NONE', #20584, 1000.000000000000000 ) ;
#34826 = DIRECTION ( 'NONE',  ( 0.2149704402110242940, -0.9766205557100865464, 0.000000000000000000 ) ) ;
#34827 = CARTESIAN_POINT ( 'NONE',  ( -414.0000000000000568, 113.0000000000000000, -175.0000000000000000 ) ) ;
#34828 = ORIENTED_EDGE ( 'NONE', *, *, #13691, .T. ) ;
#34829 = DIRECTION ( 'NONE',  ( -0.1063910735369225230, 0.9943243633099118073, -1.000770725407345128E-14 ) ) ;
#34830 = ORIENTED_EDGE ( 'NONE', *, *, #10566, .F. ) ;
#34831 = DIRECTION ( 'NONE',  ( -0.000000000000000000, -1.000000000000000000, -0.000000000000000000 ) ) ;
#34832 = ORIENTED_EDGE ( 'NONE', *, *, #25835, .F. ) ;
#34833 = DIRECTION ( 'NONE',  ( 1.000000000000000000, 0.000000000000000000, 0.000000000000000000 ) ) ;
#34834 = EDGE_CURVE ( 'NONE', #14276, #16070, #4763, .T. ) ;
#34835 = EDGE_CURVE ( 'NONE', #27012, #4827, #697, .T. ) ;
#34836 = DIRECTION ( 'NONE',  ( 0.000000000000000000, -1.000000000000000000, -1.310824597558155437E-49 ) ) ;
#34837 = EDGE_CURVE ( 'NONE', #34245, #13771, #27022, .T. ) ;
#34838 = CARTESIAN_POINT ( 'NONE',  ( -102.4139082377428451, -4.424982940199789105, -6.059505149883824160 ) ) ;
#34839 = DIRECTION ( 'NONE',  ( 1.300283923313630633E-47, 0.000000000000000000, -1.000000000000000000 ) ) ;
#34840 = CONTEXT_DEPENDENT_SHAPE_REPRESENTATION ( #3293, #23129 ) ;
#34841 = EDGE_LOOP ( 'NONE', ( #6811, #3043, #31576, #16535 ) ) ;
#34842 = ORIENTED_EDGE ( 'NONE', *, *, #3243, .T. ) ;
#34843 = EDGE_LOOP ( 'NONE', ( #32144, #27081, #11254, #10042 ) ) ;
#34844 = LINE ( 'NONE', #2605, #22485 ) ;
#34845 = LINE ( 'NONE', #2954, #31666 ) ;
#34846 = EDGE_CURVE ( 'NONE', #24518, #32005, #21852, .T. ) ;
#34847 = DIRECTION ( 'NONE',  ( 0.000000000000000000, -1.000000000000000000, -2.465190328815662439E-32 ) ) ;
#34848 = AXIS2_PLACEMENT_3D ( 'NONE', #9080, #3901, #9954 ) ;
#34850 = ADVANCED_FACE ( 'NONE', ( #8503 ), #19552, .T. ) ;
#34849 = CARTESIAN_POINT ( 'NONE',  ( 1.532562817202168137, 32.50931595846692801, -36.68877005347593467 ) ) ;
#34851 = DIRECTION ( 'NONE',  ( -0.8276889981568904542, -0.5611870653623824978, 0.000000000000000000 ) ) ;
#34852 = AXIS2_PLACEMENT_3D ( 'NONE', #10514, #21371, #16038 ) ;
#34853 = AXIS2_PLACEMENT_3D ( 'NONE', #7659, #4808, #27061 ) ;
#34854 = DIRECTION ( 'NONE',  ( -1.000000000000000000, -0.000000000000000000, -0.000000000000000000 ) ) ;
#34855 = AXIS2_PLACEMENT_3D ( 'NONE', #32429, #8047, #24243 ) ;
#34856 = CARTESIAN_POINT ( 'NONE',  ( -442.0000000000000000, -141.0000000000000000, -175.0000000000000000 ) ) ;
#34857 = ORIENTED_EDGE ( 'NONE', *, *, #17901, .F. ) ;
#34858 = LINE ( 'NONE', #19014, #33308 ) ;
#34859 = CARTESIAN_POINT ( 'NONE',  ( 0.006871268844553799111, -30.26101440722787217, 6.099076262612395993 ) ) ;
#34860 = DIRECTION ( 'NONE',  ( -0.000000000000000000, 1.836970198721029934E-16, -1.000000000000000000 ) ) ;
#34861 = ORIENTED_EDGE ( 'NONE', *, *, #11177, .T. ) ;
#34862 = EDGE_CURVE ( 'NONE', #22788, #2604, #14395, .T. ) ;
#34863 = FACE_BOUND ( 'NONE', #12808, .T. ) ;
#34864 = VERTEX_POINT ( 'NONE', #6171 ) ;
#34865 = CARTESIAN_POINT ( 'NONE',  ( 2.789999999999999147, 29.94779062842794559, -5.619744560738758388 ) ) ;
#34866 = DIRECTION ( 'NONE',  ( 0.9766205557100866574, -0.2149704402110243773, -3.948942922735927635E-17 ) ) ;
#34867 = VECTOR ( 'NONE', #29814, 1000.000000000000000 ) ;
#34868 = ORIENTED_EDGE ( 'NONE', *, *, #2870, .T. ) ;
#34869 = FACE_OUTER_BOUND ( 'NONE', #17992, .T. ) ;
#34870 = LINE ( 'NONE', #18512, #27013 ) ;
#34871 = CARTESIAN_POINT ( 'NONE',  ( 0.000000000000000000, -33.69708579775584667, 49.43553178847298568 ) ) ;
#34872 = ORIENTED_EDGE ( 'NONE', *, *, #15465, .T. ) ;
#34873 = AXIS2_PLACEMENT_3D ( 'NONE', #334, #2982, #11192 ) ;
#34874 = ORIENTED_EDGE ( 'NONE', *, *, #20443, .T. ) ;
#34875 = CIRCLE ( 'NONE', #6976, 2.525000000000000799 ) ;
#34876 = CARTESIAN_POINT ( 'NONE',  ( 765.6827644300816473, 1255.735501172547174, 1753.598338701303646 ) ) ;
#34877 = AXIS2_PLACEMENT_3D ( 'NONE', #31178, #34720, #10158 ) ;
#34878 = VERTEX_POINT ( 'NONE', #16533 ) ;
#34879 = CARTESIAN_POINT ( 'NONE',  ( -5.021133111224782120, 14.09580098603202458, -67.50000000000000000 ) ) ;
#34880 = EDGE_CURVE ( 'NONE', #32120, #34561, #32708, .T. ) ;
#34882 = EDGE_CURVE ( 'NONE', #17435, #30812, #10908, .T. ) ;
#34881 = B_SPLINE_CURVE_WITH_KNOTS ( 'NONE', 3,
 ( #29475, #10426, #13286, #8096 ),
 .UNSPECIFIED., .F., .F.,
 ( 4, 4 ),
 ( 0.005298517298376327969, 0.005985383706685561134 ),
 .UNSPECIFIED. ) ;
#34883 = CARTESIAN_POINT ( 'NONE',  ( -410.0000000000000568, -104.9999999999999005, -77.99999999999997158 ) ) ;
#34884 = FACE_BOUND ( 'NONE', #5661, .T. ) ;
#34885 = ORIENTED_EDGE ( 'NONE', *, *, #26670, .T. ) ;
#34886 = DIRECTION ( 'NONE',  ( 0.000000000000000000, -1.000000000000000000, -2.465190328815662439E-32 ) ) ;
#34887 = AXIS2_PLACEMENT_3D ( 'NONE', #32713, #2983, #32885 ) ;
#34889 = CARTESIAN_POINT ( 'NONE',  ( 2.765921099433443775, -11.07880054387241664, 29.04985141099759360 ) ) ;
#34888 = CARTESIAN_POINT ( 'NONE',  ( -23.93921925319781963, 29.33115633223345142, 68.31122994652405112 ) ) ;
#34890 = EDGE_LOOP ( 'NONE', ( #34604, #26195, #34874, #6519 ) ) ;
#34891 = ORIENTED_EDGE ( 'NONE', *, *, #8634, .F. ) ;
#34892 = CARTESIAN_POINT ( 'NONE',  ( 0.1859802827496877808, 4.859980099383433227, 31.91379830674626206 ) ) ;
#34893 = ORIENTED_EDGE ( 'NONE', *, *, #20893, .T. ) ;
#34894 = CARTESIAN_POINT ( 'NONE',  ( -361.0000000000000000, -125.0000000000000284, 166.9999999999999716 ) ) ;
#34895 = CARTESIAN_POINT ( 'NONE',  ( -349.0000000000000000, -125.0000000000000284, 109.9999999999999858 ) ) ;
#34896 = EDGE_LOOP ( 'NONE', ( #9352, #32315, #4339, #19844, #20272, #10227 ) ) ;
#34897 = DIRECTION ( 'NONE',  ( 0.000000000000000000, -0.5000000000000012212, -0.8660254037844380415 ) ) ;
#34898 = CIRCLE ( 'NONE', #16715, 32.54542015209055705 ) ;
#34899 = AXIS2_PLACEMENT_3D ( 'NONE', #34540, #26003, #23506 ) ;
#34900 = PRODUCT_DEFINITION_SHAPE ( 'NONE', 'NONE',  #35239 ) ;
#34901 = DIRECTION ( 'NONE',  ( 0.000000000000000000, 0.000000000000000000, 1.000000000000000000 ) ) ;
#34902 = ORIENTED_EDGE ( 'NONE', *, *, #20295, .F. ) ;
#34903 = FACE_OUTER_BOUND ( 'NONE', #31913, .T. ) ;
#34904 = DIRECTION ( 'NONE',  ( 1.000000000000000000, 3.040835319149746090E-31, 1.232595164407830946E-32 ) ) ;
#34905 = DIRECTION ( 'NONE',  ( 0.000000000000000000, 0.000000000000000000, 1.000000000000000000 ) ) ;
#34907 = DIRECTION ( 'NONE',  ( 0.000000000000000000, 1.000000000000000000, 5.053935297177146739E-49 ) ) ;
#34906 = CARTESIAN_POINT ( 'NONE',  ( 15.99999999999998579, 4.559999999999908127, -172.9900000000000091 ) ) ;
#34908 =( REPRESENTATION_RELATIONSHIP ('NONE','NONE', #23037, #15767 ) REPRESENTATION_RELATIONSHIP_WITH_TRANSFORMATION ( #33598 )SHAPE_REPRESENTATION_RELATIONSHIP( ) );
#34909 = LINE ( 'NONE', #6955, #25068 ) ;
#34910 = DIRECTION ( 'NONE',  ( 0.000000000000000000, 0.000000000000000000, -1.000000000000000000 ) ) ;
#34911 = DIRECTION ( 'NONE',  ( 0.000000000000000000, 0.000000000000000000, 1.000000000000000000 ) ) ;
#34912 = VECTOR ( 'NONE', #12082, 1000.000000000000000 ) ;
#34913 = VERTEX_POINT ( 'NONE', #25036 ) ;
#34914 = CARTESIAN_POINT ( 'NONE',  ( 2.289514115302874409, 0.9548574718894666802, -11.96154122019908783 ) ) ;
#34915 = CARTESIAN_POINT ( 'NONE',  ( 824.2973882641603041, 1280.728782669502607, 1753.598338701302964 ) ) ;
#34916 = PRODUCT_DEFINITION_CONTEXT ( 'detailed design', #15794, 'design' ) ;
#34917 = ORIENTED_EDGE ( 'NONE', *, *, #18898, .T. ) ;
#34918 = VECTOR ( 'NONE', #1605, 1000.000000000000000 ) ;
#34919 = ORIENTED_EDGE ( 'NONE', *, *, #23046, .T. ) ;
#34920 = ADVANCED_FACE ( 'NONE', ( #24688 ), #504, .F. ) ;
#34921 = VERTEX_POINT ( 'NONE', #11719 ) ;
#34922 = EDGE_CURVE ( 'NONE', #22339, #26155, #24506, .T. ) ;
#34923 = CARTESIAN_POINT ( 'NONE',  ( 109.9370925636957139, 2.947297676519624599, 6.904853577595275738 ) ) ;
#34924 = DIRECTION ( 'NONE',  ( 0.6153844916016690814, 0.7882270786367058246, 9.094875506676379127E-15 ) ) ;
#34925 = VECTOR ( 'NONE', #12976, 1000.000000000000000 ) ;
#34926 = ORIENTED_EDGE ( 'NONE', *, *, #12607, .F. ) ;
#34927 = EDGE_CURVE ( 'NONE', #14045, #35, #8327, .T. ) ;
#34928 = DIRECTION ( 'NONE',  ( 0.000000000000000000, 0.000000000000000000, 1.000000000000000000 ) ) ;
#34929 = LINE ( 'NONE', #25723, #13034 ) ;
#34930 = AXIS2_PLACEMENT_3D ( 'NONE', #32965, #27466, #3077 ) ;
#34931 = LINE ( 'NONE', #20516, #14150 ) ;
#34932 = EDGE_LOOP ( 'NONE', ( #20045, #20053, #1160, #12934 ) ) ;
#34933 = ORIENTED_EDGE ( 'NONE', *, *, #22548, .F. ) ;
#34934 = CARTESIAN_POINT ( 'NONE',  ( 0.006871323915374539550, 4.186936631162940792, 30.58426604563496909 ) ) ;
#34935 = DIRECTION ( 'NONE',  ( -0.000000000000000000, -0.000000000000000000, 1.000000000000000000 ) ) ;
#34936 = B_SPLINE_CURVE_WITH_KNOTS ( 'NONE', 3,
 ( #7614, #21154, #17804, #34505 ),
 .UNSPECIFIED., .F., .F.,
 ( 4, 4 ),
 ( 0.005298458409503519449, 0.005985325590332028593 ),
 .UNSPECIFIED. ) ;
#34937 = CARTESIAN_POINT ( 'NONE',  ( -430.0000000000000000, -133.0000000000000000, 113.9999999999999858 ) ) ;
#34938 = PLANE ( 'NONE',  #19959 ) ;
#34939 = CARTESIAN_POINT ( 'NONE',  ( 1.749999999999999778, -33.39989884085096605, 8.296590337300138174 ) ) ;
#34940 = ORIENTED_EDGE ( 'NONE', *, *, #34862, .T. ) ;
#34941 = CARTESIAN_POINT ( 'NONE',  ( -20.02113311122498729, -3.725253662474300231, -87.50000000000000000 ) ) ;
#34942 = CARTESIAN_POINT ( 'NONE',  ( -442.0000000000000000, -137.0000000000000000, -175.0000000000000000 ) ) ;
#34943 = CIRCLE ( 'NONE', #25829, 3.999999999999976019 ) ;
#34944 = CARTESIAN_POINT ( 'NONE',  ( -361.0000000000000000, -125.0000000000000284, 164.9999999999999716 ) ) ;
#34945 = CARTESIAN_POINT ( 'NONE',  ( 12.00000000000001066, -134.9999999999999716, 162.9999999999999716 ) ) ;
#34946 = FACE_OUTER_BOUND ( 'NONE', #31378, .T. ) ;
#34947 = EDGE_LOOP ( 'NONE', ( #30325, #17936, #10793, #13460 ) ) ;
#34948 = CARTESIAN_POINT ( 'NONE',  ( -418.0000000000000000, 144.9999999999999716, -155.0000000000000000 ) ) ;
#34950 = LINE ( 'NONE', #21938, #16261 ) ;
#34949 = CARTESIAN_POINT ( 'NONE',  ( -35.00000000000000000, 0.000000000000000000, 0.000000000000000000 ) ) ;
#34951 = DIRECTION ( 'NONE',  ( 1.000000000000000000, 0.000000000000000000, -1.232595164407831220E-32 ) ) ;
#34952 = ORIENTED_EDGE ( 'NONE', *, *, #15125, .T. ) ;
#34953 = CARTESIAN_POINT ( 'NONE',  ( 103.6817977190026454, 5.587831648195836998, -11.18158713856774611 ) ) ;
#34955 = CARTESIAN_POINT ( 'NONE',  ( -1.625000000000000000, 2.702098422956710877, 3.180000000000000160 ) ) ;
#34954 = PLANE ( 'NONE',  #17790 ) ;
#34956 = VECTOR ( 'NONE', #19562, 1000.000000000000000 ) ;
#34957 = EDGE_LOOP ( 'NONE', ( #13066, #1369, #21972, #9700, #19408, #4192, #32851, #1514 ) ) ;
#34958 = CARTESIAN_POINT ( 'NONE',  ( -8.256681647508496812E-14, -11.08290750743005226, 28.58973358960017919 ) ) ;
#34959 = VERTEX_POINT ( 'NONE', #21677 ) ;
#34960 = EDGE_CURVE ( 'NONE', #2214, #17376, #27544, .T. ) ;
#34961 = AXIS2_PLACEMENT_3D ( 'NONE', #6444, #20348, #1471 ) ;
#34962 = ORIENTED_EDGE ( 'NONE', *, *, #26801, .F. ) ;
#34963 = FACE_BOUND ( 'NONE', #19028, .T. ) ;
#34964 = ORIENTED_EDGE ( 'NONE', *, *, #33278, .T. ) ;
#34965 = ORIENTED_EDGE ( 'NONE', *, *, #22304, .F. ) ;
#34966 = EDGE_CURVE ( 'NONE', #20509, #4608, #677, .T. ) ;
#34967 = DIRECTION ( 'NONE',  ( -1.000000000000000000, -0.000000000000000000, -0.000000000000000000 ) ) ;
#34968 = VECTOR ( 'NONE', #32544, 1000.000000000000114 ) ;
#34969 = ADVANCED_FACE ( 'NONE', ( #5472 ), #27892, .T. ) ;
#34970 = EDGE_CURVE ( 'NONE', #30812, #23243, #27995, .T. ) ;
#34971 = VECTOR ( 'NONE', #20156, 1000.000000000000000 ) ;
#34972 = DIRECTION ( 'NONE',  ( -0.6876994588534233177, 0.7259954919231308423, -0.000000000000000000 ) ) ;
#34973 = CARTESIAN_POINT ( 'NONE',  ( -20.72055270933793736, 25.09707290294331017, -36.68877005347593467 ) ) ;
#34974 = EDGE_CURVE ( 'NONE', #14584, #31542, #34820, .T. ) ;
#34975 = ORIENTED_EDGE ( 'NONE', *, *, #20454, .F. ) ;
#34976 = ADVANCED_FACE ( 'NONE', ( #30399 ), #27722, .T. ) ;
#34977 = EDGE_LOOP ( 'NONE', ( #17956, #26204, #28305, #20734 ) ) ;
#34978 = VECTOR ( 'NONE', #11583, 1000.000000000000000 ) ;
#34979 = DIRECTION ( 'NONE',  ( 0.000000000000000000, 0.000000000000000000, 1.000000000000000000 ) ) ;
#34980 = CARTESIAN_POINT ( 'NONE',  ( 0.000000000000000000, 0.000000000000000000, 0.000000000000000000 ) ) ;
#34981 = VECTOR ( 'NONE', #9150, 1000.000000000000000 ) ;
#34982 = EDGE_CURVE ( 'NONE', #10479, #18486, #11188, .T. ) ;
#34983 = CARTESIAN_POINT ( 'NONE',  ( -4.875000000000000000, -1.866624223957557671, 0.000000000000000000 ) ) ;
#34984 = FACE_OUTER_BOUND ( 'NONE', #358, .T. ) ;
#34985 = VERTEX_POINT ( 'NONE', #5994 ) ;
#34986 = LINE ( 'NONE', #10599, #16253 ) ;
#34987 = CARTESIAN_POINT ( 'NONE',  ( 0.000000000000000000, 23.28319895603578971, 21.86437915510226659 ) ) ;
#34988 = ORIENTED_EDGE ( 'NONE', *, *, #1886, .T. ) ;
#34989 = LINE ( 'NONE', #12929, #11756 ) ;
#34990 = CARTESIAN_POINT ( 'NONE',  ( 212.5000000000000000, 0.000000000000000000, 0.000000000000000000 ) ) ;
#34991 = CYLINDRICAL_SURFACE ( 'NONE', #13485, 7.999999999999986677 ) ;
#34992 = ORIENTED_EDGE ( 'NONE', *, *, #31149, .T. ) ;
#34993 = LINE ( 'NONE', #20928, #34825 ) ;
#34994 = ORIENTED_EDGE ( 'NONE', *, *, #4490, .F. ) ;
#34995 = CIRCLE ( 'NONE', #2577, 30.47050528711511674 ) ;
#34996 = AXIS2_PLACEMENT_3D ( 'NONE', #12528, #17887, #7161 ) ;
#34997 = CARTESIAN_POINT ( 'NONE',  ( 2.765921099433442443, 29.44518845714779332, -9.980709654879110104 ) ) ;
#34998 = ORIENTED_EDGE ( 'NONE', *, *, #25302, .F. ) ;
#35000 = CARTESIAN_POINT ( 'NONE',  ( -23.78520691327551262, 22.21414650552150505, -36.68877005347593467 ) ) ;
#34999 = SURFACE_SIDE_STYLE ('',( #26972 ) ) ;
#35001 = AXIS2_PLACEMENT_3D ( 'NONE', #33217, #33394, #19886 ) ;
#35002 = CARTESIAN_POINT ( 'NONE',  ( 2.789999999999999147, -30.41598411195407081, -1.821977758773984490 ) ) ;
#35003 = ORIENTED_EDGE ( 'NONE', *, *, #3548, .F. ) ;
#35004 = CARTESIAN_POINT ( 'NONE',  ( 28.23027531293552528, -10.15143121711728469, 20.00000000000000000 ) ) ;
#35005 = CARTESIAN_POINT ( 'NONE',  ( -361.0000000000000000, 134.9999999999999716, 113.9999999999999858 ) ) ;
#35006 = AXIS2_PLACEMENT_3D ( 'NONE', #8226, #29952, #19283 ) ;
#35007 = EDGE_LOOP ( 'NONE', ( #11285, #9495, #30463, #1061 ) ) ;
#35008 = DIRECTION ( 'NONE',  ( 0.2332500902972249601, 0.9724167806945416270, -1.059241111688404545E-15 ) ) ;
#35009 = VERTEX_POINT ( 'NONE', #3336 ) ;
#35010 = CARTESIAN_POINT ( 'NONE',  ( -19.99999999999998934, 124.9999999999999716, 162.9999999999999716 ) ) ;
#35011 = ORIENTED_EDGE ( 'NONE', *, *, #15889, .F. ) ;
#35012 = CARTESIAN_POINT ( 'NONE',  ( -410.0000000000000568, -137.0000000000000000, -155.0000000000000000 ) ) ;
#35013 = ADVANCED_FACE ( 'NONE', ( #30576 ), #11539, .T. ) ;
#35014 = DIRECTION ( 'NONE',  ( 1.000000000000000000, 0.000000000000000000, 0.000000000000000000 ) ) ;
#35015 = CIRCLE ( 'NONE', #30460, 2.033421858999711507 ) ;
#35016 = CARTESIAN_POINT ( 'NONE',  ( -109.5736443501088928, -2.314419832420933520, -7.141071956987316227 ) ) ;
#35017 = CARTESIAN_POINT ( 'NONE',  ( 0.000000000000000000, 3.214697847761802057E-14, -87.50000000000000000 ) ) ;
#35018 = EDGE_CURVE ( 'NONE', #19221, #2759, #33471, .T. ) ;
#35019 = ORIENTED_EDGE ( 'NONE', *, *, #24005, .T. ) ;
#35020 = EDGE_CURVE ( 'NONE', #10968, #1533, #8147, .T. ) ;
#35021 = ORIENTED_EDGE ( 'NONE', *, *, #11984, .F. ) ;
#35022 = ORIENTED_EDGE ( 'NONE', *, *, #33017, .F. ) ;
#35023 = DIRECTION ( 'NONE',  ( 0.000000000000000000, 0.000000000000000000, 1.000000000000000000 ) ) ;
#35024 = DIRECTION ( 'NONE',  ( -0.3701381553399156199, -0.9289767198167909745, -1.706502549609061002E-16 ) ) ;
#35025 = VECTOR ( 'NONE', #15733, 1000.000000000000000 ) ;
#35026 = CARTESIAN_POINT ( 'NONE',  ( 11.99999999999999645, 144.9999999999999147, 155.0000000000000000 ) ) ;
#35027 = DIRECTION ( 'NONE',  ( -1.000000000000000000, 0.000000000000000000, 0.000000000000000000 ) ) ;
#35028 = DIRECTION ( 'NONE',  ( 0.000000000000000000, -1.000000000000000000, -1.836970198721029934E-16 ) ) ;
#35029 = CARTESIAN_POINT ( 'NONE',  ( 11.99999999999999645, -24.99999999999999289, 154.9999999999999716 ) ) ;
#35030 = CARTESIAN_POINT ( 'NONE',  ( -70.00000000000000000, 4.559999999999909015, 177.7400000000000091 ) ) ;
#35031 = ORIENTED_EDGE ( 'NONE', *, *, #21992, .T. ) ;
#35032 = AXIS2_PLACEMENT_3D ( 'NONE', #32918, #20420, #3197 ) ;
#35033 = CARTESIAN_POINT ( 'NONE',  ( 3.235562306570555532E-30, 14.09580098603202458, -67.50000000000000000 ) ) ;
#35034 = CYLINDRICAL_SURFACE ( 'NONE', #102, 16.19999999999999574 ) ;
#35035 = ADVANCED_FACE ( 'NONE', ( #6350 ), #20255, .T. ) ;
#35036 = CARTESIAN_POINT ( 'NONE',  ( 2.261199741286049836, 30.75271593550620608, -13.00575455800169955 ) ) ;
#35037 = ORIENTED_EDGE ( 'NONE', *, *, #33619, .F. ) ;
#35038 = CARTESIAN_POINT ( 'NONE',  ( 18.63894936814906345, 26.67946662374789213, 68.31122994652405112 ) ) ;
#35039 = VERTEX_POINT ( 'NONE', #9034 ) ;
#35040 = CARTESIAN_POINT ( 'NONE',  ( -104.6652972762545062, 5.115232524641492695, -11.40545467192879592 ) ) ;
#35041 = EDGE_CURVE ( 'NONE', #12488, #18684, #720, .T. ) ;
#35042 = CARTESIAN_POINT ( 'NONE',  ( -418.0000000000000000, -125.0000000000000000, 187.0000000000000000 ) ) ;
#35043 = ADVANCED_FACE ( 'NONE', ( #12903, #20896 ), #28255, .T. ) ;
#35044 = ORIENTED_EDGE ( 'NONE', *, *, #22865, .F. ) ;
#35045 = LINE ( 'NONE', #32183, #24502 ) ;
#35046 = CARTESIAN_POINT ( 'NONE',  ( -143.0000000000000568, -45.49999999999999289, 63.00000000000000000 ) ) ;
#35047 = DIRECTION ( 'NONE',  ( 0.000000000000000000, 0.000000000000000000, -1.000000000000000000 ) ) ;
#35048 = AXIS2_PLACEMENT_3D ( 'NONE', #19190, #15642, #2100 ) ;
#35049 = EDGE_CURVE ( 'NONE', #7313, #12505, #11523, .T. ) ;
#35050 = ORIENTED_EDGE ( 'NONE', *, *, #2197, .T. ) ;
#35051 = EDGE_LOOP ( 'NONE', ( #6451, #9944, #3076, #1509 ) ) ;
#35052 = DIRECTION ( 'NONE',  ( -0.1063910735369017202, 0.9943243633099136947, -1.000770725407181676E-14 ) ) ;
#35053 = PLANE ( 'NONE',  #34319 ) ;
#35054 = ORIENTED_EDGE ( 'NONE', *, *, #6166, .T. ) ;
#35055 = AXIS2_PLACEMENT_3D ( 'NONE', #14873, #25527, #20210 ) ;
#35056 = CARTESIAN_POINT ( 'NONE',  ( 0.02407890056655738464, 24.20451283648857554, -19.51346322004903300 ) ) ;
#35057 = LINE ( 'NONE', #13681, #13564 ) ;
#35058 = CARTESIAN_POINT ( 'NONE',  ( 5.917509466954039044E-05, -25.81864426690146885, -16.24881338200996694 ) ) ;
#35059 = CARTESIAN_POINT ( 'NONE',  ( -41.91829877876165256, 16.36631389076590892, -36.69130526491316857 ) ) ;
#35060 = ITEM_DEFINED_TRANSFORMATION ( 'NONE', 'NONE', #6973,  #28566 ) ;
#35061 = EDGE_CURVE ( 'NONE', #29588, #16280, #19905, .T. ) ;
#35062 = VERTEX_POINT ( 'NONE', #9211 ) ;
#35063 = CARTESIAN_POINT ( 'NONE',  ( 10.00000000000000000, 0.000000000000000000, 0.000000000000000000 ) ) ;
#35064 = AXIS2_PLACEMENT_3D ( 'NONE', #25642, #1271, #3403 ) ;
#35065 = AXIS2_PLACEMENT_3D ( 'NONE', #12448, #8877, #1399 ) ;
#35067 = CARTESIAN_POINT ( 'NONE',  ( -10.00000000000000000, 3.520859547548641820E-15, 47.49999999999999289 ) ) ;
#35066 = DIRECTION ( 'NONE',  ( 0.000000000000000000, 0.000000000000000000, -1.000000000000000000 ) ) ;
#35068 = EDGE_LOOP ( 'NONE', ( #15215, #4888, #3916, #563 ) ) ;
#35069 = VERTEX_POINT ( 'NONE', #30746 ) ;
#35070 = DIRECTION ( 'NONE',  ( -0.6473862847818285804, 0.7621620551276356847, -0.000000000000000000 ) ) ;
#35071 = ORIENTED_EDGE ( 'NONE', *, *, #20376, .T. ) ;
#35072 = CARTESIAN_POINT ( 'NONE',  ( -430.0000000000000000, -131.0000000000000000, 126.0000000000000000 ) ) ;
#35073 = CARTESIAN_POINT ( 'NONE',  ( 0.000000000000000000, 7.489092610871481703, -29.53582882395380693 ) ) ;
#35074 = ORIENTED_EDGE ( 'NONE', *, *, #40, .T. ) ;
#35075 = VERTEX_POINT ( 'NONE', #22917 ) ;
#35076 = CARTESIAN_POINT ( 'NONE',  ( 1.749999999999999778, 0.000000000000000000, 0.000000000000000000 ) ) ;
#35077 = PLANE ( 'NONE',  #1303 ) ;
#35078 = ORIENTED_EDGE ( 'NONE', *, *, #31078, .T. ) ;
#35079 = PLANE ( 'NONE',  #18083 ) ;
#35080 = FACE_OUTER_BOUND ( 'NONE', #27853, .T. ) ;
#35081 = CARTESIAN_POINT ( 'NONE',  ( 12.73347502555019872, -33.69708579775584667, -36.68877005347592757 ) ) ;
#35082 = ADVANCED_FACE ( 'NONE', ( #14569 ), #25398, .T. ) ;
#35083 = DIRECTION ( 'NONE',  ( 1.000000000000000000, 3.040835319149746090E-31, 1.232595164407830946E-32 ) ) ;
#35084 = EDGE_CURVE ( 'NONE', #10220, #14310, #31741, .T. ) ;
#35085 = CARTESIAN_POINT ( 'NONE',  ( 1.394999999999999574, 14.40815186467820475, -31.25366880301303496 ) ) ;
#35086 = CARTESIAN_POINT ( 'NONE',  ( -32.32899628990712415, -3.747048406849366131, 68.31122994652405112 ) ) ;
#35087 = DIRECTION ( 'NONE',  ( -1.000000000000000000, 0.000000000000000000, 0.000000000000000000 ) ) ;
#35088 = AXIS2_PLACEMENT_3D ( 'NONE', #18271, #29635, #18793 ) ;
#35089 = VECTOR ( 'NONE', #24056, 1000.000000000000000 ) ;
#35090 = VECTOR ( 'NONE', #11263, 1000.000000000000000 ) ;
#35091 = VERTEX_POINT ( 'NONE', #11897 ) ;
#35092 = CARTESIAN_POINT ( 'NONE',  ( 2.789999999999999147, 30.40449935640660684, 2.004522720844263084 ) ) ;
#35093 = SHAPE_REPRESENTATION_RELATIONSHIP ( 'NONE' , 'NONE' ,  #15767, #23274 ) ;
#35094 = CYLINDRICAL_SURFACE ( 'NONE', #987, 4.309328216469825001 ) ;
#35095 = NEXT_ASSEMBLY_USAGE_OCCURRENCE ( 'NAUO1', ' ', ' ', #764, #13389, $ ) ;
#35096 = NEXT_ASSEMBLY_USAGE_OCCURRENCE ( 'NAUO2', ' ', ' ', #764, #22952, $ ) ;
#35097 = NEXT_ASSEMBLY_USAGE_OCCURRENCE ( 'NAUO3', ' ', ' ', #764, #30332, $ ) ;
#35098 = NEXT_ASSEMBLY_USAGE_OCCURRENCE ( 'NAUO4', ' ', ' ', #764, #30332, $ ) ;
#35099 = NEXT_ASSEMBLY_USAGE_OCCURRENCE ( 'NAUO5', ' ', ' ', #764, #25992, $ ) ;
#35100 = NEXT_ASSEMBLY_USAGE_OCCURRENCE ( 'NAUO6', ' ', ' ', #764, #329, $ ) ;
#35101 = NEXT_ASSEMBLY_USAGE_OCCURRENCE ( 'NAUO7', ' ', ' ', #764, #329, $ ) ;
#35102 = NEXT_ASSEMBLY_USAGE_OCCURRENCE ( 'NAUO8', ' ', ' ', #764, #16007, $ ) ;
#35103 = NEXT_ASSEMBLY_USAGE_OCCURRENCE ( 'NAUO9', ' ', ' ', #764, #18183, $ ) ;
#35104 = NEXT_ASSEMBLY_USAGE_OCCURRENCE ( 'NAUO10', ' ', ' ', #764, #31842, $ ) ;
#35105 = NEXT_ASSEMBLY_USAGE_OCCURRENCE ( 'NAUO11', ' ', ' ', #764, #31842, $ ) ;
#35106 = NEXT_ASSEMBLY_USAGE_OCCURRENCE ( 'NAUO12', ' ', ' ', #764, #32294, $ ) ;
#35107 = NEXT_ASSEMBLY_USAGE_OCCURRENCE ( 'NAUO13', ' ', ' ', #764, #21422, $ ) ;
#35108 = NEXT_ASSEMBLY_USAGE_OCCURRENCE ( 'NAUO14', ' ', ' ', #764, #21422, $ ) ;
#35109 = NEXT_ASSEMBLY_USAGE_OCCURRENCE ( 'NAUO15', ' ', ' ', #764, #21422, $ ) ;
#35110 = NEXT_ASSEMBLY_USAGE_OCCURRENCE ( 'NAUO16', ' ', ' ', #764, #21422, $ ) ;
#35111 = NEXT_ASSEMBLY_USAGE_OCCURRENCE ( 'NAUO17', ' ', ' ', #764, #21422, $ ) ;
#35112 = NEXT_ASSEMBLY_USAGE_OCCURRENCE ( 'NAUO18', ' ', ' ', #764, #21422, $ ) ;
#35113 = NEXT_ASSEMBLY_USAGE_OCCURRENCE ( 'NAUO19', ' ', ' ', #764, #21422, $ ) ;
#35114 = NEXT_ASSEMBLY_USAGE_OCCURRENCE ( 'NAUO20', ' ', ' ', #764, #21422, $ ) ;
#35115 = NEXT_ASSEMBLY_USAGE_OCCURRENCE ( 'NAUO21', ' ', ' ', #764, #21422, $ ) ;
#35116 = NEXT_ASSEMBLY_USAGE_OCCURRENCE ( 'NAUO22', ' ', ' ', #764, #21422, $ ) ;
#35117 = NEXT_ASSEMBLY_USAGE_OCCURRENCE ( 'NAUO23', ' ', ' ', #764, #21422, $ ) ;
#35118 = NEXT_ASSEMBLY_USAGE_OCCURRENCE ( 'NAUO24', ' ', ' ', #764, #21422, $ ) ;
#35119 = NEXT_ASSEMBLY_USAGE_OCCURRENCE ( 'NAUO25', ' ', ' ', #764, #21422, $ ) ;
#35120 = NEXT_ASSEMBLY_USAGE_OCCURRENCE ( 'NAUO26', ' ', ' ', #764, #21422, $ ) ;
#35121 = NEXT_ASSEMBLY_USAGE_OCCURRENCE ( 'NAUO27', ' ', ' ', #764, #21422, $ ) ;
#35122 = NEXT_ASSEMBLY_USAGE_OCCURRENCE ( 'NAUO28', ' ', ' ', #764, #21422, $ ) ;
#35123 = NEXT_ASSEMBLY_USAGE_OCCURRENCE ( 'NAUO29', ' ', ' ', #764, #21422, $ ) ;
#35124 = NEXT_ASSEMBLY_USAGE_OCCURRENCE ( 'NAUO30', ' ', ' ', #764, #21422, $ ) ;
#35125 = NEXT_ASSEMBLY_USAGE_OCCURRENCE ( 'NAUO31', ' ', ' ', #764, #21422, $ ) ;
#35126 = NEXT_ASSEMBLY_USAGE_OCCURRENCE ( 'NAUO32', ' ', ' ', #764, #21422, $ ) ;
#35127 = NEXT_ASSEMBLY_USAGE_OCCURRENCE ( 'NAUO33', ' ', ' ', #764, #21422, $ ) ;
#35128 = NEXT_ASSEMBLY_USAGE_OCCURRENCE ( 'NAUO34', ' ', ' ', #764, #21422, $ ) ;
#35129 = NEXT_ASSEMBLY_USAGE_OCCURRENCE ( 'NAUO35', ' ', ' ', #764, #21422, $ ) ;
#35130 = NEXT_ASSEMBLY_USAGE_OCCURRENCE ( 'NAUO36', ' ', ' ', #764, #21422, $ ) ;
#35131 = NEXT_ASSEMBLY_USAGE_OCCURRENCE ( 'NAUO37', ' ', ' ', #764, #21422, $ ) ;
#35132 = NEXT_ASSEMBLY_USAGE_OCCURRENCE ( 'NAUO38', ' ', ' ', #764, #21422, $ ) ;
#35133 = NEXT_ASSEMBLY_USAGE_OCCURRENCE ( 'NAUO39', ' ', ' ', #764, #21422, $ ) ;
#35134 = NEXT_ASSEMBLY_USAGE_OCCURRENCE ( 'NAUO40', ' ', ' ', #764, #21422, $ ) ;
#35135 = NEXT_ASSEMBLY_USAGE_OCCURRENCE ( 'NAUO41', ' ', ' ', #764, #21422, $ ) ;
#35136 = NEXT_ASSEMBLY_USAGE_OCCURRENCE ( 'NAUO42', ' ', ' ', #764, #21422, $ ) ;
#35137 = NEXT_ASSEMBLY_USAGE_OCCURRENCE ( 'NAUO43', ' ', ' ', #764, #21422, $ ) ;
#35138 = NEXT_ASSEMBLY_USAGE_OCCURRENCE ( 'NAUO44', ' ', ' ', #764, #21422, $ ) ;
#35139 = NEXT_ASSEMBLY_USAGE_OCCURRENCE ( 'NAUO45', ' ', ' ', #764, #21422, $ ) ;
#35140 = NEXT_ASSEMBLY_USAGE_OCCURRENCE ( 'NAUO46', ' ', ' ', #764, #21422, $ ) ;
#35141 = NEXT_ASSEMBLY_USAGE_OCCURRENCE ( 'NAUO47', ' ', ' ', #764, #21422, $ ) ;
#35142 = NEXT_ASSEMBLY_USAGE_OCCURRENCE ( 'NAUO48', ' ', ' ', #764, #21422, $ ) ;
#35143 = NEXT_ASSEMBLY_USAGE_OCCURRENCE ( 'NAUO49', ' ', ' ', #764, #21422, $ ) ;
#35144 = NEXT_ASSEMBLY_USAGE_OCCURRENCE ( 'NAUO50', ' ', ' ', #764, #21422, $ ) ;
#35145 = NEXT_ASSEMBLY_USAGE_OCCURRENCE ( 'NAUO51', ' ', ' ', #764, #21422, $ ) ;
#35146 = NEXT_ASSEMBLY_USAGE_OCCURRENCE ( 'NAUO52', ' ', ' ', #764, #21422, $ ) ;
#35147 = NEXT_ASSEMBLY_USAGE_OCCURRENCE ( 'NAUO53', ' ', ' ', #764, #21422, $ ) ;
#35148 = NEXT_ASSEMBLY_USAGE_OCCURRENCE ( 'NAUO54', ' ', ' ', #764, #21422, $ ) ;
#35149 = NEXT_ASSEMBLY_USAGE_OCCURRENCE ( 'NAUO55', ' ', ' ', #764, #21422, $ ) ;
#35150 = NEXT_ASSEMBLY_USAGE_OCCURRENCE ( 'NAUO56', ' ', ' ', #764, #21422, $ ) ;
#35151 = NEXT_ASSEMBLY_USAGE_OCCURRENCE ( 'NAUO57', ' ', ' ', #764, #21422, $ ) ;
#35152 = NEXT_ASSEMBLY_USAGE_OCCURRENCE ( 'NAUO58', ' ', ' ', #764, #21422, $ ) ;
#35153 = NEXT_ASSEMBLY_USAGE_OCCURRENCE ( 'NAUO59', ' ', ' ', #764, #21422, $ ) ;
#35154 = NEXT_ASSEMBLY_USAGE_OCCURRENCE ( 'NAUO60', ' ', ' ', #764, #21422, $ ) ;
#35155 = NEXT_ASSEMBLY_USAGE_OCCURRENCE ( 'NAUO61', ' ', ' ', #764, #21422, $ ) ;
#35156 = NEXT_ASSEMBLY_USAGE_OCCURRENCE ( 'NAUO62', ' ', ' ', #764, #21422, $ ) ;
#35157 = NEXT_ASSEMBLY_USAGE_OCCURRENCE ( 'NAUO63', ' ', ' ', #764, #21422, $ ) ;
#35158 = NEXT_ASSEMBLY_USAGE_OCCURRENCE ( 'NAUO64', ' ', ' ', #764, #21422, $ ) ;
#35159 = NEXT_ASSEMBLY_USAGE_OCCURRENCE ( 'NAUO65', ' ', ' ', #764, #21422, $ ) ;
#35160 = NEXT_ASSEMBLY_USAGE_OCCURRENCE ( 'NAUO66', ' ', ' ', #764, #21422, $ ) ;
#35161 = NEXT_ASSEMBLY_USAGE_OCCURRENCE ( 'NAUO67', ' ', ' ', #764, #21422, $ ) ;
#35162 = NEXT_ASSEMBLY_USAGE_OCCURRENCE ( 'NAUO68', ' ', ' ', #764, #21422, $ ) ;
#35163 = NEXT_ASSEMBLY_USAGE_OCCURRENCE ( 'NAUO69', ' ', ' ', #764, #21422, $ ) ;
#35164 = NEXT_ASSEMBLY_USAGE_OCCURRENCE ( 'NAUO70', ' ', ' ', #764, #21422, $ ) ;
#35165 = NEXT_ASSEMBLY_USAGE_OCCURRENCE ( 'NAUO71', ' ', ' ', #764, #21422, $ ) ;
#35166 = NEXT_ASSEMBLY_USAGE_OCCURRENCE ( 'NAUO72', ' ', ' ', #764, #21422, $ ) ;
#35167 = NEXT_ASSEMBLY_USAGE_OCCURRENCE ( 'NAUO73', ' ', ' ', #764, #21422, $ ) ;
#35168 = NEXT_ASSEMBLY_USAGE_OCCURRENCE ( 'NAUO74', ' ', ' ', #764, #21422, $ ) ;
#35169 = NEXT_ASSEMBLY_USAGE_OCCURRENCE ( 'NAUO75', ' ', ' ', #764, #21422, $ ) ;
#35170 = NEXT_ASSEMBLY_USAGE_OCCURRENCE ( 'NAUO76', ' ', ' ', #764, #21422, $ ) ;
#35171 = NEXT_ASSEMBLY_USAGE_OCCURRENCE ( 'NAUO77', ' ', ' ', #764, #21422, $ ) ;
#35172 = NEXT_ASSEMBLY_USAGE_OCCURRENCE ( 'NAUO78', ' ', ' ', #764, #21422, $ ) ;
#35173 = NEXT_ASSEMBLY_USAGE_OCCURRENCE ( 'NAUO79', ' ', ' ', #764, #21422, $ ) ;
#35174 = NEXT_ASSEMBLY_USAGE_OCCURRENCE ( 'NAUO80', ' ', ' ', #764, #21422, $ ) ;
#35175 = NEXT_ASSEMBLY_USAGE_OCCURRENCE ( 'NAUO81', ' ', ' ', #764, #21422, $ ) ;
#35176 = NEXT_ASSEMBLY_USAGE_OCCURRENCE ( 'NAUO82', ' ', ' ', #764, #32294, $ ) ;
#35177 = NEXT_ASSEMBLY_USAGE_OCCURRENCE ( 'NAUO83', ' ', ' ', #764, #32294, $ ) ;
#35178 = NEXT_ASSEMBLY_USAGE_OCCURRENCE ( 'NAUO84', ' ', ' ', #764, #32294, $ ) ;
#35179 = NEXT_ASSEMBLY_USAGE_OCCURRENCE ( 'NAUO85', ' ', ' ', #764, #32294, $ ) ;
#35180 = NEXT_ASSEMBLY_USAGE_OCCURRENCE ( 'NAUO86', ' ', ' ', #764, #32294, $ ) ;
#35181 = NEXT_ASSEMBLY_USAGE_OCCURRENCE ( 'NAUO87', ' ', ' ', #764, #32294, $ ) ;
#35182 = NEXT_ASSEMBLY_USAGE_OCCURRENCE ( 'NAUO88', ' ', ' ', #764, #32294, $ ) ;
#35183 = NEXT_ASSEMBLY_USAGE_OCCURRENCE ( 'NAUO89', ' ', ' ', #764, #32294, $ ) ;
#35184 = NEXT_ASSEMBLY_USAGE_OCCURRENCE ( 'NAUO90', ' ', ' ', #764, #32294, $ ) ;
#35185 = NEXT_ASSEMBLY_USAGE_OCCURRENCE ( 'NAUO91', ' ', ' ', #764, #32294, $ ) ;
#35186 = NEXT_ASSEMBLY_USAGE_OCCURRENCE ( 'NAUO92', ' ', ' ', #764, #32294, $ ) ;
#35187 = NEXT_ASSEMBLY_USAGE_OCCURRENCE ( 'NAUO93', ' ', ' ', #764, #32294, $ ) ;
#35188 = NEXT_ASSEMBLY_USAGE_OCCURRENCE ( 'NAUO94', ' ', ' ', #764, #32294, $ ) ;
#35189 = NEXT_ASSEMBLY_USAGE_OCCURRENCE ( 'NAUO95', ' ', ' ', #764, #32294, $ ) ;
#35190 = NEXT_ASSEMBLY_USAGE_OCCURRENCE ( 'NAUO96', ' ', ' ', #764, #32294, $ ) ;
#35191 = NEXT_ASSEMBLY_USAGE_OCCURRENCE ( 'NAUO97', ' ', ' ', #764, #32294, $ ) ;
#35192 = NEXT_ASSEMBLY_USAGE_OCCURRENCE ( 'NAUO98', ' ', ' ', #764, #32294, $ ) ;
#35193 = NEXT_ASSEMBLY_USAGE_OCCURRENCE ( 'NAUO99', ' ', ' ', #764, #32294, $ ) ;
#35194 = NEXT_ASSEMBLY_USAGE_OCCURRENCE ( 'NAUO100', ' ', ' ', #764, #32294, $ ) ;
#35195 = NEXT_ASSEMBLY_USAGE_OCCURRENCE ( 'NAUO101', ' ', ' ', #764, #32294, $ ) ;
#35196 = NEXT_ASSEMBLY_USAGE_OCCURRENCE ( 'NAUO102', ' ', ' ', #764, #32294, $ ) ;
#35197 = NEXT_ASSEMBLY_USAGE_OCCURRENCE ( 'NAUO103', ' ', ' ', #764, #32294, $ ) ;
#35198 = NEXT_ASSEMBLY_USAGE_OCCURRENCE ( 'NAUO104', ' ', ' ', #764, #32294, $ ) ;
#35199 = NEXT_ASSEMBLY_USAGE_OCCURRENCE ( 'NAUO105', ' ', ' ', #764, #32294, $ ) ;
#35200 = NEXT_ASSEMBLY_USAGE_OCCURRENCE ( 'NAUO106', ' ', ' ', #764, #32294, $ ) ;
#35201 = NEXT_ASSEMBLY_USAGE_OCCURRENCE ( 'NAUO107', ' ', ' ', #764, #32294, $ ) ;
#35202 = NEXT_ASSEMBLY_USAGE_OCCURRENCE ( 'NAUO108', ' ', ' ', #764, #32294, $ ) ;
#35203 = NEXT_ASSEMBLY_USAGE_OCCURRENCE ( 'NAUO109', ' ', ' ', #764, #32294, $ ) ;
#35204 = NEXT_ASSEMBLY_USAGE_OCCURRENCE ( 'NAUO110', ' ', ' ', #764, #32294, $ ) ;
#35205 = NEXT_ASSEMBLY_USAGE_OCCURRENCE ( 'NAUO111', ' ', ' ', #764, #32294, $ ) ;
#35206 = NEXT_ASSEMBLY_USAGE_OCCURRENCE ( 'NAUO112', ' ', ' ', #764, #32294, $ ) ;
#35207 = NEXT_ASSEMBLY_USAGE_OCCURRENCE ( 'NAUO113', ' ', ' ', #764, #32294, $ ) ;
#35208 = NEXT_ASSEMBLY_USAGE_OCCURRENCE ( 'NAUO114', ' ', ' ', #764, #32294, $ ) ;
#35209 = NEXT_ASSEMBLY_USAGE_OCCURRENCE ( 'NAUO115', ' ', ' ', #764, #32294, $ ) ;
#35210 = NEXT_ASSEMBLY_USAGE_OCCURRENCE ( 'NAUO116', ' ', ' ', #764, #32294, $ ) ;
#35211 = NEXT_ASSEMBLY_USAGE_OCCURRENCE ( 'NAUO117', ' ', ' ', #764, #32294, $ ) ;
#35212 = NEXT_ASSEMBLY_USAGE_OCCURRENCE ( 'NAUO118', ' ', ' ', #764, #32294, $ ) ;
#35213 = NEXT_ASSEMBLY_USAGE_OCCURRENCE ( 'NAUO119', ' ', ' ', #764, #32294, $ ) ;
#35214 = NEXT_ASSEMBLY_USAGE_OCCURRENCE ( 'NAUO120', ' ', ' ', #764, #32294, $ ) ;
#35215 = NEXT_ASSEMBLY_USAGE_OCCURRENCE ( 'NAUO121', ' ', ' ', #764, #32294, $ ) ;
#35216 = NEXT_ASSEMBLY_USAGE_OCCURRENCE ( 'NAUO122', ' ', ' ', #764, #32294, $ ) ;
#35217 = NEXT_ASSEMBLY_USAGE_OCCURRENCE ( 'NAUO123', ' ', ' ', #764, #32294, $ ) ;
#35218 = NEXT_ASSEMBLY_USAGE_OCCURRENCE ( 'NAUO124', ' ', ' ', #764, #32294, $ ) ;
#35219 = NEXT_ASSEMBLY_USAGE_OCCURRENCE ( 'NAUO125', ' ', ' ', #764, #32294, $ ) ;
#35220 = NEXT_ASSEMBLY_USAGE_OCCURRENCE ( 'NAUO126', ' ', ' ', #764, #32294, $ ) ;
#35221 = NEXT_ASSEMBLY_USAGE_OCCURRENCE ( 'NAUO127', ' ', ' ', #764, #32294, $ ) ;
#35222 = NEXT_ASSEMBLY_USAGE_OCCURRENCE ( 'NAUO128', ' ', ' ', #764, #32294, $ ) ;
#35223 = NEXT_ASSEMBLY_USAGE_OCCURRENCE ( 'NAUO129', ' ', ' ', #764, #32294, $ ) ;
#35224 = NEXT_ASSEMBLY_USAGE_OCCURRENCE ( 'NAUO130', ' ', ' ', #764, #32294, $ ) ;
#35225 = NEXT_ASSEMBLY_USAGE_OCCURRENCE ( 'NAUO131', ' ', ' ', #764, #32294, $ ) ;
#35226 = NEXT_ASSEMBLY_USAGE_OCCURRENCE ( 'NAUO132', ' ', ' ', #764, #32294, $ ) ;
#35227 = NEXT_ASSEMBLY_USAGE_OCCURRENCE ( 'NAUO133', ' ', ' ', #764, #32294, $ ) ;
#35228 = NEXT_ASSEMBLY_USAGE_OCCURRENCE ( 'NAUO134', ' ', ' ', #764, #32294, $ ) ;
#35229 = NEXT_ASSEMBLY_USAGE_OCCURRENCE ( 'NAUO135', ' ', ' ', #764, #32294, $ ) ;
#35230 = NEXT_ASSEMBLY_USAGE_OCCURRENCE ( 'NAUO136', ' ', ' ', #764, #32294, $ ) ;
#35231 = NEXT_ASSEMBLY_USAGE_OCCURRENCE ( 'NAUO137', ' ', ' ', #764, #32294, $ ) ;
#35232 = NEXT_ASSEMBLY_USAGE_OCCURRENCE ( 'NAUO138', ' ', ' ', #764, #32294, $ ) ;
#35233 = NEXT_ASSEMBLY_USAGE_OCCURRENCE ( 'NAUO139', ' ', ' ', #764, #32294, $ ) ;
#35234 = NEXT_ASSEMBLY_USAGE_OCCURRENCE ( 'NAUO140', ' ', ' ', #764, #32294, $ ) ;
#35235 = NEXT_ASSEMBLY_USAGE_OCCURRENCE ( 'NAUO141', ' ', ' ', #764, #32294, $ ) ;
#35236 = NEXT_ASSEMBLY_USAGE_OCCURRENCE ( 'NAUO142', ' ', ' ', #764, #32294, $ ) ;
#35237 = NEXT_ASSEMBLY_USAGE_OCCURRENCE ( 'NAUO143', ' ', ' ', #764, #32294, $ ) ;
#35238 = NEXT_ASSEMBLY_USAGE_OCCURRENCE ( 'NAUO144', ' ', ' ', #764, #32294, $ ) ;
#35239 = NEXT_ASSEMBLY_USAGE_OCCURRENCE ( 'NAUO145', ' ', ' ', #764, #32294, $ ) ;
#35240 = NEXT_ASSEMBLY_USAGE_OCCURRENCE ( 'NAUO146', ' ', ' ', #764, #32294, $ ) ;
#35241 = NEXT_ASSEMBLY_USAGE_OCCURRENCE ( 'NAUO147', ' ', ' ', #764, #32294, $ ) ;
#35242 = NEXT_ASSEMBLY_USAGE_OCCURRENCE ( 'NAUO148', ' ', ' ', #764, #32294, $ ) ;
#35243 = NEXT_ASSEMBLY_USAGE_OCCURRENCE ( 'NAUO149', ' ', ' ', #764, #32294, $ ) ;
#35244 = NEXT_ASSEMBLY_USAGE_OCCURRENCE ( 'NAUO150', ' ', ' ', #764, #27721, $ ) ;
#35245 = NEXT_ASSEMBLY_USAGE_OCCURRENCE ( 'NAUO151', ' ', ' ', #764, #27721, $ ) ;
#35246 = NEXT_ASSEMBLY_USAGE_OCCURRENCE ( 'NAUO152', ' ', ' ', #764, #27721, $ ) ;
#35247 = NEXT_ASSEMBLY_USAGE_OCCURRENCE ( 'NAUO153', ' ', ' ', #764, #27721, $ ) ;
#35248=COLOUR_RGB('Dark Blue',0.08,0.2,0.34);
#35249=FILL_AREA_STYLE_COLOUR('',#35248);
#35250=FILL_AREA_STYLE('',(#35249));
#35251=SURFACE_STYLE_FILL_AREA(#35250);
#35252=SURFACE_SIDE_STYLE('',(#35251));
#35253=SURFACE_STYLE_USAGE(.BOTH.,#35252);
#35254=PRESENTATION_STYLE_ASSIGNMENT((#35253));
#35255=COLOUR_RGB('Light Blue',0.38,0.62,0.78);
#35256=FILL_AREA_STYLE_COLOUR('',#35255);
#35257=FILL_AREA_STYLE('',(#35256));
#35258=SURFACE_STYLE_FILL_AREA(#35257);
#35259=SURFACE_SIDE_STYLE('',(#35258));
#35260=SURFACE_STYLE_USAGE(.BOTH.,#35259);
#35261=PRESENTATION_STYLE_ASSIGNMENT((#35260));
#35262=COLOUR_RGB('Sky Blue',0.24,0.69,0.87);
#35263=FILL_AREA_STYLE_COLOUR('',#35262);
#35264=FILL_AREA_STYLE('',(#35263));
#35265=SURFACE_STYLE_FILL_AREA(#35264);
#35266=SURFACE_SIDE_STYLE('',(#35265));
#35267=SURFACE_STYLE_USAGE(.BOTH.,#35266);
#35268=PRESENTATION_STYLE_ASSIGNMENT((#35267));
#35269=COLOUR_RGB('Grey',0.48,0.52,0.57);
#35270=FILL_AREA_STYLE_COLOUR('',#35269);
#35271=FILL_AREA_STYLE('',(#35270));
#35272=SURFACE_STYLE_FILL_AREA(#35271);
#35273=SURFACE_SIDE_STYLE('',(#35272));
#35274=SURFACE_STYLE_USAGE(.BOTH.,#35273);
#35275=PRESENTATION_STYLE_ASSIGNMENT((#35274));
#35276=COLOUR_RGB('Black',0.12,0.14,0.17);
#35277=FILL_AREA_STYLE_COLOUR('',#35276);
#35278=FILL_AREA_STYLE('',(#35277));
#35279=SURFACE_STYLE_FILL_AREA(#35278);
#35280=SURFACE_SIDE_STYLE('',(#35279));
#35281=SURFACE_STYLE_USAGE(.BOTH.,#35280);
#35282=PRESENTATION_STYLE_ASSIGNMENT((#35281));
#35283=COLOUR_RGB('Off White',0.89,0.88,0.83);
#35284=FILL_AREA_STYLE_COLOUR('',#35283);
#35285=FILL_AREA_STYLE('',(#35284));
#35286=SURFACE_STYLE_FILL_AREA(#35285);
#35287=SURFACE_SIDE_STYLE('',(#35286));
#35288=SURFACE_STYLE_USAGE(.BOTH.,#35287);
#35289=PRESENTATION_STYLE_ASSIGNMENT((#35288));
ENDSEC;
END-ISO-10303-21;
